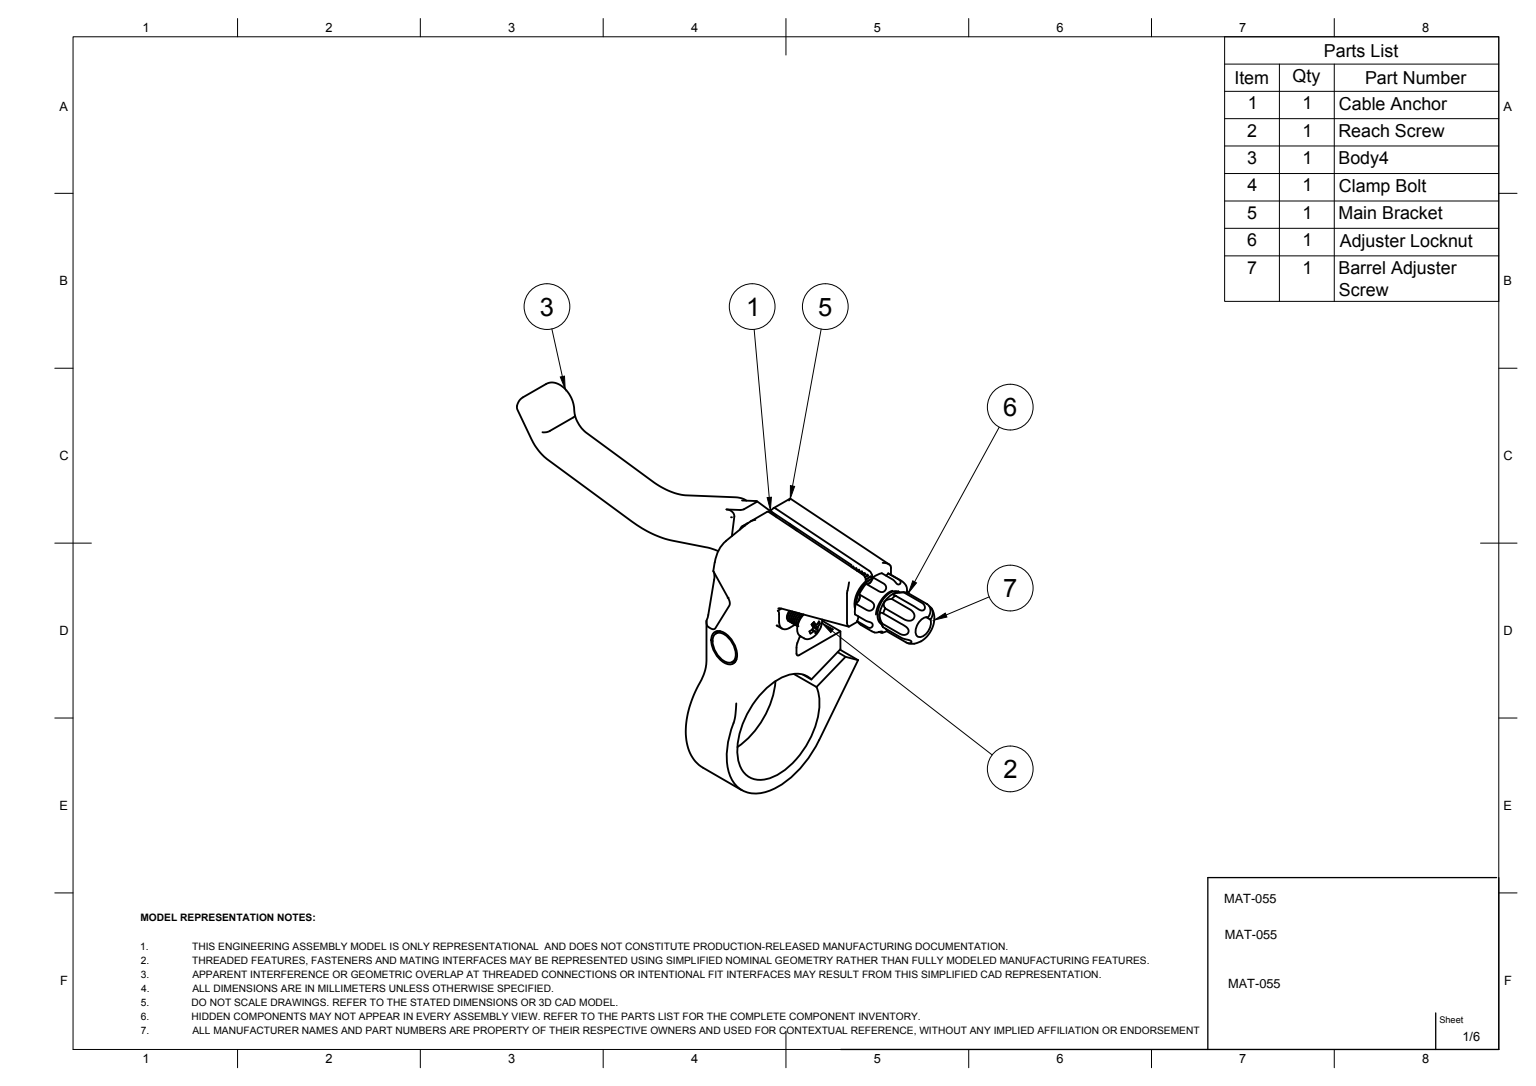
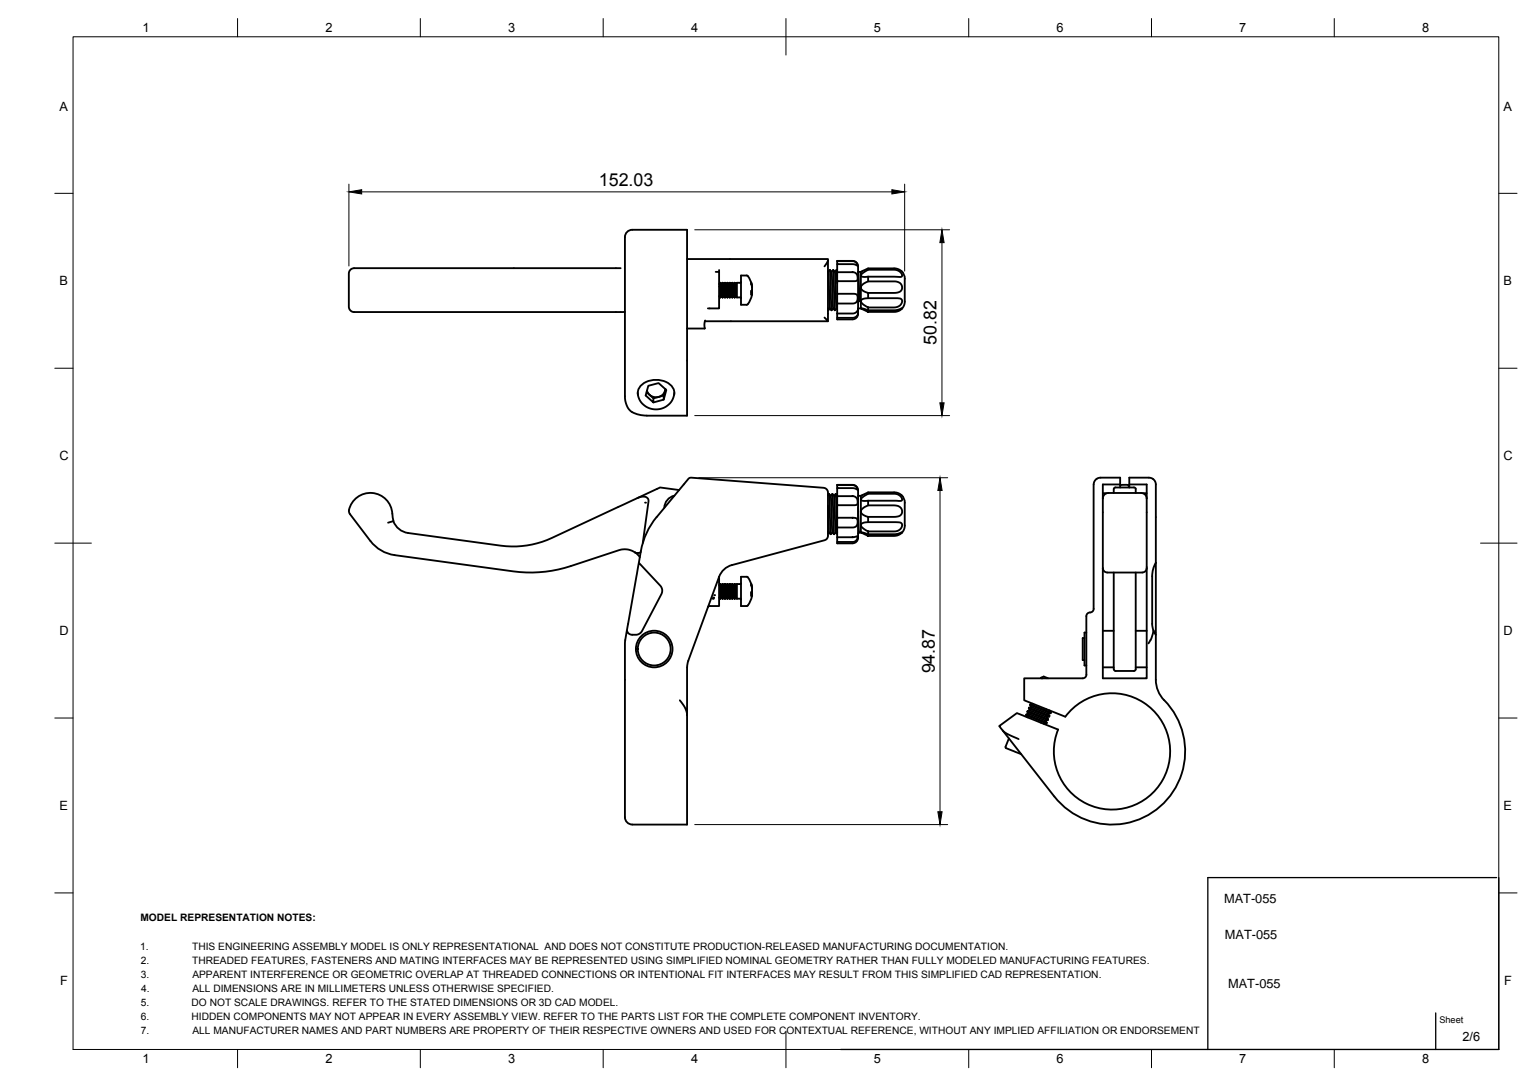
ISO-10303-21;
HEADER;
FILE_DESCRIPTION (('STEP AP214'),
    '1' );
FILE_NAME ('MAT-055',
    '2026-10-30T09:41:00',
    ( '' ),
    ( '' ),
    'SwSTEP 2.0',
    'SolidWorks 2020',
    '' );
FILE_SCHEMA (( 'AUTOMOTIVE_DESIGN' ));
ENDSEC;

DATA;
#1 = CARTESIAN_POINT ( 'NONE',  ( 110.9687390045248350, -9.868328341294098749, -11.32035403202665869 ) ) ;
#2 = LINE ( 'NONE', #2744, #42488 ) ;
#3 = ORIENTED_EDGE ( 'NONE', *, *, #32082, .F. ) ;
#4 = CARTESIAN_POINT ( 'NONE',  ( 113.1933481442453058, -4.089484607189486809, -7.948022111789456723 ) ) ;
#5 = CARTESIAN_POINT ( 'NONE',  ( 112.6260814775786514, -9.261995988541697145, -16.69588392320189030 ) ) ;
#6 = CARTESIAN_POINT ( 'NONE',  ( 122.0994348109119443, 0.9020085738987339008, -11.91225656197089222 ) ) ;
#7 = CARTESIAN_POINT ( 'NONE',  ( 116.4267681442453153, -6.222761293078241884, -8.102969835052219238 ) ) ;
#8 = DIRECTION ( 'NONE',  ( 1.000000000000000000, 0.000000000000000000, -0.000000000000000000 ) ) ;
#9 = CARTESIAN_POINT ( 'NONE',  ( 120.6245414775786458, -9.988377603198976828, -10.36322818467138340 ) ) ;
#10 = FACE_OUTER_BOUND ( 'NONE', #7467, .T. ) ;
#11 = CARTESIAN_POINT ( 'NONE',  ( 121.3619881442452879, -5.574606645277164318, -18.38911715685844683 ) ) ;
#12 = ORIENTED_EDGE ( 'NONE', *, *, #37026, .T. ) ;
#13 = CARTESIAN_POINT ( 'NONE',  ( 69.69189222814998175, -41.76310523276723785, -24.39321520033831447 ) ) ;
#14 = CIRCLE ( 'NONE', #29859, 2.000000000000000444 ) ;
#15 = CARTESIAN_POINT ( 'NONE',  ( 117.5613014775786525, 0.9020085738987339008, -11.91225656197089222 ) ) ;
#16 = CARTESIAN_POINT ( 'NONE',  ( 89.67401078471493747, -27.84333996136784961, -14.15691383771150136 ) ) ;
#17 = VERTEX_POINT ( 'NONE', #2774 ) ;
#18 = CARTESIAN_POINT ( 'NONE',  ( 123.0077516859119839, -9.665098340737509730, -17.37397104707595474 ) ) ;
#19 = CARTESIAN_POINT ( 'NONE',  ( 137.1799701741921922, -1.245005990108144500, -9.487437202584745322 ) ) ;
#20 = CARTESIAN_POINT ( 'NONE',  ( 121.4754414775786131, -8.166667518702819706, -8.995218007635861213 ) ) ;
#21 = CARTESIAN_POINT ( 'NONE',  ( 106.2459265045248173, -7.250697342233347165, -19.15521520033831138 ) ) ;
#22 = CARTESIAN_POINT ( 'NONE',  ( 119.6034614775786196, -3.505236298600246325, -18.68346056562440793 ) ) ;
#23 = ORIENTED_EDGE ( 'NONE', *, *, #16097, .T. ) ;
#24 = ORIENTED_EDGE ( 'NONE', *, *, #31128, .T. ) ;
#25 = CARTESIAN_POINT ( 'NONE',  ( 115.3489614775786407, -9.261995988541697145, -16.69588392320189030 ) ) ;
#26 = CYLINDRICAL_SURFACE ( 'NONE', #29939, 3.000000000000002665 ) ;
#27 = AXIS2_PLACEMENT_3D ( 'NONE', #14609, #30094, #23021 ) ;
#28 = DIRECTION ( 'NONE',  ( 0.000000000000000000, 0.000000000000000000, -1.000000000000000000 ) ) ;
#29 = EDGE_CURVE ( 'NONE', #24368, #33578, #9787, .T. ) ;
#30 = LINE ( 'NONE', #27854, #4652 ) ;
#31 = CARTESIAN_POINT ( 'NONE',  ( 121.5321681442453183, -9.988377603198976828, -10.36322818467138340 ) ) ;
#32 = CARTESIAN_POINT ( 'NONE',  ( 74.32979735608419958, -48.45188957854135481, -10.89321520033831447 ) ) ;
#33 = LINE ( 'NONE', #17589, #1125 ) ;
#34 = CARTESIAN_POINT ( 'NONE',  ( 122.3830681442452857, -8.166667518702819706, -8.995218007635861213 ) ) ;
#36 = CARTESIAN_POINT ( 'NONE',  ( 118.7525614775786380, -1.833838273342659253, -17.42832698103878286 ) ) ;
#35 = CARTESIAN_POINT ( 'NONE',  ( 120.3409081442453044, -0.4660016031367893996, -10.09054647747474043 ) ) ;
#37 = CARTESIAN_POINT ( 'NONE',  ( 121.2485348109119769, -8.899110576539710493, -16.42337572283490132 ) ) ;
#38 = DIRECTION ( 'NONE',  ( 0.9609149988134837450, -0.1028163501681639419, 0.2570431154366518145 ) ) ;
#39 = CARTESIAN_POINT ( 'NONE',  ( 114.9518748109119883, -1.834011780172310813, -8.268836392978581529 ) ) ;
#40 = EDGE_LOOP ( 'NONE', ( #5265, #23177, #27838, #18578 ) ) ;
#41 = CARTESIAN_POINT ( 'NONE',  ( 116.0834518517486771, -0.01906416985213849058, -12.14321520033831625 ) ) ;
#42 = CARTESIAN_POINT ( 'NONE',  ( 106.5237390045248418, 0.8980012041604421569, -15.77991374673208469 ) ) ;
#43 = CARTESIAN_POINT ( 'NONE',  ( 107.8433483795247838, -8.402594152722688392, -16.93181055722141792 ) ) ;
#44 = CARTESIAN_POINT ( 'NONE',  ( 105.4819421295248247, 0.8980012041604618078, -13.39321520033831447 ) ) ;
#45 = CARTESIAN_POINT ( 'NONE',  ( 125.3895814775786448, -7.893985811506177619, -18.51759400769804742 ) ) ;
#46 = CARTESIAN_POINT ( 'NONE',  ( 125.5597614775786326, -7.894159318335828068, -9.358103419637847864 ) ) ;
#47 = ORIENTED_EDGE ( 'NONE', *, *, #34668, .T. ) ;
#48 = CARTESIAN_POINT ( 'NONE',  ( 125.2761281442453054, -10.63000616557722466, -14.87417383870573495 ) ) ;
#49 = CARTESIAN_POINT ( 'NONE',  ( 111.3854577545248645, -7.250697342233347165, -7.631215200338321125 ) ) ;
#50 = DIRECTION ( 'NONE',  ( 0.000000000000000000, 0.000000000000000000, -1.000000000000000000 ) ) ;
#51 = ADVANCED_FACE ( 'NONE', ( #30593 ), #44511, .T. ) ;
#52 = CARTESIAN_POINT ( 'NONE',  ( 122.7234281442452755, -5.638512984488999180, -18.83840828888717311 ) ) ;
#53 = CARTESIAN_POINT ( 'NONE',  ( 125.8433948109119456, -1.834011780172310813, -8.268836392978581529 ) ) ;
#54 = CARTESIAN_POINT ( 'NONE',  ( 111.7184548109119788, -9.261995988541697145, -16.69588392320189030 ) ) ;
#55 = CARTESIAN_POINT ( 'NONE',  ( 116.0388171295248014, -10.62599879583958540, -13.39321520033831447 ) ) ;
#56 = CARTESIAN_POINT ( 'NONE',  ( 106.8710046295248759, -4.863998795839590272, -7.631215200338315796 ) ) ;
#57 = ORIENTED_EDGE ( 'NONE', *, *, #39925, .T. ) ;
#58 = DIRECTION ( 'NONE',  ( -0.000000000000000000, -0.9284778069183721172, -0.3713878862591650232 ) ) ;
#59 = AXIS2_PLACEMENT_3D ( 'NONE', #1011, #14251, #21539 ) ;
#60 = CARTESIAN_POINT ( 'NONE',  ( 116.8238548109119819, -5.574606645277164318, -18.38911715685844683 ) ) ;
#61 = CARTESIAN_POINT ( 'NONE',  ( 112.6260814775786514, -9.261995988541697145, -16.69588392320189030 ) ) ;
#62 = CARTESIAN_POINT ( 'NONE',  ( 115.7610046295247912, -4.863998795839590272, -7.631215200338315796 ) ) ;
#63 = CARTESIAN_POINT ( 'NONE',  ( 108.3295202545248657, 0.1403307496149616695, -11.32035403202665336 ) ) ;
#64 = AXIS2_PLACEMENT_3D ( 'NONE', #36243, #40129, #40585 ) ;
#65 = CARTESIAN_POINT ( 'NONE',  ( 120.9081748109119872, -4.153390946401325223, -8.397313243818185668 ) ) ;
#66 = CARTESIAN_POINT ( 'NONE',  ( 115.1787814775786387, -0.1624402480850797581, -16.17319339645315424 ) ) ;
#67 = CARTESIAN_POINT ( 'NONE',  ( 112.1155414775786454, -10.15424416112533912, -14.75197769757731336 ) ) ;
#68 = ORIENTED_EDGE ( 'NONE', *, *, #40399, .T. ) ;
#69 = CARTESIAN_POINT ( 'NONE',  ( 121.4103298109119748, -7.200787124940443817, -17.81845355600750835 ) ) ;
#70 = CARTESIAN_POINT ( 'NONE',  ( 124.5059548109119731, -5.999156839134619723, -18.26265215102738892 ) ) ;
#71 = CARTESIAN_POINT ( 'NONE',  ( 112.3991748109119868, -1.833838273342658809, -17.42832698103878286 ) ) ;
#72 = ORIENTED_EDGE ( 'NONE', *, *, #6315, .T. ) ;
#73 = CARTESIAN_POINT ( 'NONE',  ( 126.4750299824193007, -9.298013242772034559, -15.96981777986906970 ) ) ;
#74 = CARTESIAN_POINT ( 'NONE',  ( 112.6356140045247827, 0.1403307496149616695, -15.46607636864997204 ) ) ;
#75 = ORIENTED_EDGE ( 'NONE', *, *, #33478, .T. ) ;
#76 = AXIS2_PLACEMENT_3D ( 'NONE', #7945, #18211, #24609 ) ;
#77 = CARTESIAN_POINT ( 'NONE',  ( 116.8238548109119819, -5.574606645277164318, -18.38911715685844683 ) ) ;
#78 = CARTESIAN_POINT ( 'NONE',  ( 113.1933481442453058, -5.574606645277164318, -18.38911715685844683 ) ) ;
#79 = CARTESIAN_POINT ( 'NONE',  ( 112.8721930757767495, -0.9924539043446216624, -17.29976612834909133 ) ) ;
#80 = CARTESIAN_POINT ( 'NONE',  ( 123.7717360609119623, -3.387241619883791355, -18.17469012370385073 ) ) ;
#81 = ORIENTED_EDGE ( 'NONE', *, *, #25738, .F. ) ;
#82 = DIRECTION ( 'NONE',  ( 0.9609149988134837450, -0.1028163501681639419, 0.2570431154366518145 ) ) ;
#83 = CARTESIAN_POINT ( 'NONE',  ( 86.34560043013698305, -9.320000780048239619, -16.89321520033831447 ) ) ;
#84 = B_SPLINE_CURVE_WITH_KNOTS ( 'NONE', 3,
 ( #40412, #43376, #5506, #23076, #29462, #30146, #44061, #26048, #15786, #12373 ),
 .UNSPECIFIED., .F., .F.,
 ( 4, 2, 2, 2, 4 ),
 ( 0.000000000000000000, 0.0003215953659093761900, 0.0006431907318187523800, 0.0009647860977281285701, 0.001286381463637504760 ),
 .UNSPECIFIED. ) ;
#85 = CARTESIAN_POINT ( 'NONE',  ( 106.4542858795248179, -8.402594152722688392, -9.854619843455216355 ) ) ;
#86 = B_SPLINE_CURVE_WITH_KNOTS ( 'NONE', 3,
 ( #37430, #6200, #27183, #20122 ),
 .UNSPECIFIED., .F., .F.,
 ( 4, 4 ),
 ( 7.175310251266321521E-15, 2.533189092146110195E-06 ),
 .UNSPECIFIED. ) ;
#87 = FACE_OUTER_BOUND ( 'NONE', #1657, .T. ) ;
#88 = AXIS2_PLACEMENT_3D ( 'NONE', #42203, #35787, #10965 ) ;
#89 = CARTESIAN_POINT ( 'NONE',  ( 124.5954081442453116, -6.222761293078241884, -8.102969835052219238 ) ) ;
#90 = CARTESIAN_POINT ( 'NONE',  ( 116.8805814775786445, -3.505236298600246325, -18.68346056562440793 ) ) ;
#91 = CARTESIAN_POINT ( 'NONE',  ( 78.69189222814998175, -49.76310523276723785, -23.89321520033831803 ) ) ;
#92 = ORIENTED_EDGE ( 'NONE', *, *, #23975, .F. ) ;
#93 = CARTESIAN_POINT ( 'NONE',  ( 71.02242295334774269, -99.02728775972636299, -55.91838671430374319 ) ) ;
#94 = CARTESIAN_POINT ( 'NONE',  ( 117.0507614775786465, 0.1319031606808879209, -14.10382304977623669 ) ) ;
#95 = CARTESIAN_POINT ( 'NONE',  ( 119.7434548109119703, -3.132014511563818271, -18.68827187929387179 ) ) ;
#96 = CARTESIAN_POINT ( 'NONE',  ( 85.28386362106600416, -27.88924328735366132, -8.828750294274950505 ) ) ;
#97 = CARTESIAN_POINT ( 'NONE',  ( 125.5030348109119558, -3.383040157471821630, -19.15922257007629170 ) ) ;
#98 = EDGE_CURVE ( 'NONE', #12720, #5950, #1643, .T. ) ;
#99 = CARTESIAN_POINT ( 'NONE',  ( 113.5337081442453240, -9.261995988541697145, -16.69588392320189030 ) ) ;
#100 = ORIENTED_EDGE ( 'NONE', *, *, #14497, .T. ) ;
#101 = CARTESIAN_POINT ( 'NONE',  ( 112.7962614775786676, -3.383040157471821630, -19.15922257007629170 ) ) ;
#102 = CARTESIAN_POINT ( 'NONE',  ( 114.4980614775786592, -7.893985811506184724, -18.51759400769803676 ) ) ;
#103 = CARTESIAN_POINT ( 'NONE',  ( 111.6632702545248605, -10.62599879583958717, -15.77991374673208469 ) ) ;
#104 = CARTESIAN_POINT ( 'NONE',  ( 112.3424481442453384, -6.344957434206662583, -7.627207830600332805 ) ) ;
#105 = CARTESIAN_POINT ( 'NONE',  ( 114.4980614775786592, -7.893985811506177619, -18.51759400769804742 ) ) ;
#106 = CARTESIAN_POINT ( 'NONE',  ( 124.3685014775786328, 0.4262465694468514643, -12.03445270309931736 ) ) ;
#107 = CARTESIAN_POINT ( 'NONE',  ( 69.36136150295220659, -60.18712133882883819, -34.17284023871924603 ) ) ;
#108 = CARTESIAN_POINT ( 'NONE',  ( 108.5378796295247810, -4.863998795839590272, -8.388885654883775800 ) ) ;
#109 = DIRECTION ( 'NONE',  ( -1.000000000000000000, 0.000000000000000000, 0.000000000000000000 ) ) ;
#110 = CARTESIAN_POINT ( 'NONE',  ( 109.2294422165998071, -3.102175910333654585, -18.18453611788106983 ) ) ;
#111 = AXIS2_PLACEMENT_3D ( 'NONE', #10058, #13020, #24396 ) ;
#112 = CARTESIAN_POINT ( 'NONE',  ( 117.9583881442453048, 0.1319031606808879209, -14.10382304977623669 ) ) ;
#113 = CARTESIAN_POINT ( 'NONE',  ( 107.0099108795247815, -8.938348069036489818, -9.318865927141430916 ) ) ;
#114 = CARTESIAN_POINT ( 'NONE',  ( 115.2748327545248657, -6.936859964151250502, -8.388885654883777576 ) ) ;
#115 = CARTESIAN_POINT ( 'NONE',  ( 111.3854577545248645, -7.250697342233347165, -7.631215200338321125 ) ) ;
#116 = CARTESIAN_POINT ( 'NONE',  ( 128.2184548109119930, -5.622599431619523358, -7.441364641445410655 ) ) ;
#117 = CARTESIAN_POINT ( 'NONE',  ( 124.1983214775786166, -8.166667518702819706, -8.995218007635861213 ) ) ;
#118 = FACE_OUTER_BOUND ( 'NONE', #4304, .T. ) ;
#119 = CARTESIAN_POINT ( 'NONE',  ( 121.5888948109119809, -10.30919188438810075, -12.61870101168855918 ) ) ;
#120 = CARTESIAN_POINT ( 'NONE',  ( 117.9583881442453048, -10.30919188438810075, -12.61870101168855918 ) ) ;
#121 = ORIENTED_EDGE ( 'NONE', *, *, #26803, .F. ) ;
#122 = CARTESIAN_POINT ( 'NONE',  ( 115.6325948109119821, -9.565557343593413364, -10.61323700422348004 ) ) ;
#123 = CIRCLE ( 'NONE', #28512, 2.445500000000004448 ) ;
#124 = CARTESIAN_POINT ( 'NONE',  ( 122.0427081442452817, 0.5811942927096110934, -14.16772938898807510 ) ) ;
#126 = EDGE_CURVE ( 'NONE', #5046, #36034, #30866, .T. ) ;
#125 = CARTESIAN_POINT ( 'NONE',  ( 118.4689281442453392, 0.9020085738987339008, -11.91225656197089222 ) ) ;
#127 = CARTESIAN_POINT ( 'NONE',  ( 115.7460481442453357, -10.15424416112533912, -14.75197769757731336 ) ) ;
#128 = ORIENTED_EDGE ( 'NONE', *, *, #14994, .T. ) ;
#129 = CARTESIAN_POINT ( 'NONE',  ( 120.0572748109119772, -6.222761293078241884, -8.102969835052219238 ) ) ;
#130 = CARTESIAN_POINT ( 'NONE',  ( 115.0086014775786509, -4.089484607189486809, -7.948022111789456723 ) ) ;
#131 = CARTESIAN_POINT ( 'NONE',  ( 137.2359773051214802, 0.4104479539111648978, -13.25635893580179925 ) ) ;
#132 = CARTESIAN_POINT ( 'NONE',  ( 114.7192077545248594, -7.250697342233347165, -7.631215200338321125 ) ) ;
#133 = B_SPLINE_CURVE_WITH_KNOTS ( 'NONE', 3,
 ( #26160, #29806, #32757, #36631, #33206, #33421, #5174, #29130, #43042, #26387, #19321, #1981, #18865, #15907, #43720, #40297, #19544, #22961, #9061, #39624, #36853, #40065, #5622, #19092, #8163, #15001, #35960, #8830, #28914, #1530, #42824, #25494, #39398, #32977, #11810 ),
 .UNSPECIFIED., .F., .F.,
 ( 4, 2, 2, 1, 1, 2, 2, 1, 2, 2, 1, 1, 1, 1, 2, 2, 1, 1, 1, 1, 2, 2, 4 ),
 ( 0.000000000000000000, 0.06250000000002535472, 0.1250000000000507094, 0.1875000000000760503, 0.2187500000000859035, 0.2343750000000941469, 0.2500000000001023626, 0.3125000000001353362, 0.3281250000001413869, 0.3437500000001474376, 0.3750000000001494360, 0.4375000000001431633, 0.4687500000001400546, 0.4843750000001384448, 0.4921875000001327272, 0.5000000000001270095, 0.6250000000001643130, 0.6875000000001828537, 0.7187500000001921796, 0.7343750000001968425, 0.7421875000001944001, 0.7500000000001918465, 1.000000000000000000 ),
 .UNSPECIFIED. ) ;
#134 = DIRECTION ( 'NONE',  ( -0.000000000000000000, -0.9284778069183718952, -0.3713878862591649677 ) ) ;
#135 = CARTESIAN_POINT ( 'NONE',  ( 70.19189222814998175, -53.33815113939435548, -34.53808368179734600 ) ) ;
#136 = DIRECTION ( 'NONE',  ( 0.000000000000000000, -0.4669533266896233603, -0.8842819633428546933 ) ) ;
#137 = CARTESIAN_POINT ( 'NONE',  ( 114.9518748109119883, -1.834011780172310813, -8.268836392978581529 ) ) ;
#138 = LINE ( 'NONE', #803, #41193 ) ;
#139 = DIRECTION ( 'NONE',  ( 0.000000000000000000, 0.9242245927363041957, 0.3818493186865896116 ) ) ;
#140 = CARTESIAN_POINT ( 'NONE',  ( 63.90572062191856872, -12.84802420451643812, -16.01116961145836370 ) ) ;
#141 = CARTESIAN_POINT ( 'NONE',  ( 111.1767004682428848, 0.5115630086001619059, -14.64321520033833757 ) ) ;
#142 = CARTESIAN_POINT ( 'NONE',  ( 115.6915515045247531, -6.936859964151250502, -18.39754474579286025 ) ) ;
#143 = CARTESIAN_POINT ( 'NONE',  ( 116.9373081442452929, -8.166667518702817929, -8.995218007635861213 ) ) ;
#144 = DIRECTION ( 'NONE',  ( 0.000000000000000000, 0.000000000000000000, -1.000000000000000000 ) ) ;
#145 = CARTESIAN_POINT ( 'NONE',  ( 111.8528364273310274, -2.236191541394347837, -18.14152338500401385 ) ) ;
#146 = CARTESIAN_POINT ( 'NONE',  ( 118.4689281442453250, 0.9020085738987385637, -11.91225656197091887 ) ) ;
#147 = CARTESIAN_POINT ( 'NONE',  ( 125.0492214775786266, -3.505236298600246325, -18.68346056562440793 ) ) ;
#148 = ORIENTED_EDGE ( 'NONE', *, *, #1596, .T. ) ;
#149 = CARTESIAN_POINT ( 'NONE',  ( 136.0320772899156339, -9.514942969284794216, -9.745064694461806454 ) ) ;
#150 = CARTESIAN_POINT ( 'NONE',  ( 124.4252281442452812, -9.261995988541697145, -16.69588392320189030 ) ) ;
#151 = CARTESIAN_POINT ( 'NONE',  ( 125.9568481442452850, -6.344957434206665248, -7.627207830600338134 ) ) ;
#152 = CARTESIAN_POINT ( 'NONE',  ( 115.2355081442453155, 0.1319031606808879209, -14.10382304977623669 ) ) ;
#153 = CARTESIAN_POINT ( 'NONE',  ( 112.3424481442453384, -3.505236298600246325, -18.68346056562440793 ) ) ;
#154 = CARTESIAN_POINT ( 'NONE',  ( 74.47157298427187300, -3.053873105668316601, -12.39321520033831447 ) ) ;
#155 = CARTESIAN_POINT ( 'NONE',  ( 112.5661608795247872, -8.938348069036489818, -9.318865927141430916 ) ) ;
#156 = CARTESIAN_POINT ( 'NONE',  ( 119.1496481442453046, -6.222761293078241884, -8.102969835052219238 ) ) ;
#157 = CARTESIAN_POINT ( 'NONE',  ( 120.1707281442453166, -9.565557343593413364, -10.61323700422348004 ) ) ;
#158 = CARTESIAN_POINT ( 'NONE',  ( 109.2294420414169451, -0.008529726858385754465, -11.21375788622608560 ) ) ;
#159 = CARTESIAN_POINT ( 'NONE',  ( 122.9382985609119743, -10.36940331770106916, -15.09355782777062061 ) ) ;
#160 = CARTESIAN_POINT ( 'NONE',  ( 107.0793640045248196, 0.1403307496149616695, -15.46607636864997204 ) ) ;
#161 = DIRECTION ( 'NONE',  ( 0.000000000000000000, -0.3818493186865927203, 0.9242245927363029745 ) ) ;
#162 = CARTESIAN_POINT ( 'NONE',  ( 114.1577014775786552, -6.344957434206662583, -7.627207830600332805 ) ) ;
#163 = CARTESIAN_POINT ( 'NONE',  ( 113.3068014775786594, -8.166667518702817929, -8.995218007635859436 ) ) ;
#164 = CARTESIAN_POINT ( 'NONE',  ( 108.8851452545248151, 0.8980012041604421569, -11.00651665394454071 ) ) ;
#165 = DIRECTION ( 'NONE',  ( -0.9970811988817434024, 0.07634843047859724008, 0.000000000000000000 ) ) ;
#166 = VERTEX_POINT ( 'NONE', #36740 ) ;
#167 = CIRCLE ( 'NONE', #27232, 2.999999999999999556 ) ;
#168 = CARTESIAN_POINT ( 'NONE',  ( 123.3474214775786209, -9.988377603198976828, -10.36322818467138340 ) ) ;
#169 = AXIS2_PLACEMENT_3D ( 'NONE', #31050, #27866, #41779 ) ;
#170 = CARTESIAN_POINT ( 'NONE',  ( 112.3991748109119868, -8.166667518702817929, -8.995218007635859436 ) ) ;
#171 = CARTESIAN_POINT ( 'NONE',  ( 119.2063748109119814, -7.894159318335828068, -9.358103419637847864 ) ) ;
#172 = CARTESIAN_POINT ( 'NONE',  ( 124.9357681442453014, -1.834011780172310813, -8.268836392978581529 ) ) ;
#173 = CARTESIAN_POINT ( 'NONE',  ( 116.7104014775786425, -0.4660016031367893996, -10.09054647747474043 ) ) ;
#174 = CARTESIAN_POINT ( 'NONE',  ( 108.1906140045248037, 0.1403307496149616695, -15.46607636864997204 ) ) ;
#175 = AXIS2_PLACEMENT_3D ( 'NONE', #36006, #42871, #25989 ) ;
#176 = CARTESIAN_POINT ( 'NONE',  ( 111.6050014775786536, 0.1319031606808879209, -14.10382304977623669 ) ) ;
#177 = EDGE_LOOP ( 'NONE', ( #36537, #100, #20372, #6347 ) ) ;
#178 = CARTESIAN_POINT ( 'NONE',  ( 121.7023481442452777, -9.261995988541697145, -16.69588392320189030 ) ) ;
#179 = EDGE_CURVE ( 'NONE', #39765, #40221, #19962, .T. ) ;
#180 = CARTESIAN_POINT ( 'NONE',  ( 121.2019704359119743, 1.345710702986147034, -13.97328579221134426 ) ) ;
#181 = CARTESIAN_POINT ( 'NONE',  ( 114.2711548109119803, -9.988377603198976828, -10.36322818467138340 ) ) ;
#182 = EDGE_LOOP ( 'NONE', ( #10317, #8710, #12538, #23742 ) ) ;
#183 = CARTESIAN_POINT ( 'NONE',  ( 107.3571765045248299, -2.791137627527939813, -8.388885654883777576 ) ) ;
#184 = CARTESIAN_POINT ( 'NONE',  ( 124.0848681442452772, -4.089484607189486809, -7.948022111789456723 ) ) ;
#185 = CYLINDRICAL_SURFACE ( 'NONE', #31797, 1.499999999999999556 ) ;
#186 = CARTESIAN_POINT ( 'NONE',  ( 112.5693548109119888, 0.4262465694468514643, -12.03445270309931736 ) ) ;
#187 = CARTESIAN_POINT ( 'NONE',  ( 124.5059548109119731, -9.675232987814487373, -12.03232374619203249 ) ) ;
#188 =( BOUNDED_CURVE ( )  B_SPLINE_CURVE ( 3, ( #13503, #13725, #28295, #3452 ),
 .UNSPECIFIED., .F., .F. ) 
 B_SPLINE_CURVE_WITH_KNOTS ( ( 4, 4 ),
 ( 4.712388980384689674, 4.721492906269370238 ),
 .UNSPECIFIED. ) 
 CURVE ( )  GEOMETRIC_REPRESENTATION_ITEM ( )  RATIONAL_B_SPLINE_CURVE ( ( 1.000000000000000000, 0.9999930932230500780, 0.9999930932230500780, 1.000000000000000000 ) ) 
 REPRESENTATION_ITEM ( '' )  );
#189 = CARTESIAN_POINT ( 'NONE',  ( 119.4332814775786318, -8.899110576539710493, -16.42337572283490132 ) ) ;
#190 = CARTESIAN_POINT ( 'NONE',  ( 121.0408330757767459, -0.9924539043446216624, -17.29976612834909133 ) ) ;
#191 = CONICAL_SURFACE ( 'NONE', #23525, 2.999999999999999556, 0.9599310885968830309 ) ;
#192 = CARTESIAN_POINT ( 'NONE',  ( 120.7947214775786193, -0.8288870151387760510, -10.36305467784173118 ) ) ;
#193 = VECTOR ( 'NONE', #10934, 1000.000000000000114 ) ;
#194 = DIRECTION ( 'NONE',  ( -0.000000000000000000, -0.9284778069183721172, -0.3713878862591650232 ) ) ;
#195 = CARTESIAN_POINT ( 'NONE',  ( 119.4332814775786318, -8.899110576539710493, -16.42337572283490132 ) ) ;
#196 = CARTESIAN_POINT ( 'NONE',  ( 123.5633766859119760, -0.06289925094097943703, -9.412459353600674206 ) ) ;
#197 = CARTESIAN_POINT ( 'NONE',  ( 115.0653281442453277, -6.344957434206662583, -7.627207830600332805 ) ) ;
#198 = CARTESIAN_POINT ( 'NONE',  ( 123.3474214775786351, -9.988377603198957289, -10.36322818467135498 ) ) ;
#199 = CARTESIAN_POINT ( 'NONE',  ( 117.8449348109119938, -1.833838273342659253, -17.42832698103878286 ) ) ;
#200 = ORIENTED_EDGE ( 'NONE', *, *, #27729, .T. ) ;
#201 = CARTESIAN_POINT ( 'NONE',  ( 116.8805814775786445, -6.344957434206662583, -7.627207830600332805 ) ) ;
#202 = CARTESIAN_POINT ( 'NONE',  ( 106.8015515045248378, -2.477300249445798297, -7.631215200338321125 ) ) ;
#203 = EDGE_CURVE ( 'NONE', #36947, #44995, #9172, .T. ) ;
#204 = CARTESIAN_POINT ( 'NONE',  ( 70.47992290675011873, 2.032776587329049978, -16.39321520033831447 ) ) ;
#205 = AXIS2_PLACEMENT_3D ( 'NONE', #1914, #29739, #9001 ) ;
#206 = CARTESIAN_POINT ( 'NONE',  ( 90.99708770779186295, -25.99489077589524300, -13.39321520033831447 ) ) ;
#207 = CARTESIAN_POINT ( 'NONE',  ( 127.7184548109119788, -4.683672500039348208, -14.88233656108870662 ) ) ;
#208 = CARTESIAN_POINT ( 'NONE',  ( 121.2485348109119769, -0.4660016031367893996, -10.09054647747474043 ) ) ;
#209 = ORIENTED_EDGE ( 'NONE', *, *, #44836, .F. ) ;
#210 = CARTESIAN_POINT ( 'NONE',  ( 120.2510376736034345, -8.245233026025740486, -17.07659070123625611 ) ) ;
#211 = CARTESIAN_POINT ( 'NONE',  ( 118.0151148109119816, 0.4262465694468514643, -12.03445270309931736 ) ) ;
#212 = EDGE_CURVE ( 'NONE', #32579, #21740, #16699, .T. ) ;
#213 = CARTESIAN_POINT ( 'NONE',  ( 74.69189222814998175, -41.76310523276723785, -7.393215200338315363 ) ) ;
#214 = CARTESIAN_POINT ( 'NONE',  ( 64.04449450084898388, -15.08552066177155382, -16.37144510805424957 ) ) ;
#215 = DIRECTION ( 'NONE',  ( -0.1352586133457950590, -0.9908103287288504424, 0.000000000000000000 ) ) ;
#216 = EDGE_CURVE ( 'NONE', #33082, #17518, #26949, .T. ) ;
#217 = CARTESIAN_POINT ( 'NONE',  ( 110.5520202545248054, 0.1403307496149616695, -11.32035403202665336 ) ) ;
#218 = CARTESIAN_POINT ( 'NONE',  ( 89.13600071704317429, -10.42165226880396567, -14.07015947738872796 ) ) ;
#219 = VERTEX_POINT ( 'NONE', #5508 ) ;
#220 = CARTESIAN_POINT ( 'NONE',  ( 113.4769814775786330, -10.63000616557722466, -14.87417383870573495 ) ) ;
#221 = CARTESIAN_POINT ( 'NONE',  ( 124.5386814775786206, -4.153390946401325223, -8.397313243818185668 ) ) ;
#222 = CARTESIAN_POINT ( 'NONE',  ( 124.3685014775786328, -10.63000616557722466, -14.87417383870573495 ) ) ;
#223 = CARTESIAN_POINT ( 'NONE',  ( 115.6893214775786447, -9.859900752359374465, -12.68260735090039404 ) ) ;
#224 = LINE ( 'NONE', #17347, #39403 ) ;
#225 = CARTESIAN_POINT ( 'NONE',  ( 118.6391081442452986, -4.089484607189486809, -7.948022111789456723 ) ) ;
#226 = DIRECTION ( 'NONE',  ( 0.000000000000000000, 0.000000000000000000, -1.000000000000000000 ) ) ;
#227 = CYLINDRICAL_SURFACE ( 'NONE', #9190, 4.000000000000000000 ) ;
#228 = CARTESIAN_POINT ( 'NONE',  ( 122.8936081442453059, -9.565557343593413364, -10.61323700422348004 ) ) ;
#229 = ORIENTED_EDGE ( 'NONE', *, *, #20701, .T. ) ;
#230 = AXIS2_PLACEMENT_3D ( 'NONE', #1932, #32931, #26795 ) ;
#231 = CARTESIAN_POINT ( 'NONE',  ( 70.19189222814998175, -75.31442247550839397, -37.94335727672635983 ) ) ;
#232 = CONICAL_SURFACE ( 'NONE', #26442, 1.610000000000000986, 0.9599310885968765916 ) ;
#233 = CARTESIAN_POINT ( 'NONE',  ( 116.8805814775786445, -6.344957434206662583, -7.627207830600332805 ) ) ;
#234 = CARTESIAN_POINT ( 'NONE',  ( 136.3514896075913327, -8.489760904479810577, -17.93711134556155784 ) ) ;
#235 = ORIENTED_EDGE ( 'NONE', *, *, #33948, .T. ) ;
#236 = ADVANCED_FACE ( 'NONE', ( #2543, #19428 ), #16245, .T. ) ;
#237 = LINE ( 'NONE', #38306, #33556 ) ;
#238 = EDGE_CURVE ( 'NONE', #18481, #11704, #33042, .T. ) ;
#239 = ADVANCED_FACE ( 'NONE', ( #9623 ), #30148, .T. ) ;
#240 = CARTESIAN_POINT ( 'NONE',  ( 123.4608748109119745, -10.63000616557722466, -14.87417383870573495 ) ) ;
#241 = CARTESIAN_POINT ( 'NONE',  ( 77.77634386988368931, 3.254514819260763581, -19.39321520033831447 ) ) ;
#242 = CARTESIAN_POINT ( 'NONE',  ( 110.1353015045248469, -2.477300249445798297, -7.631215200338321125 ) ) ;
#243 = CARTESIAN_POINT ( 'NONE',  ( 121.4187148109119789, -3.505236298600246325, -18.68346056562440793 ) ) ;
#244 = EDGE_LOOP ( 'NONE', ( #3351, #8690, #1510, #25931, #38519, #27404, #20407, #392, #9598, #8626 ) ) ;
#245 = AXIS2_PLACEMENT_3D ( 'NONE', #38694, #8154, #22058 ) ;
#246 = ORIENTED_EDGE ( 'NONE', *, *, #30782, .T. ) ;
#247 = CARTESIAN_POINT ( 'NONE',  ( 113.6471614775786492, -5.638512984488999180, -18.83840828888717311 ) ) ;
#248 = CARTESIAN_POINT ( 'NONE',  ( 123.6310548109119765, -4.153390946401325223, -8.397313243818185668 ) ) ;
#249 = CARTESIAN_POINT ( 'NONE',  ( 112.7938987682628067, -1.040089454026971172, -17.23633227186634187 ) ) ;
#250 = CARTESIAN_POINT ( 'NONE',  ( 121.7023481442452777, -9.261995988541697145, -16.69588392320189030 ) ) ;
#251 = DIRECTION ( 'NONE',  ( 0.2768435750659263284, 0.3568721902840676363, -0.8921882507333129819 ) ) ;
#252 = CYLINDRICAL_SURFACE ( 'NONE', #41921, 3.000000000000001776 ) ;
#253 = CARTESIAN_POINT ( 'NONE',  ( 122.2696148109119889, -4.089484607189486809, -7.948022111789456723 ) ) ;
#255 = CARTESIAN_POINT ( 'NONE',  ( 123.2339681442453241, -3.505236298600246325, -18.68346056562440793 ) ) ;
#254 = CARTESIAN_POINT ( 'NONE',  ( 120.7947214775786193, -9.261995988541697145, -16.69588392320189030 ) ) ;
#256 = CARTESIAN_POINT ( 'NONE',  ( 118.8092881442453290, -0.1624402480850797581, -16.17319339645315424 ) ) ;
#257 = CARTESIAN_POINT ( 'NONE',  ( 64.46696884417693241, -15.35047623415474405, -15.89321305673442986 ) ) ;
#258 = CARTESIAN_POINT ( 'NONE',  ( 116.5402214775786405, 0.2603800115204892296, -16.42320221600525088 ) ) ;
#259 = VERTEX_POINT ( 'NONE', #5961 ) ;
#260 = VECTOR ( 'NONE', #38746, 1000.000000000000000 ) ;
#261 = DIRECTION ( 'NONE',  ( 1.000000000000000000, 0.000000000000000000, 0.000000000000000000 ) ) ;
#262 = CARTESIAN_POINT ( 'NONE',  ( 113.1217858795247935, -8.402594152722688392, -9.854619843455216355 ) ) ;
#263 = AXIS2_PLACEMENT_3D ( 'NONE', #1168, #7793, #17829 ) ;
#264 = CARTESIAN_POINT ( 'NONE',  ( 108.3989733795247759, -1.325403438956436419, -9.854619843455211026 ) ) ;
#265 = CARTESIAN_POINT ( 'NONE',  ( 113.7468640045248236, 0.1403307496149616695, -15.46607636864997204 ) ) ;
#266 = CARTESIAN_POINT ( 'NONE',  ( 125.3223148109119904, 0.3778260857404745487, -12.04688916545782185 ) ) ;
#267 = CARTESIAN_POINT ( 'NONE',  ( 125.1059481442452750, -1.833838273342660141, -17.42832698103878286 ) ) ;
#268 = EDGE_LOOP ( 'NONE', ( #6034, #39667, #9832, #29930 ) ) ;
#269 = CARTESIAN_POINT ( 'NONE',  ( 112.2857214775786474, -5.574606645277164318, -18.38911715685844683 ) ) ;
#270 = CARTESIAN_POINT ( 'NONE',  ( 110.9687390045248350, 0.8980012041604421569, -15.77991374673208469 ) ) ;
#271 = CARTESIAN_POINT ( 'NONE',  ( 91.77400275106518279, -25.99489077589524300, -13.39321520033831625 ) ) ;
#272 = CARTESIAN_POINT ( 'NONE',  ( 123.8012348109119642, 0.2603800115204892296, -16.42320221600525088 ) ) ;
#273 = CARTESIAN_POINT ( 'NONE',  ( 124.0281414775786146, -1.834011780172310813, -8.268836392978581529 ) ) ;
#274 = CARTESIAN_POINT ( 'NONE',  ( 119.9518141859119851, -8.321307733199551748, -9.223433127585318303 ) ) ;
#275 = CARTESIAN_POINT ( 'NONE',  ( 112.9097148109120070, 0.2603800115204892296, -16.42320221600525088 ) ) ;
#276 = EDGE_CURVE ( 'NONE', #36610, #20781, #19248, .T. ) ;
#277 = CARTESIAN_POINT ( 'NONE',  ( 115.2748327545248657, -2.477300249445798297, -19.15521520033831138 ) ) ;
#278 = CARTESIAN_POINT ( 'NONE',  ( 114.7886608795247696, -1.325403438956436419, -16.93181055722141792 ) ) ;
#279 = VERTEX_POINT ( 'NONE', #20785 ) ;
#280 = AXIS2_PLACEMENT_3D ( 'NONE', #38645, #14273, #42543 ) ;
#281 = CARTESIAN_POINT ( 'NONE',  ( 126.2202699136542350, -7.820588090633775025, -9.359791697047713299 ) ) ;
#282 = CARTESIAN_POINT ( 'NONE',  ( 114.4413348109119823, -0.8288870151387760510, -10.36305467784173118 ) ) ;
#283 = CARTESIAN_POINT ( 'NONE',  ( 126.1270281442452870, 0.1319031606808879209, -14.10382304977623669 ) ) ;
#284 = CARTESIAN_POINT ( 'NONE',  ( 113.3995983795247895, -0.7896495226426338832, -9.318865927141430916 ) ) ;
#285 = CARTESIAN_POINT ( 'NONE',  ( 107.4960827545248350, -6.936859964151250502, -8.388885654883777576 ) ) ;
#286 = CARTESIAN_POINT ( 'NONE',  ( 120.2841814775786276, -10.15424416112533912, -14.75197769757731336 ) ) ;
#287 = CARTESIAN_POINT ( 'NONE',  ( 119.0929214775786278, -4.153390946401325223, -8.397313243818185668 ) ) ;
#288 = CARTESIAN_POINT ( 'NONE',  ( 125.9001214775786224, -4.089484607189486809, -7.948022111789456723 ) ) ;
#289 = ORIENTED_EDGE ( 'NONE', *, *, #44643, .F. ) ;
#290 = CARTESIAN_POINT ( 'NONE',  ( 124.6521348109119884, -7.894159318335828068, -9.358103419637847864 ) ) ;
#291 = CARTESIAN_POINT ( 'NONE',  ( 27.57768543387103222, -14.97172645945875935, -19.39321520033831447 ) ) ;
#292 = CARTESIAN_POINT ( 'NONE',  ( 114.2144281442453178, -1.833838273342658809, -17.42832698103878286 ) ) ;
#293 = ORIENTED_EDGE ( 'NONE', *, *, #35379, .F. ) ;
#294 = CARTESIAN_POINT ( 'NONE',  ( 124.8328548109119822, -8.862178061931773598, -16.39564131203328401 ) ) ;
#295 = EDGE_CURVE ( 'NONE', #33939, #11904, #44743, .T. ) ;
#296 = CARTESIAN_POINT ( 'NONE',  ( 106.5931921295248372, 0.8980012041604618078, -13.39321520033831447 ) ) ;
#297 = CARTESIAN_POINT ( 'NONE',  ( 110.9687390045248350, -9.868328341294098749, -11.32035403202665869 ) ) ;
#298 = EDGE_LOOP ( 'NONE', ( #6324, #200, #13819, #23872, #43619, #8175, #10670, #40408, #38496, #9642, #19801, #11801, #12135, #8822, #43173 ) ) ;
#299 = CARTESIAN_POINT ( 'NONE',  ( 118.5823814775786360, -7.643976991954077427, -18.09477374809248928 ) ) ;
#300 = CARTESIAN_POINT ( 'NONE',  ( 113.8740681442453138, -9.859900752359374465, -12.68260735090039404 ) ) ;
#301 = EDGE_CURVE ( 'NONE', #24082, #31284, #22134, .T. ) ;
#302 = LINE ( 'NONE', #3715, #30421 ) ;
#303 = CARTESIAN_POINT ( 'NONE',  ( 123.7717360609119623, -6.564341423271550902, -7.887810678476487425 ) ) ;
#304 = ORIENTED_EDGE ( 'NONE', *, *, #43174, .F. ) ;
#305 = CARTESIAN_POINT ( 'NONE',  ( 74.32979735608419958, -48.45188957854135481, -10.39321520033831625 ) ) ;
#306 = DIRECTION ( 'NONE',  ( 0.000000000000000000, 0.7876185884367599144, -0.6161630946014909904 ) ) ;
#307 = CARTESIAN_POINT ( 'NONE',  ( 106.5931921295248372, -9.868328341294093420, -13.39321520033831447 ) ) ;
#308 = CARTESIAN_POINT ( 'NONE',  ( 114.1009748109119784, -4.089484607189486809, -7.948022111789456723 ) ) ;
#309 = CARTESIAN_POINT ( 'NONE',  ( 122.2696148109119889, -5.574606645277164318, -18.38911715685844683 ) ) ;
#310 = CARTESIAN_POINT ( 'NONE',  ( 116.3700414775786527, -4.153390946401321671, -8.397313243818183892 ) ) ;
#311 = FACE_OUTER_BOUND ( 'NONE', #28489, .T. ) ;
#312 = ORIENTED_EDGE ( 'NONE', *, *, #19134, .T. ) ;
#313 = CARTESIAN_POINT ( 'NONE',  ( 115.1787814775786387, -0.1624402480850797581, -16.17319339645315424 ) ) ;
#314 = AXIS2_PLACEMENT_3D ( 'NONE', #35221, #3555, #37996 ) ;
#315 = CARTESIAN_POINT ( 'NONE',  ( 121.9470836909669913, -25.99489077589524300, -13.39321520033831447 ) ) ;
#316 = LINE ( 'NONE', #14010, #39137 ) ;
#317 = CARTESIAN_POINT ( 'NONE',  ( 90.04708369096697140, -25.99489077589524300, -13.39321520033831447 ) ) ;
#318 = CARTESIAN_POINT ( 'NONE',  ( 116.5402214775786405, 0.2603800115204892296, -16.42320221600525088 ) ) ;
#319 = ORIENTED_EDGE ( 'NONE', *, *, #19756, .T. ) ;
#320 = CARTESIAN_POINT ( 'NONE',  ( 118.4689281442453392, 0.9020085738987339008, -11.91225656197089222 ) ) ;
#321 = LINE ( 'NONE', #35409, #15967 ) ;
#322 = CARTESIAN_POINT ( 'NONE',  ( 112.8439733795247832, -8.938348069036489818, -17.46756447353520159 ) ) ;
#323 = CARTESIAN_POINT ( 'NONE',  ( 113.3068014775786594, -8.166667518702817929, -8.995218007635859436 ) ) ;
#324 = CARTESIAN_POINT ( 'NONE',  ( 112.2289948109119848, -1.834011780172310813, -8.268836392978581529 ) ) ;
#326 = AXIS2_PLACEMENT_3D ( 'NONE', #2034, #13672, #6599 ) ;
#325 = CARTESIAN_POINT ( 'NONE',  ( 123.5743281442453139, -2.084020599724406786, -8.691656652584148546 ) ) ;
#327 = CARTESIAN_POINT ( 'NONE',  ( 111.7327233795247849, -1.325403438956533675, -9.854619843455175499 ) ) ;
#328 = CARTESIAN_POINT ( 'NONE',  ( 110.2047546295247855, -4.863998795839590272, -18.39754474579285315 ) ) ;
#329 = ORIENTED_EDGE ( 'NONE', *, *, #34728, .F. ) ;
#330 = CARTESIAN_POINT ( 'NONE',  ( 120.5887993777725029, -1.267766418764730840, -16.93314635290706605 ) ) ;
#331 = CARTESIAN_POINT ( 'NONE',  ( 109.2294421564239713, -3.315832619059893460, -18.27430022661860676 ) ) ;
#332 = CARTESIAN_POINT ( 'NONE',  ( 115.2355081442453155, 0.1319031606808879209, -14.10382304977623669 ) ) ;
#333 = CARTESIAN_POINT ( 'NONE',  ( 106.0375671295248310, -10.62599879583958540, -13.39321520033831447 ) ) ;
#334 = CARTESIAN_POINT ( 'NONE',  ( 114.4413952545248350, -9.868328341294098749, -15.46607636864997204 ) ) ;
#335 = CARTESIAN_POINT ( 'NONE',  ( 108.1906140045248463, -10.62599879583958717, -11.00651665394454604 ) ) ;
#336 = CARTESIAN_POINT ( 'NONE',  ( 66.06194382436763135, -14.97931106434683635, -7.393215200338315363 ) ) ;
#337 = CARTESIAN_POINT ( 'NONE',  ( 124.0281414775786146, -1.834011780172310813, -8.268836392978581529 ) ) ;
#338 = CARTESIAN_POINT ( 'NONE',  ( 71.37572422742091760, -11.86958442233774313, -21.89321520033831447 ) ) ;
#339 = CARTESIAN_POINT ( 'NONE',  ( 123.2339681442453241, -6.344957434206665248, -7.627207830600338134 ) ) ;
#340 = CARTESIAN_POINT ( 'NONE',  ( 116.0296814775786345, -8.166667518702817929, -8.995218007635861213 ) ) ;
#342 = ORIENTED_EDGE ( 'NONE', *, *, #31421, .T. ) ;
#341 = EDGE_CURVE ( 'NONE', #2225, #6245, #14383, .T. ) ;
#343 = CARTESIAN_POINT ( 'NONE',  ( 116.4267681442453153, -6.222761293078241884, -8.102969835052219238 ) ) ;
#344 = CARTESIAN_POINT ( 'NONE',  ( 113.1933481442453058, -4.089484607189486809, -7.948022111789456723 ) ) ;
#345 = CARTESIAN_POINT ( 'NONE',  ( 117.5045748109119756, 0.5811942927096110934, -14.16772938898807510 ) ) ;
#346 = CARTESIAN_POINT ( 'NONE',  ( 117.4478481442453131, -9.565557343593413364, -10.61323700422348004 ) ) ;
#347 = ORIENTED_EDGE ( 'NONE', *, *, #19251, .F. ) ;
#348 = CARTESIAN_POINT ( 'NONE',  ( 119.7736414775786358, 0.1319031606808879209, -14.10382304977623669 ) ) ;
#349 = AXIS2_PLACEMENT_3D ( 'NONE', #13047, #20117, #28 ) ;
#350 = CARTESIAN_POINT ( 'NONE',  ( 116.9940348109119839, -9.988377603198976828, -10.36322818467138340 ) ) ;
#351 = EDGE_CURVE ( 'NONE', #29699, #30236, #16925, .T. ) ;
#352 = CARTESIAN_POINT ( 'NONE',  ( 67.84197459855160162, -60.15404070048191443, -37.99358876332483703 ) ) ;
#353 = CARTESIAN_POINT ( 'NONE',  ( 107.9128015045248219, -2.477300249445798297, -7.631215200338321125 ) ) ;
#354 = B_SPLINE_CURVE_WITH_KNOTS ( 'NONE', 3,
 ( #21953, #36072, #29691, #15790, #25607, #25823, #22401, #36296, #1419, #40183 ),
 .UNSPECIFIED., .F., .F.,
 ( 4, 2, 2, 2, 4 ),
 ( 0.000000000000000000, 0.2500000000000000000, 0.5000000000000000000, 0.7500000000000000000, 1.000000000000000000 ),
 .UNSPECIFIED. ) ;
#355 = VECTOR ( 'NONE', #33888, 1000.000000000000000 ) ;
#356 = FACE_OUTER_BOUND ( 'NONE', #44787, .T. ) ;
#357 = DIRECTION ( 'NONE',  ( 1.000000000000000000, 0.000000000000000000, -0.000000000000000000 ) ) ;
#358 = CARTESIAN_POINT ( 'NONE',  ( 94.20708369096698220, -26.09538666226425363, -14.49867541642786861 ) ) ;
#359 = CARTESIAN_POINT ( 'NONE',  ( 113.0798948109119948, -0.4660016031367893996, -10.09054647747474043 ) ) ;
#360 = CARTESIAN_POINT ( 'NONE',  ( 90.93679655599923706, -18.80572346544368756, -20.89321520033831447 ) ) ;
#361 = CARTESIAN_POINT ( 'NONE',  ( 113.9307948109119764, -10.15424416112533912, -14.75197769757731336 ) ) ;
#362 = CARTESIAN_POINT ( 'NONE',  ( 61.78196040322745120, -12.46576002031727448, -17.04883285403948534 ) ) ;
#363 = CARTESIAN_POINT ( 'NONE',  ( 112.3324666496844912, 0.5600166689815611054, -12.14321520033829849 ) ) ;
#364 = CARTESIAN_POINT ( 'NONE',  ( 114.4413952545248350, -9.868328341294098749, -15.46607636864997204 ) ) ;
#365 = CARTESIAN_POINT ( 'NONE',  ( 113.8740681442453138, -9.859900752359374465, -12.68260735090039404 ) ) ;
#366 = CARTESIAN_POINT ( 'NONE',  ( 95.28169473643895060, -25.99489077589524300, -13.39321520033831447 ) ) ;
#367 = DIRECTION ( 'NONE',  ( -0.000000000000000000, -0.9284778069183718952, -0.3713878862591649677 ) ) ;
#368 = ADVANCED_FACE ( 'NONE', ( #7092 ), #38148, .T. ) ;
#370 = CARTESIAN_POINT ( 'NONE',  ( 114.3278814775786429, -10.30919188438810075, -12.61870101168855918 ) ) ;
#369 = FACE_OUTER_BOUND ( 'NONE', #21979, .T. ) ;
#371 = CARTESIAN_POINT ( 'NONE',  ( 124.6521348109119884, -7.894159318335828068, -9.358103419637847864 ) ) ;
#372 = CARTESIAN_POINT ( 'NONE',  ( 118.0151148109119816, 0.4262465694468514643, -12.03445270309931736 ) ) ;
#373 = ORIENTED_EDGE ( 'NONE', *, *, #35321, .F. ) ;
#374 = CARTESIAN_POINT ( 'NONE',  ( 125.5030348109119558, -3.383040157471821630, -19.15922257007629170 ) ) ;
#375 = CARTESIAN_POINT ( 'NONE',  ( 121.4187148109119789, -6.344957434206665248, -7.627207830600338134 ) ) ;
#376 = CARTESIAN_POINT ( 'NONE',  ( 116.3860827545247787, -6.936859964151250502, -8.388885654883777576 ) ) ;
#377 = CARTESIAN_POINT ( 'NONE',  ( 115.6893214775786447, -9.859900752359374465, -12.68260735090039404 ) ) ;
#378 = CARTESIAN_POINT ( 'NONE',  ( 111.7751814775786556, -2.084020599724406786, -8.691656652584148546 ) ) ;
#379 = CARTESIAN_POINT ( 'NONE',  ( 96.46827370896536991, -26.13949388144357755, -14.39191870720298994 ) ) ;
#380 = CARTESIAN_POINT ( 'NONE',  ( 114.3024890045248156, 0.8980012041604421569, -15.77991374673208469 ) ) ;
#381 = PRESENTATION_LAYER_ASSIGNMENT (  '', '', ( #30201 ) ) ;
#382 = CARTESIAN_POINT ( 'NONE',  ( 121.1350814775786233, -9.859900752359378018, -12.68260735090039759 ) ) ;
#383 = CARTESIAN_POINT ( 'NONE',  ( 119.9438214775786378, -2.084020599724406786, -8.691656652584148546 ) ) ;
#384 = CARTESIAN_POINT ( 'NONE',  ( 69.48536631248848039, -66.77523564985355620, -42.98127819198803934 ) ) ;
#385 = CARTESIAN_POINT ( 'NONE',  ( 120.0212673109119805, 0.2312338769422704887, -16.08380026872395874 ) ) ;
#386 = CARTESIAN_POINT ( 'NONE',  ( 108.3295202545248657, 0.1403307496149616695, -11.32035403202665336 ) ) ;
#387 = CARTESIAN_POINT ( 'NONE',  ( 117.1746850318387203, 1.411517391187495640, -21.51583517613059016 ) ) ;
#388 = CARTESIAN_POINT ( 'NONE',  ( 117.3343948109119737, -3.383040157471821630, -19.15922257007629170 ) ) ;
#389 = CARTESIAN_POINT ( 'NONE',  ( 115.0653281442453277, -6.344957434206662583, -7.627207830600332805 ) ) ;
#390 = CARTESIAN_POINT ( 'NONE',  ( 112.4272546295247821, -4.863998795839590272, -7.631215200338315796 ) ) ;
#391 = CARTESIAN_POINT ( 'NONE',  ( 112.2289948109119848, -1.834011780172310813, -8.268836392978581529 ) ) ;
#392 = ORIENTED_EDGE ( 'NONE', *, *, #6669, .F. ) ;
#393 = CARTESIAN_POINT ( 'NONE',  ( 117.2294421295247844, 1.035107641088057973, -21.89321520033831447 ) ) ;
#394 = CARTESIAN_POINT ( 'NONE',  ( 120.7947214775786193, -9.261995988541697145, -16.69588392320189030 ) ) ;
#395 = CARTESIAN_POINT ( 'NONE',  ( 114.8951481442453115, -0.4660016031367893996, -10.09054647747474043 ) ) ;
#396 = CARTESIAN_POINT ( 'NONE',  ( 120.6245414775786458, -0.1624402480850797581, -16.17319339645315424 ) ) ;
#397 = SURFACE_STYLE_FILL_AREA ( #24138 ) ;
#398 = CARTESIAN_POINT ( 'NONE',  ( 111.7751814775786556, -2.084020599724406786, -8.691656652584148546 ) ) ;
#399 = CARTESIAN_POINT ( 'NONE',  ( 121.0783548109119749, 0.2603800115204892296, -16.42320221600525088 ) ) ;
#400 = CARTESIAN_POINT ( 'NONE',  ( 106.7320983795247855, -8.402594152722688392, -16.93181055722141792 ) ) ;
#401 = EDGE_CURVE ( 'NONE', #31742, #38280, #42421, .T. ) ;
#402 = CARTESIAN_POINT ( 'NONE',  ( 115.6893214775786447, -9.859900752359374465, -12.68260735090039404 ) ) ;
#403 = CARTESIAN_POINT ( 'NONE',  ( 125.0375914802849024, -3.929494816607940422, -18.62311481910837685 ) ) ;
#404 = EDGE_LOOP ( 'NONE', ( #33107, #21221, #35400, #21094, #24132, #19976, #30122, #32334, #19696, #15366, #342, #5443, #42035, #39327, #5928, #9393, #16209, #25408, #27389, #31461 ) ) ;
#405 = CARTESIAN_POINT ( 'NONE',  ( 120.1707281442453166, 0.2603800115204892296, -16.42320221600525088 ) ) ;
#406 = CARTESIAN_POINT ( 'NONE',  ( 71.02242295334774269, -99.02728775972636299, -55.91838671430374319 ) ) ;
#407 = CARTESIAN_POINT ( 'NONE',  ( 118.1852948109119836, -5.638512984488999180, -18.83840828888717311 ) ) ;
#408 = VERTEX_POINT ( 'NONE', #41764 ) ;
#409 = CARTESIAN_POINT ( 'NONE',  ( 107.1488171295247867, 0.1403307496149613920, -13.39321520033831447 ) ) ;
#410 = DIRECTION ( 'NONE',  ( -1.000000000000000000, 0.000000000000000000, 0.000000000000000000 ) ) ;
#411 = CARTESIAN_POINT ( 'NONE',  ( 122.2696148109119889, -4.089484607189438847, -7.948022111789470934 ) ) ;
#412 = CARTESIAN_POINT ( 'NONE',  ( 114.4980614775786734, -2.084020599724406786, -8.691656652584148546 ) ) ;
#413 = CARTESIAN_POINT ( 'NONE',  ( 126.2184548109119788, -1.295815253274133161, -16.89579513612386563 ) ) ;
#414 = CARTESIAN_POINT ( 'NONE',  ( 118.2420214775786320, -6.222761293078241884, -8.102969835052219238 ) ) ;
#415 = CARTESIAN_POINT ( 'NONE',  ( 120.2122292294923938, -2.263366209404226392, -18.10533625161308180 ) ) ;
#416 = CIRCLE ( 'NONE', #25919, 2.999999999999999556 ) ;
#417 = CARTESIAN_POINT ( 'NONE',  ( 122.0427081442452817, -9.859900752359378018, -12.68260735090039759 ) ) ;
#418 = CARTESIAN_POINT ( 'NONE',  ( 124.7442371152574054, -12.24640110593768227, -10.93193462351065470 ) ) ;
#419 = CARTESIAN_POINT ( 'NONE',  ( 119.8870948109119752, -0.8288870151387760510, -10.36305467784173118 ) ) ;
#420 = CARTESIAN_POINT ( 'NONE',  ( 122.3132204359119868, 1.345710702986147034, -13.97328579221134426 ) ) ;
#421 = CARTESIAN_POINT ( 'NONE',  ( 114.4980614775786592, -7.893985811506177619, -18.51759400769804742 ) ) ;
#422 = DIRECTION ( 'NONE',  ( 1.000000000000000000, 0.000000000000000000, -0.000000000000000000 ) ) ;
#423 = CARTESIAN_POINT ( 'NONE',  ( 120.8514481442452961, -2.084020599724406786, -8.691656652584148546 ) ) ;
#424 = VERTEX_POINT ( 'NONE', #34228 ) ;
#425 = CARTESIAN_POINT ( 'NONE',  ( 117.5613014775786525, 0.9020085738987339008, -11.91225656197089222 ) ) ;
#426 = CARTESIAN_POINT ( 'NONE',  ( 113.6079577545248043, -2.791137627527939813, -18.39754474579286025 ) ) ;
#427 = FACE_OUTER_BOUND ( 'NONE', #35725, .T. ) ;
#428 = DIRECTION ( 'NONE',  ( 8.673617379884029556E-16, 1.000000000000000000, 0.000000000000000000 ) ) ;
#429 = DIRECTION ( 'NONE',  ( 1.387778780781445676E-17, -0.9284778069183720062, -0.3713878862591650232 ) ) ;
#430 = CIRCLE ( 'NONE', #37583, 1.200000000000000178 ) ;
#431 = CARTESIAN_POINT ( 'NONE',  ( 123.4608748109119745, -10.63000616557722466, -14.87417383870573495 ) ) ;
#432 = ORIENTED_EDGE ( 'NONE', *, *, #12226, .F. ) ;
#433 = CARTESIAN_POINT ( 'NONE',  ( 127.0298367773230979, -8.891943447879246065, -9.788057200751348219 ) ) ;
#434 = CARTESIAN_POINT ( 'NONE',  ( 120.9081748109119872, -4.153390946401325223, -8.397313243818185668 ) ) ;
#435 = FACE_OUTER_BOUND ( 'NONE', #25731, .T. ) ;
#436 = CARTESIAN_POINT ( 'NONE',  ( 62.89921056888596240, -13.37922507188889654, -18.73918694084264303 ) ) ;
#437 = CARTESIAN_POINT ( 'NONE',  ( 85.15861813568058380, -26.75858941326842810, -11.54476601486570964 ) ) ;
#438 = CARTESIAN_POINT ( 'NONE',  ( 110.2742077545248094, -2.791137627527939813, -18.39754474579286025 ) ) ;
#439 = DIRECTION ( 'NONE',  ( 1.000000000000000000, 0.000000000000000000, -0.000000000000000000 ) ) ;
#440 = AXIS2_PLACEMENT_3D ( 'NONE', #42881, #38535, #14611 ) ;
#441 = ORIENTED_EDGE ( 'NONE', *, *, #35642, .T. ) ;
#442 = CARTESIAN_POINT ( 'NONE',  ( 116.1431348109119881, -10.30919188438810075, -12.61870101168855918 ) ) ;
#443 = CARTESIAN_POINT ( 'NONE',  ( 124.9924948109119924, -5.574606645277164318, -18.38911715685844683 ) ) ;
#444 = CARTESIAN_POINT ( 'NONE',  ( 122.7801548109119665, -3.383040157471821630, -19.15922257007629170 ) ) ;
#445 = CARTESIAN_POINT ( 'NONE',  ( 117.6180281442453150, -8.899110576539710493, -16.42337572283490132 ) ) ;
#446 = CYLINDRICAL_SURFACE ( 'NONE', #37941, 1.499999999999996225 ) ;
#447 = CARTESIAN_POINT ( 'NONE',  ( 121.7023481442452777, -9.261995988541697145, -16.69588392320189030 ) ) ;
#448 = CARTESIAN_POINT ( 'NONE',  ( 123.8579614775786126, -9.859900752359374465, -12.68260735090038693 ) ) ;
#449 = CARTESIAN_POINT ( 'NONE',  ( 66.82415148905926117, -40.21211973637273474, -4.893215200338314474 ) ) ;
#450 = CARTESIAN_POINT ( 'NONE',  ( 109.9649712410415816, 0.7607806665038616689, -12.14321520033831625 ) ) ;
#451 = CARTESIAN_POINT ( 'NONE',  ( 123.0070614775786169, -10.15424416112533912, -14.75197769757731336 ) ) ;
#452 = VERTEX_POINT ( 'NONE', #31478 ) ;
#453 = AXIS2_PLACEMENT_3D ( 'NONE', #36071, #15337, #1637 ) ;
#454 = DIRECTION ( 'NONE',  ( -0.2768435750659241079, -0.3568721902840695792, 0.8921882507333129819 ) ) ;
#455 = CARTESIAN_POINT ( 'NONE',  ( 120.1707281442453166, 0.2603800115204892296, -16.42320221600525088 ) ) ;
#456 = CARTESIAN_POINT ( 'NONE',  ( 125.2761281442453054, 0.4262465694468514643, -12.03445270309931736 ) ) ;
#457 = ORIENTED_EDGE ( 'NONE', *, *, #36836, .F. ) ;
#458 =( BOUNDED_SURFACE ( )  B_SPLINE_SURFACE ( 1, 2, ( 
 ( #7146, #28584, #982, #21057, #38826, #7830, #25389, #7368, #746, #32433, #29027, #42716, #18090, #8052, #14669, #535, #42494, #38591, #10586, #34935, #3943, #35846, #14444, #35396, #28137, #31539, #24485, #28352, #14222, #11253, #4172, #39058, #21736, #35625, #35167, #17641, #21956, #4399, #11483, #18315, #18541, #42265, #308, #1207, #15121, #42045, #10806, #24701, #21281, #16248, #33317, #5066, #26508, #19213, #12381, #12151, #36075, #25611, #16017, #9176, #29467, #39958, #43383, #43605, #8501, #23083, #39732, #11700, #15792, #39513, #4846, #26054, #5297, #8720, #29694, #22405, #8277, #36964, #36524, #2091, #22626, #36744, #36298, #22179, #5512, #33093, #2320, #18765, #32654, #42938, #1421, #29925, #18982, #40416, #1862, #26279, #40187, #15341, #29250, #43839, #5735, #8953, #22853, #19431, #12606, #32871, #19654, #1640, #43159, #33541, #11926, #25825, #15564, #37885, #37431, #30151, #16473, #38105, #44298, #23548, #13507, #3229, #16929, #26732, #27415, #26952, #13729, #5965, #27638, #6661, #2546, #40874, #2779, #23773, #30824, #44067, #40641, #24214, #3456, #44972, #10312, #9627, #41335, #17155, #13053, #41552, #10094, #44748, #6201, #12833, #6880, #37665, #34670, #9396, #20123, #16704, #30376, #34233, #34008, #23997, #6440, #20349, #20790, #33776, #30598, #27186, #44515, #3007, #23307, #37191, #20571, #34448, #19889, #13280, #31042, #41106, #9864, #7537, #39226, #35793, #39000, #24875, #14841, #21454, #7311, #35337, #253, #17373, #34, #10753, #42656, #24651, #42211, #34881, #38320, #31261, #38536, #21007, #18030, #31704, #14612, #32154, #14162, #4109, #7991, #13946, #7770, #38767, #28751, #31927, #21230, #692, #28080, #27859, #41769, #35109, #11427, #3890, #10972, #3669, #7097, #10529, #17810, #17590, #28529, #474, #42435, #28299, #11199, #41988, #24428, #25333, #25104, #21677, #35565, #4337, #14387, #31483, #18258, #922, #21899, #11642, #25552, #4565, #23024, #40131, #11872, #33266, #26002, #19155, #18929, #42882, #32379, #22794, #15964, #36245, #1587 ),
 ( #39458, #12322, #26221, #25776, #18489, #36021, #12548, #18710, #43102, #33036, #36688, #36472, #1146, #1811, #1371, #2040, #8222, #29867, #8896, #22128, #15282, #22351, #43329, #5239, #15063, #28977, #43783, #4789, #19378, #26455, #29190, #15738, #5458, #32600, #40357, #29640, #43554, #39683, #8448, #9121, #12098, #5012, #32817, #15508, #29415, #39906, #8667, #22569, #37608, #30540, #44461, #13676, #40587, #19835, #33953, #9575, #9809, #20517, #33486, #23718, #27358, #2264, #5913, #17101, #13227, #16192, #27584, #16646, #30096, #41278, #44012, #30768, #37825, #27128, #33722, #44919, #26899, #41499, #12774, #41052, #9346, #30317, #2492, #37139, #16421, #44694, #34174, #23255, #10037, #13454, #34397, #44243, #23945, #20067, #26676, #13001, #37377, #40819, #19602, #6382, #10255, #36912, #5683, #20290, #23491, #2949, #6147, #2720, #16877, #6603, #3178, #30993, #24601, #35279, #31211, #10919, #14111, #642, #24819, #35511, #45134, #20958, #35050, #14557, #21175, #28475, #17754, #32099, #20737, #24162, #3834, #13893, #867, #21399, #4053, #31877, #7479, #14335, #18202, #11144, #42380, #10698, #28700, #25047, #195, #38942, #17977, #7710, #21623, #31651, #4283, #14786, #419, #28027, #42604, #38054, #10479, #17531, #28249, #42158, #38711, #34830, #6832, #34617, #3404, #17321, #41715, #27800, #24380, #38266, #41935, #7047, #3615, #31428, #38484, #7259, #22739, #4960, #8840, #5183, #22299, #36641, #19100, #35967, #32987, #1761, #42830, #15687, #29138, #32765, #29589, #11817, #15916, #18439, #32328, #11370, #29814, #43507, #18658, #40076, #1538, #25949, #25725, #4516, #39172, #12275, #5414, #43050, #8395, #15460, #39632, #29366, #19330, #8169, #25276, #43277, #7936, #1094, #26171, #33216, #32548, #21847, #11591, #1990, #25501, #4737, #39856, #35742, #12046, #15009, #8621, #22079, #28923, #39405, #1318, #15229, #36196, #18874, #22518, #36416, #44410, #12498, #9070, #38380, #17649, #14008, #24495, #40536, #27078, #31320, #12719, #10593, #9753, #13176, #26622, #43730, #7153 ) ),
 .UNSPECIFIED., .F., .F., .F. ) 
 B_SPLINE_SURFACE_WITH_KNOTS ( ( 2, 2 ),
 ( 3, 2, 2, 2, 2, 2, 2, 2, 2, 2, 2, 2, 2, 2, 2, 2, 2, 2, 2, 2, 2, 2, 2, 2, 2, 2, 2, 2, 2, 2, 2, 2, 2, 2, 2, 2, 2, 2, 2, 2, 2, 2, 2, 2, 2, 2, 2, 2, 2, 2, 2, 2, 2, 2, 2, 2, 2, 2, 2, 2, 2, 2, 2, 2, 2, 2, 2, 2, 2, 2, 2, 2, 2, 2, 2, 2, 2, 2, 2, 2, 2, 2, 2, 2, 2, 2, 2, 2, 2, 2, 2, 2, 2, 2, 2, 2, 2, 2, 2, 2, 2, 2, 2, 2, 2, 2, 2, 2, 2, 2, 2, 2, 2, 2, 2, 2, 2, 2, 2, 2, 2, 2, 2, 2, 2, 2, 2, 2, 3 ),
 ( 0.000000000000000000, 1.000000000000000000 ),
 ( 0.000000000000000000, 0.007812500000000000000, 0.01562500000000000000, 0.02343750000000000000, 0.03125000000000000000, 0.03906250000000000000, 0.04687500000000000000, 0.05468750000000000000, 0.06250000000000000000, 0.07031250000000000000, 0.07812500000000000000, 0.08593750000000000000, 0.09375000000000000000, 0.1015625000000000000, 0.1093750000000000000, 0.1171875000000000000, 0.1250000000000000000, 0.1328125000000000000, 0.1406250000000000000, 0.1484375000000000000, 0.1562500000000000000, 0.1640625000000000000, 0.1718750000000000000, 0.1796875000000000000, 0.1875000000000000000, 0.1953125000000000000, 0.2031250000000000000, 0.2109375000000000000, 0.2187500000000000000, 0.2265625000000000000, 0.2343750000000000000, 0.2421875000000000000, 0.2500000000000000000, 0.2578125000000000000, 0.2656250000000000000, 0.2734375000000000000, 0.2812500000000000000, 0.2890625000000000000, 0.2968750000000000000, 0.3046875000000000000, 0.3125000000000000000, 0.3203125000000000000, 0.3281250000000000000, 0.3359375000000000000, 0.3437500000000000000, 0.3515625000000000000, 0.3593750000000000000, 0.3671875000000000000, 0.3750000000000000000, 0.3828125000000000000, 0.3906250000000000000, 0.3984375000000000000, 0.4062500000000000000, 0.4140625000000000000, 0.4218750000000000000, 0.4296875000000000000, 0.4375000000000000000, 0.4453125000000000000, 0.4531250000000000000, 0.4609375000000000000, 0.4687500000000000000, 0.4765625000000000000, 0.4843750000000000000, 0.4921875000000000000, 0.5000000000000000000, 0.5078125000000000000, 0.5156250000000000000, 0.5234375000000000000, 0.5312500000000000000, 0.5390625000000000000, 0.5468750000000000000, 0.5546875000000000000, 0.5625000000000000000, 0.5703125000000000000, 0.5781250000000000000, 0.5859375000000000000, 0.5937500000000000000, 0.6015625000000000000, 0.6093750000000000000, 0.6171875000000000000, 0.6250000000000000000, 0.6328125000000000000, 0.6406250000000000000, 0.6484375000000000000, 0.6562500000000000000, 0.6640625000000000000, 0.6718750000000000000, 0.6796875000000000000, 0.6875000000000000000, 0.6953125000000000000, 0.7031250000000000000, 0.7109375000000000000, 0.7187500000000000000, 0.7265625000000000000, 0.7343750000000000000, 0.7421875000000000000, 0.7500000000000000000, 0.7578125000000000000, 0.7656250000000000000, 0.7734375000000000000, 0.7812500000000000000, 0.7890625000000000000, 0.7968750000000000000, 0.8046875000000000000, 0.8125000000000000000, 0.8203125000000000000, 0.8281250000000000000, 0.8359375000000000000, 0.8437500000000000000, 0.8515625000000000000, 0.8593750000000000000, 0.8671875000000000000, 0.8750000000000000000, 0.8828125000000000000, 0.8906250000000000000, 0.8984375000000000000, 0.9062500000000000000, 0.9140625000000000000, 0.9218750000000000000, 0.9296875000000000000, 0.9375000000000000000, 0.9453125000000000000, 0.9531250000000000000, 0.9609375000000000000, 0.9687500000000000000, 0.9765625000000000000, 0.9843750000000000000, 0.9921875000000000000, 1.000000000000000000 ),
 .UNSPECIFIED. ) 
 GEOMETRIC_REPRESENTATION_ITEM ( )  RATIONAL_B_SPLINE_SURFACE ( (
 ( 1.000000000000000000, 0.9238795325112869605, 1.000000000000000000, 0.9238795325112869605, 1.000000000000000000, 0.9238795325112869605, 1.000000000000000000, 0.9238795325112869605, 1.000000000000000000, 0.9238795325112869605, 1.000000000000000000, 0.9238795325112869605, 1.000000000000000000, 0.9238795325112869605, 1.000000000000000000, 0.9238795325112869605, 1.000000000000000000, 0.9238795325112869605, 1.000000000000000000, 0.9238795325112869605, 1.000000000000000000, 0.9238795325112869605, 1.000000000000000000, 0.9238795325112869605, 1.000000000000000000, 0.9238795325112869605, 1.000000000000000000, 0.9238795325112869605, 1.000000000000000000, 0.9238795325112869605, 1.000000000000000000, 0.9238795325112869605, 1.000000000000000000, 0.9238795325112869605, 1.000000000000000000, 0.9238795325112869605, 1.000000000000000000, 0.9238795325112869605, 1.000000000000000000, 0.9238795325112869605, 1.000000000000000000, 0.9238795325112869605, 1.000000000000000000, 0.9238795325112869605, 1.000000000000000000, 0.9238795325112869605, 1.000000000000000000, 0.9238795325112869605, 1.000000000000000000, 0.9238795325112869605, 1.000000000000000000, 0.9238795325112869605, 1.000000000000000000, 0.9238795325112869605, 1.000000000000000000, 0.9238795325112869605, 1.000000000000000000, 0.9238795325112869605, 1.000000000000000000, 0.9238795325112869605, 1.000000000000000000, 0.9238795325112869605, 1.000000000000000000, 0.9238795325112869605, 1.000000000000000000, 0.9238795325112869605, 1.000000000000000000, 0.9238795325112869605, 1.000000000000000000, 0.9238795325112869605, 1.000000000000000000, 0.9238795325112869605, 1.000000000000000000, 0.9238795325112869605, 1.000000000000000000, 0.9238795325112869605, 1.000000000000000000, 0.9238795325112869605, 1.000000000000000000, 0.9238795325112869605, 1.000000000000000000, 0.9238795325112869605, 1.000000000000000000, 0.9238795325112869605, 1.000000000000000000, 0.9238795325112869605, 1.000000000000000000, 0.9238795325112869605, 1.000000000000000000, 0.9238795325112869605, 1.000000000000000000, 0.9238795325112869605, 1.000000000000000000, 0.9238795325112869605, 1.000000000000000000, 0.9238795325112869605, 1.000000000000000000, 0.9238795325112869605, 1.000000000000000000, 0.9238795325112869605, 1.000000000000000000, 0.9238795325112869605, 1.000000000000000000, 0.9238795325112869605, 1.000000000000000000, 0.9238795325112869605, 1.000000000000000000, 0.9238795325112869605, 1.000000000000000000, 0.9238795325112869605, 1.000000000000000000, 0.9238795325112869605, 1.000000000000000000, 0.9238795325112869605, 1.000000000000000000, 0.9238795325112869605, 1.000000000000000000, 0.9238795325112869605, 1.000000000000000000, 0.9238795325112869605, 1.000000000000000000, 0.9238795325112869605, 1.000000000000000000, 0.9238795325112869605, 1.000000000000000000, 0.9238795325112869605, 1.000000000000000000, 0.9238795325112869605, 1.000000000000000000, 0.9238795325112869605, 1.000000000000000000, 0.9238795325112869605, 1.000000000000000000, 0.9238795325112869605, 1.000000000000000000, 0.9238795325112869605, 1.000000000000000000, 0.9238795325112869605, 1.000000000000000000, 0.9238795325112869605, 1.000000000000000000, 0.9238795325112869605, 1.000000000000000000, 0.9238795325112869605, 1.000000000000000000, 0.9238795325112869605, 1.000000000000000000, 0.9238795325112869605, 1.000000000000000000, 0.9238795325112869605, 1.000000000000000000, 0.9238795325112869605, 1.000000000000000000, 0.9238795325112869605, 1.000000000000000000, 0.9238795325112869605, 1.000000000000000000, 0.9238795325112869605, 1.000000000000000000, 0.9238795325112869605, 1.000000000000000000, 0.9238795325112869605, 1.000000000000000000, 0.9238795325112869605, 1.000000000000000000, 0.9238795325112869605, 1.000000000000000000, 0.9238795325112869605, 1.000000000000000000, 0.9238795325112869605, 1.000000000000000000, 0.9238795325112869605, 1.000000000000000000, 0.9238795325112869605, 1.000000000000000000, 0.9238795325112869605, 1.000000000000000000, 0.9238795325112869605, 1.000000000000000000, 0.9238795325112869605, 1.000000000000000000, 0.9238795325112869605, 1.000000000000000000, 0.9238795325112869605, 1.000000000000000000, 0.9238795325112869605, 1.000000000000000000, 0.9238795325112869605, 1.000000000000000000, 0.9238795325112869605, 1.000000000000000000, 0.9238795325112869605, 1.000000000000000000, 0.9238795325112869605, 1.000000000000000000, 0.9238795325112869605, 1.000000000000000000, 0.9238795325112869605, 1.000000000000000000, 0.9238795325112869605, 1.000000000000000000, 0.9238795325112869605, 1.000000000000000000, 0.9238795325112869605, 1.000000000000000000, 0.9238795325112869605, 1.000000000000000000, 0.9238795325112869605, 1.000000000000000000, 0.9238795325112869605, 1.000000000000000000, 0.9238795325112869605, 1.000000000000000000, 0.9238795325112869605, 1.000000000000000000, 0.9238795325112869605, 1.000000000000000000, 0.9238795325112869605, 1.000000000000000000, 0.9238795325112869605, 1.000000000000000000, 0.9238795325112869605, 1.000000000000000000, 0.9238795325112869605, 1.000000000000000000, 0.9238795325112869605, 1.000000000000000000, 0.9238795325112869605, 1.000000000000000000, 0.9238795325112869605, 1.000000000000000000, 0.9238795325112869605, 1.000000000000000000, 0.9238795325112869605, 1.000000000000000000, 0.9238795325112869605, 1.000000000000000000, 0.9238795325112869605, 1.000000000000000000, 0.9238795325112869605, 1.000000000000000000, 0.9238795325112869605, 1.000000000000000000, 0.9238795325112869605, 1.000000000000000000, 0.9238795325112869605, 1.000000000000000000, 0.9238795325112869605, 1.000000000000000000, 0.9238795325112869605, 1.000000000000000000, 0.9238795325112869605, 1.000000000000000000, 0.9238795325112869605, 1.000000000000000000, 0.9238795325112869605, 1.000000000000000000),
 ( 1.000000000000000000, 0.9238795325112869605, 1.000000000000000000, 0.9238795325112869605, 1.000000000000000000, 0.9238795325112869605, 1.000000000000000000, 0.9238795325112869605, 1.000000000000000000, 0.9238795325112869605, 1.000000000000000000, 0.9238795325112869605, 1.000000000000000000, 0.9238795325112869605, 1.000000000000000000, 0.9238795325112869605, 1.000000000000000000, 0.9238795325112869605, 1.000000000000000000, 0.9238795325112869605, 1.000000000000000000, 0.9238795325112869605, 1.000000000000000000, 0.9238795325112869605, 1.000000000000000000, 0.9238795325112869605, 1.000000000000000000, 0.9238795325112869605, 1.000000000000000000, 0.9238795325112869605, 1.000000000000000000, 0.9238795325112869605, 1.000000000000000000, 0.9238795325112869605, 1.000000000000000000, 0.9238795325112869605, 1.000000000000000000, 0.9238795325112869605, 1.000000000000000000, 0.9238795325112869605, 1.000000000000000000, 0.9238795325112869605, 1.000000000000000000, 0.9238795325112869605, 1.000000000000000000, 0.9238795325112869605, 1.000000000000000000, 0.9238795325112869605, 1.000000000000000000, 0.9238795325112869605, 1.000000000000000000, 0.9238795325112869605, 1.000000000000000000, 0.9238795325112869605, 1.000000000000000000, 0.9238795325112869605, 1.000000000000000000, 0.9238795325112869605, 1.000000000000000000, 0.9238795325112869605, 1.000000000000000000, 0.9238795325112869605, 1.000000000000000000, 0.9238795325112869605, 1.000000000000000000, 0.9238795325112869605, 1.000000000000000000, 0.9238795325112869605, 1.000000000000000000, 0.9238795325112869605, 1.000000000000000000, 0.9238795325112869605, 1.000000000000000000, 0.9238795325112869605, 1.000000000000000000, 0.9238795325112869605, 1.000000000000000000, 0.9238795325112869605, 1.000000000000000000, 0.9238795325112869605, 1.000000000000000000, 0.9238795325112869605, 1.000000000000000000, 0.9238795325112869605, 1.000000000000000000, 0.9238795325112869605, 1.000000000000000000, 0.9238795325112869605, 1.000000000000000000, 0.9238795325112869605, 1.000000000000000000, 0.9238795325112869605, 1.000000000000000000, 0.9238795325112869605, 1.000000000000000000, 0.9238795325112869605, 1.000000000000000000, 0.9238795325112869605, 1.000000000000000000, 0.9238795325112869605, 1.000000000000000000, 0.9238795325112869605, 1.000000000000000000, 0.9238795325112869605, 1.000000000000000000, 0.9238795325112869605, 1.000000000000000000, 0.9238795325112869605, 1.000000000000000000, 0.9238795325112869605, 1.000000000000000000, 0.9238795325112869605, 1.000000000000000000, 0.9238795325112869605, 1.000000000000000000, 0.9238795325112869605, 1.000000000000000000, 0.9238795325112869605, 1.000000000000000000, 0.9238795325112869605, 1.000000000000000000, 0.9238795325112869605, 1.000000000000000000, 0.9238795325112869605, 1.000000000000000000, 0.9238795325112869605, 1.000000000000000000, 0.9238795325112869605, 1.000000000000000000, 0.9238795325112869605, 1.000000000000000000, 0.9238795325112869605, 1.000000000000000000, 0.9238795325112869605, 1.000000000000000000, 0.9238795325112869605, 1.000000000000000000, 0.9238795325112869605, 1.000000000000000000, 0.9238795325112869605, 1.000000000000000000, 0.9238795325112869605, 1.000000000000000000, 0.9238795325112869605, 1.000000000000000000, 0.9238795325112869605, 1.000000000000000000, 0.9238795325112869605, 1.000000000000000000, 0.9238795325112869605, 1.000000000000000000, 0.9238795325112869605, 1.000000000000000000, 0.9238795325112869605, 1.000000000000000000, 0.9238795325112869605, 1.000000000000000000, 0.9238795325112869605, 1.000000000000000000, 0.9238795325112869605, 1.000000000000000000, 0.9238795325112869605, 1.000000000000000000, 0.9238795325112869605, 1.000000000000000000, 0.9238795325112869605, 1.000000000000000000, 0.9238795325112869605, 1.000000000000000000, 0.9238795325112869605, 1.000000000000000000, 0.9238795325112869605, 1.000000000000000000, 0.9238795325112869605, 1.000000000000000000, 0.9238795325112869605, 1.000000000000000000, 0.9238795325112869605, 1.000000000000000000, 0.9238795325112869605, 1.000000000000000000, 0.9238795325112869605, 1.000000000000000000, 0.9238795325112869605, 1.000000000000000000, 0.9238795325112869605, 1.000000000000000000, 0.9238795325112869605, 1.000000000000000000, 0.9238795325112869605, 1.000000000000000000, 0.9238795325112869605, 1.000000000000000000, 0.9238795325112869605, 1.000000000000000000, 0.9238795325112869605, 1.000000000000000000, 0.9238795325112869605, 1.000000000000000000, 0.9238795325112869605, 1.000000000000000000, 0.9238795325112869605, 1.000000000000000000, 0.9238795325112869605, 1.000000000000000000, 0.9238795325112869605, 1.000000000000000000, 0.9238795325112869605, 1.000000000000000000, 0.9238795325112869605, 1.000000000000000000, 0.9238795325112869605, 1.000000000000000000, 0.9238795325112869605, 1.000000000000000000, 0.9238795325112869605, 1.000000000000000000, 0.9238795325112869605, 1.000000000000000000, 0.9238795325112869605, 1.000000000000000000, 0.9238795325112869605, 1.000000000000000000, 0.9238795325112869605, 1.000000000000000000, 0.9238795325112869605, 1.000000000000000000, 0.9238795325112869605, 1.000000000000000000, 0.9238795325112869605, 1.000000000000000000, 0.9238795325112869605, 1.000000000000000000, 0.9238795325112869605, 1.000000000000000000, 0.9238795325112869605, 1.000000000000000000, 0.9238795325112869605, 1.000000000000000000, 0.9238795325112869605, 1.000000000000000000, 0.9238795325112869605, 1.000000000000000000, 0.9238795325112869605, 1.000000000000000000, 0.9238795325112869605, 1.000000000000000000, 0.9238795325112869605, 1.000000000000000000, 0.9238795325112869605, 1.000000000000000000, 0.9238795325112869605, 1.000000000000000000, 0.9238795325112869605, 1.000000000000000000, 0.9238795325112869605, 1.000000000000000000) ) ) 
 REPRESENTATION_ITEM ( '' )  SURFACE ( )  );
#459 = CARTESIAN_POINT ( 'NONE',  ( 136.3568202015646875, 0.5053874888704125157, -11.17693241582777119 ) ) ;
#460 = CARTESIAN_POINT ( 'NONE',  ( 121.9859814775786333, 0.2603800115204892296, -16.42320221600525088 ) ) ;
#461 = CARTESIAN_POINT ( 'NONE',  ( 108.8851452545248151, 0.8980012041604421569, -11.00651665394454071 ) ) ;
#462 = CARTESIAN_POINT ( 'NONE',  ( 120.2841814775786276, -10.15424416112533912, -14.75197769757731336 ) ) ;
#463 = ORIENTED_EDGE ( 'NONE', *, *, #12759, .F. ) ;
#464 = CARTESIAN_POINT ( 'NONE',  ( 114.7816948109119863, 0.5811942927096154232, -14.16772938898807155 ) ) ;
#465 = AXIS2_PLACEMENT_3D ( 'NONE', #17179, #9891, #34693 ) ;
#466 = CARTESIAN_POINT ( 'NONE',  ( 69.69189222814998175, -41.76310523276723785, -4.893215200338314474 ) ) ;
#467 = CARTESIAN_POINT ( 'NONE',  ( 120.1814158072985350, 0.3208234527006321724, -15.99825685930877839 ) ) ;
#468 = DIRECTION ( 'NONE',  ( 0.000000000000000000, -0.3818493186865927203, 0.9242245927363029745 ) ) ;
#469 = EDGE_CURVE ( 'NONE', #23752, #259, #6849, .T. ) ;
#470 = CARTESIAN_POINT ( 'NONE',  ( 125.2194014775786286, -10.30919188438810075, -12.61870101168855918 ) ) ;
#471 = CONICAL_SURFACE ( 'NONE', #35383, 5.999999999999997335, 0.4636476090008060935 ) ;
#472 = DIRECTION ( 'NONE',  ( 0.000000000000000000, 0.000000000000000000, -1.000000000000000000 ) ) ;
#473 = CARTESIAN_POINT ( 'NONE',  ( 112.1243801106810167, -8.918668529216430940, -16.32041580884654053 ) ) ;
#474 = CARTESIAN_POINT ( 'NONE',  ( 124.4819548109119722, -7.893985811506177619, -18.51759400769804742 ) ) ;
#476 = CARTESIAN_POINT ( 'NONE',  ( 123.3474214775786209, -0.1624402480850797581, -16.17319339645315424 ) ) ;
#475 = CARTESIAN_POINT ( 'NONE',  ( 122.8368814775786291, -1.561330072975668948, -17.79121239304076951 ) ) ;
#477 = CARTESIAN_POINT ( 'NONE',  ( 118.2987481442453088, -7.894159318335828068, -9.358103419637847864 ) ) ;
#478 = LINE ( 'NONE', #3232, #42202 ) ;
#479 = CARTESIAN_POINT ( 'NONE',  ( 116.5969481442453031, 0.5811942927096154232, -14.16772938898807155 ) ) ;
#480 = EDGE_LOOP ( 'NONE', ( #674, #23, #42394, #32349, #19349 ) ) ;
#481 = VECTOR ( 'NONE', #10247, 1000.000000000000000 ) ;
#482 = DIRECTION ( 'NONE',  ( -0.2768435750659241079, -0.3568721902840695792, 0.8921882507333129819 ) ) ;
#483 = CARTESIAN_POINT ( 'NONE',  ( 125.4357681442453156, -2.109465145233854422, -8.734689011828928429 ) ) ;
#484 = CARTESIAN_POINT ( 'NONE',  ( 113.2606921295247702, -9.868328341294093420, -13.39321520033831447 ) ) ;
#485 = CARTESIAN_POINT ( 'NONE',  ( 110.1353015045248469, -6.936859964151250502, -18.39754474579286025 ) ) ;
#486 = CARTESIAN_POINT ( 'NONE',  ( 115.6915515045247531, -6.936859964151250502, -18.39754474579286025 ) ) ;
#487 = DIRECTION ( 'NONE',  ( 0.9609149988134843001, -0.1028163501681632064, 0.2570431154366505933 ) ) ;
#488 = CARTESIAN_POINT ( 'NONE',  ( 112.5693548109119888, -10.63000616557722466, -14.87417383870573495 ) ) ;
#489 = ORIENTED_EDGE ( 'NONE', *, *, #38798, .T. ) ;
#490 = EDGE_CURVE ( 'NONE', #13961, #15605, #188, .T. ) ;
#491 = CARTESIAN_POINT ( 'NONE',  ( 114.8951481442453115, -8.899110576539710493, -16.42337572283490132 ) ) ;
#492 = CARTESIAN_POINT ( 'NONE',  ( 112.7745202545247878, -10.62599879583958717, -15.77991374673208469 ) ) ;
#493 = CARTESIAN_POINT ( 'NONE',  ( 118.7735460444391862, -1.267766418764730840, -16.93314635290706605 ) ) ;
#494 = CARTESIAN_POINT ( 'NONE',  ( 122.0427081442452817, 0.5811942927096110934, -14.16772938898807510 ) ) ;
#495 = EDGE_CURVE ( 'NONE', #29216, #38926, #30, .T. ) ;
#496 = CARTESIAN_POINT ( 'NONE',  ( 126.0135748109119902, -8.166667518702819706, -8.995218007635861213 ) ) ;
#497 = CARTESIAN_POINT ( 'NONE',  ( 64.24243542014160369, -41.01918285936451269, -16.39321520033831447 ) ) ;
#498 = CARTESIAN_POINT ( 'NONE',  ( 116.6536748109119941, 0.9020085738987339008, -11.91225656197089222 ) ) ;
#499 = CARTESIAN_POINT ( 'NONE',  ( 115.6915515045247531, -2.477300249445798297, -7.631215200338321125 ) ) ;
#500 = CARTESIAN_POINT ( 'NONE',  ( 112.9134265045247645, -2.791137627527939813, -8.388885654883777576 ) ) ;
#501 = ORIENTED_EDGE ( 'NONE', *, *, #21109, .T. ) ;
#502 = CARTESIAN_POINT ( 'NONE',  ( 127.0150841466612093, -7.206988222280049428, -8.529861501223846787 ) ) ;
#503 = CARTESIAN_POINT ( 'NONE',  ( 116.4834948109119779, -7.894159318335828068, -9.358103419637847864 ) ) ;
#504 = CARTESIAN_POINT ( 'NONE',  ( 113.0798948109119948, -0.4660016031367893996, -10.09054647747474043 ) ) ;
#505 = AXIS2_PLACEMENT_3D ( 'NONE', #40612, #43354, #19626 ) ;
#506 = CARTESIAN_POINT ( 'NONE',  ( 114.9970202545248412, -10.62599879583958717, -15.77991374673208469 ) ) ;
#507 = CARTESIAN_POINT ( 'NONE',  ( 105.2041296295248287, -4.863998795839590272, -8.388885654883775800 ) ) ;
#508 = CYLINDRICAL_SURFACE ( 'NONE', #17648, 1.999999999999998890 ) ;
#509 = CARTESIAN_POINT ( 'NONE',  ( 118.2420214775786320, -6.222761293078241884, -8.102969835052219238 ) ) ;
#510 = CARTESIAN_POINT ( 'NONE',  ( 112.9097148109120070, -9.565557343593413364, -10.61323700422348004 ) ) ;
#511 = VERTEX_POINT ( 'NONE', #38315 ) ;
#512 = AXIS2_PLACEMENT_3D ( 'NONE', #29324, #1497, #9256 ) ;
#513 = CARTESIAN_POINT ( 'NONE',  ( 125.7866681442452688, -8.899110576539710493, -16.42337572283490132 ) ) ;
#514 = CARTESIAN_POINT ( 'NONE',  ( 125.3895814775786448, -2.084020599724406786, -8.691656652584148546 ) ) ;
#515 = CARTESIAN_POINT ( 'NONE',  ( 112.4559014775786778, -0.1624402480850797581, -16.17319339645315424 ) ) ;
#516 = ORIENTED_EDGE ( 'NONE', *, *, #914, .T. ) ;
#517 = DIRECTION ( 'NONE',  ( -0.7071067811865480168, 0.5654279342906962658, 0.4246071727182139655 ) ) ;
#518 = CARTESIAN_POINT ( 'NONE',  ( 112.6828081442453282, -7.893985811506177619, -18.51759400769804742 ) ) ;
#519 = VECTOR ( 'NONE', #2199, 999.9999999999998863 ) ;
#520 = CARTESIAN_POINT ( 'NONE',  ( 111.5938171295247940, 0.1403307496149613920, -13.39321520033831447 ) ) ;
#521 = CARTESIAN_POINT ( 'NONE',  ( 124.8790414775786246, -8.899110576539710493, -16.42337572283490132 ) ) ;
#522 = EDGE_CURVE ( 'NONE', #12356, #39715, #34544, .T. ) ;
#523 = VERTEX_POINT ( 'NONE', #21002 ) ;
#524 = CARTESIAN_POINT ( 'NONE',  ( 117.9583881442453048, 0.1319031606808879209, -14.10382304977623669 ) ) ;
#525 = CARTESIAN_POINT ( 'NONE',  ( 112.2857214775786474, -5.574606645277164318, -18.38911715685844683 ) ) ;
#526 = DIRECTION ( 'NONE',  ( 1.000000000000000000, 0.000000000000000000, 0.000000000000000000 ) ) ;
#527 = EDGE_CURVE ( 'NONE', #24697, #26785, #16321, .T. ) ;
#528 = CARTESIAN_POINT ( 'NONE',  ( 123.8411891859119862, -8.844754642576884152, -8.592115655440050404 ) ) ;
#529 = VERTEX_POINT ( 'NONE', #27409 ) ;
#530 = CARTESIAN_POINT ( 'NONE',  ( 121.4178819144190129, -1.220279397241718966, -16.99638242193886484 ) ) ;
#531 = DIRECTION ( 'NONE',  ( 0.000000000000000000, 0.000000000000000000, -1.000000000000000000 ) ) ;
#532 = ADVANCED_FACE ( 'NONE', ( #3665 ), #7307, .T. ) ;
#533 = CARTESIAN_POINT ( 'NONE',  ( 112.4967077545247633, -7.250697342233347165, -7.631215200338321125 ) ) ;
#534 = CIRCLE ( 'NONE', #35440, 3.000000000000002665 ) ;
#535 = CARTESIAN_POINT ( 'NONE',  ( 112.5693548109119888, -10.63000616557722466, -14.87417383870573495 ) ) ;
#536 = CARTESIAN_POINT ( 'NONE',  ( 126.2972081442452890, -2.084020599724406786, -8.691656652584148546 ) ) ;
#537 = CARTESIAN_POINT ( 'NONE',  ( 118.8092881442453290, -0.1624402480850797581, -16.17319339645315424 ) ) ;
#538 = DIRECTION ( 'NONE',  ( 1.000000000000000000, 0.000000000000000000, -0.000000000000000000 ) ) ;
#539 = EDGE_LOOP ( 'NONE', ( #15498, #3012, #28270, #31753 ) ) ;
#540 = CARTESIAN_POINT ( 'NONE',  ( 115.5758681442453053, -7.894159318335828068, -9.358103419637847864 ) ) ;
#541 = CARTESIAN_POINT ( 'NONE',  ( 115.4137390045248566, 0.8980012041604421569, -15.77991374673208469 ) ) ;
#542 = CARTESIAN_POINT ( 'NONE',  ( 85.65290454163996969, -26.88367880166602220, -8.452090709015315895 ) ) ;
#543 = DIRECTION ( 'NONE',  ( 1.000000000000000000, 0.000000000000000000, -0.000000000000000000 ) ) ;
#544 = CARTESIAN_POINT ( 'NONE',  ( 115.1787814775786387, -9.988377603198976828, -10.36322818467138340 ) ) ;
#545 = ORIENTED_EDGE ( 'NONE', *, *, #32038, .F. ) ;
#546 = CARTESIAN_POINT ( 'NONE',  ( 118.7525614775786380, -8.166667518702819706, -8.995218007635861213 ) ) ;
#547 = CARTESIAN_POINT ( 'NONE',  ( 113.8740681442453138, 0.5811942927096102052, -14.16772938898808221 ) ) ;
#548 = CARTESIAN_POINT ( 'NONE',  ( 113.1912390045248031, 0.8980012041604421569, -15.77991374673208469 ) ) ;
#549 = CARTESIAN_POINT ( 'NONE',  ( 111.7184548109119788, -9.261995988541697145, -16.69588392320189030 ) ) ;
#550 = EDGE_CURVE ( 'NONE', #15771, #19842, #17806, .T. ) ;
#551 = CARTESIAN_POINT ( 'NONE',  ( 114.5547881442453217, -5.638512984488999180, -18.83840828888717311 ) ) ;
#552 = CIRCLE ( 'NONE', #2726, 2.000000000000001776 ) ;
#553 = DIRECTION ( 'NONE',  ( -0.6049664196031393493, 0.7962509850245451659, 0.000000000000000000 ) ) ;
#554 = CARTESIAN_POINT ( 'NONE',  ( 62.74499803203641335, -14.59121584191781018, -17.38686684484656908 ) ) ;
#555 = CARTESIAN_POINT ( 'NONE',  ( 110.3436608795247764, -1.325403438956436419, -16.93181055722141792 ) ) ;
#556 = EDGE_LOOP ( 'NONE', ( #34925, #21880, #41263, #43526, #26990, #41505, #39389, #13719, #5501, #37121, #24239, #17991 ) ) ;
#557 = CARTESIAN_POINT ( 'NONE',  ( 119.7434548109119703, -4.863998795839242995, -13.39321520033831447 ) ) ;
#558 = CARTESIAN_POINT ( 'NONE',  ( 109.2294414898113217, -8.099164058012600975, -17.65094077544404882 ) ) ;
#559 = CARTESIAN_POINT ( 'NONE',  ( 116.8805814775786445, -3.505236298600246325, -18.68346056562440793 ) ) ;
#560 = CARTESIAN_POINT ( 'NONE',  ( 64.90995917204980969, -13.28308322077656278, -11.63059948780157349 ) ) ;
#561 = CARTESIAN_POINT ( 'NONE',  ( 122.7386537256648751, -1.063912429576147511, -17.20460841810472985 ) ) ;
#562 = CARTESIAN_POINT ( 'NONE',  ( 111.2465515045248168, -2.477300249445798297, -7.631215200338321125 ) ) ;
#563 = CARTESIAN_POINT ( 'NONE',  ( 126.5010429760476995, -4.770821923364382044, -8.252762481559532404 ) ) ;
#564 = CARTESIAN_POINT ( 'NONE',  ( 111.3213681442453264, -7.643976991954077427, -18.09477374809248928 ) ) ;
#565 = CARTESIAN_POINT ( 'NONE',  ( 135.7140458755418138, 1.062807768444411494, -12.64888035845507375 ) ) ;
#566 = CARTESIAN_POINT ( 'NONE',  ( 122.8368814775786291, -1.561330072975668948, -17.79121239304076951 ) ) ;
#567 = CARTESIAN_POINT ( 'NONE',  ( 117.4478481442453131, 0.2603800115204892296, -16.42320221600525088 ) ) ;
#568 = ORIENTED_EDGE ( 'NONE', *, *, #1973, .T. ) ;
#569 = CARTESIAN_POINT ( 'NONE',  ( 113.4769814775786330, 0.4262465694468514643, -12.03445270309931736 ) ) ;
#570 = CARTESIAN_POINT ( 'NONE',  ( 125.7299414775786346, 0.9020085738987339008, -11.91225656197089222 ) ) ;
#571 = CARTESIAN_POINT ( 'NONE',  ( 119.0361948109119652, -7.893985811506177619, -18.51759400769804742 ) ) ;
#572 = AXIS2_PLACEMENT_3D ( 'NONE', #28197, #18381, #24548 ) ;
#573 = CARTESIAN_POINT ( 'NONE',  ( 115.6325948109119821, -9.565557343593413364, -10.61323700422348004 ) ) ;
#574 = VERTEX_POINT ( 'NONE', #3001 ) ;
#575 = CARTESIAN_POINT ( 'NONE',  ( 120.4543614775786295, -5.574606645277164318, -18.38911715685844683 ) ) ;
#576 = CARTESIAN_POINT ( 'NONE',  ( 118.4122014775786340, 0.5811942927096110934, -14.16772938898807510 ) ) ;
#577 = CARTESIAN_POINT ( 'NONE',  ( 137.2322813334390048, 0.1647898037908461233, -15.00067708421986978 ) ) ;
#578 = B_SPLINE_CURVE_WITH_KNOTS ( 'NONE', 3,
 ( #44025, #9134, #33735, #2506, #13013, #26912, #37389, #6161, #17545, #41510, #31003, #21410, #14569, #34840, #207 ),
 .UNSPECIFIED., .F., .F.,
 ( 4, 2, 2, 1, 1, 1, 2, 2, 4 ),
 ( 0.000000000000000000, 0.2500000000000473510, 0.3750000000000788258, 0.4375000000001000311, 0.4687500000001022515, 0.4843750000001034173, 0.4921875000000962008, 0.5000000000000890399, 1.000000000000000000 ),
 .UNSPECIFIED. ) ;
#579 = CARTESIAN_POINT ( 'NONE',  ( 108.2600671295247992, -10.62599879583958540, -13.39321520033831447 ) ) ;
#580 = CARTESIAN_POINT ( 'NONE',  ( 114.2354127111058659, -1.267766418764742165, -16.93314635290707315 ) ) ;
#581 = CARTESIAN_POINT ( 'NONE',  ( 126.5034829605236268, 0.2779052449522967372, -13.48229229357312597 ) ) ;
#582 = CARTESIAN_POINT ( 'NONE',  ( 116.4555358795247884, -8.402594152722688392, -9.854619843455216355 ) ) ;
#583 = CARTESIAN_POINT ( 'NONE',  ( 113.7038881442453402, -3.383040157471821630, -19.15922257007629170 ) ) ;
#584 = DIRECTION ( 'NONE',  ( 0.000000000000000000, 0.000000000000000000, -1.000000000000000000 ) ) ;
#585 = CARTESIAN_POINT ( 'NONE',  ( 114.1009748109119784, -5.574606645277164318, -18.38911715685844683 ) ) ;
#586 = LINE ( 'NONE', #7416, #43252 ) ;
#587 = EDGE_CURVE ( 'NONE', #3470, #34725, #44742, .T. ) ;
#588 = CARTESIAN_POINT ( 'NONE',  ( 112.4290776191212871, 0.4261359969231631739, -12.14321520033833046 ) ) ;
#589 = CARTESIAN_POINT ( 'NONE',  ( 114.8581140045248361, 0.1403307496149616695, -15.46607636864997204 ) ) ;
#590 = CARTESIAN_POINT ( 'NONE',  ( 112.9664414775786412, -9.859900752359374465, -12.68260735090039404 ) ) ;
#591 = DIRECTION ( 'NONE',  ( -0.000000000000000000, -0.9284778069183721172, -0.3713878862591650232 ) ) ;
#592 = DIRECTION ( 'NONE',  ( -1.224775218828351862E-16, 0.3818493186865896671, -0.9242245927363043068 ) ) ;
#594 = CARTESIAN_POINT ( 'NONE',  ( 117.6747548109119919, -1.834011780172310813, -8.268836392978581529 ) ) ;
#593 = CARTESIAN_POINT ( 'NONE',  ( 118.6391081442452986, -4.089484607189483256, -7.948022111789462052 ) ) ;
#595 = CARTESIAN_POINT ( 'NONE',  ( 123.7445081442452874, -7.894159318335828068, -9.358103419637847864 ) ) ;
#596 = CARTESIAN_POINT ( 'NONE',  ( 118.2420214775786320, -6.222761293078241884, -8.102969835052219238 ) ) ;
#597 = CARTESIAN_POINT ( 'NONE',  ( 112.9664414775786412, -9.859900752359374465, -12.68260735090039404 ) ) ;
#598 = ORIENTED_EDGE ( 'NONE', *, *, #44306, .T. ) ;
#599 = CARTESIAN_POINT ( 'NONE',  ( 135.8497638153338585, -7.066639826094078813, -7.851922482749025711 ) ) ;
#600 = CARTESIAN_POINT ( 'NONE',  ( 121.6456214775786293, -10.63000616557722466, -14.87417383870573495 ) ) ;
#601 = CARTESIAN_POINT ( 'NONE',  ( 113.1912390045248031, -9.868328341294098749, -11.32035403202665869 ) ) ;
#602 = CARTESIAN_POINT ( 'NONE',  ( 118.0718414775786442, -0.8288870151387760510, -10.36305467784173118 ) ) ;
#603 = CARTESIAN_POINT ( 'NONE',  ( 114.1577014775786552, -3.505236298600246325, -18.68346056562440793 ) ) ;
#604 = DIRECTION ( 'NONE',  ( -1.000000000000000000, 0.000000000000000000, 0.000000000000000000 ) ) ;
#605 = CARTESIAN_POINT ( 'NONE',  ( 114.8581140045248361, -10.62599879583958717, -11.00651665394454604 ) ) ;
#606 = CARTESIAN_POINT ( 'NONE',  ( 121.0783548109119749, -9.565557343593413364, -10.61323700422348004 ) ) ;
#607 = CARTESIAN_POINT ( 'NONE',  ( 123.1205148109119563, -7.643976991954077427, -18.09477374809248928 ) ) ;
#608 = CARTESIAN_POINT ( 'NONE',  ( 114.6115148109119843, -6.222761293078232114, -8.102969835052212133 ) ) ;
#609 = CARTESIAN_POINT ( 'NONE',  ( 109.2293317483792805, -6.895714903177337263, -8.103635009265300226 ) ) ;
#610 = CARTESIAN_POINT ( 'NONE',  ( 121.9659548109119811, -7.554583864224885481, -18.48844787311982785 ) ) ;
#611 = CARTESIAN_POINT ( 'NONE',  ( 114.7192077545248594, -7.250697342233347165, -7.631215200338321125 ) ) ;
#612 = CARTESIAN_POINT ( 'NONE',  ( 116.4741944465760213, 2.215541826465470709, -20.45829475731958169 ) ) ;
#613 = CARTESIAN_POINT ( 'NONE',  ( 118.0718414775786300, -9.261995988541697145, -16.69588392320189030 ) ) ;
#614 = CARTESIAN_POINT ( 'NONE',  ( 116.5402214775786405, 0.2603800115204892296, -16.42320221600525088 ) ) ;
#615 = CARTESIAN_POINT ( 'NONE',  ( 111.5243640045248412, -10.62599879583958717, -11.00651665394454604 ) ) ;
#616 = EDGE_CURVE ( 'NONE', #38570, #22820, #35985, .T. ) ;
#617 = CARTESIAN_POINT ( 'NONE',  ( 114.7816948109119863, 0.5811942927096154232, -14.16772938898807155 ) ) ;
#618 = ORIENTED_EDGE ( 'NONE', *, *, #13638, .T. ) ;
#619 = DIRECTION ( 'NONE',  ( 1.000000000000000000, 0.000000000000000000, -0.000000000000000000 ) ) ;
#620 = CARTESIAN_POINT ( 'NONE',  ( 124.0848681442452772, -4.089484607189486809, -7.948022111789456723 ) ) ;
#621 = CARTESIAN_POINT ( 'NONE',  ( 117.0507614775786465, -10.30919188438810075, -12.61870101168855918 ) ) ;
#622 = CARTESIAN_POINT ( 'NONE',  ( 122.8936081442453059, -9.565557343593413364, -10.61323700422348004 ) ) ;
#623 = CARTESIAN_POINT ( 'NONE',  ( 112.0020881442453344, -9.565557343593413364, -10.61323700422348004 ) ) ;
#624 = CARTESIAN_POINT ( 'NONE',  ( 121.5888948109119809, -10.30919188438810075, -12.61870101168855918 ) ) ;
#625 = CARTESIAN_POINT ( 'NONE',  ( 113.1217858795247935, -0.7896495226426338832, -17.46756447353520159 ) ) ;
#626 = CARTESIAN_POINT ( 'NONE',  ( 116.3700414775786527, -4.153390946401321671, -8.397313243818183892 ) ) ;
#627 = CARTESIAN_POINT ( 'NONE',  ( 123.6792205938796485, -6.000230167480150811, -18.26468474152937205 ) ) ;
#628 = ORIENTED_EDGE ( 'NONE', *, *, #2447, .F. ) ;
#629 = CARTESIAN_POINT ( 'NONE',  ( 120.5678148109119832, -8.166667518702819706, -8.995218007635861213 ) ) ;
#630 = CARTESIAN_POINT ( 'NONE',  ( 123.4939235609119663, 0.6414057260225851653, -11.69287257290600657 ) ) ;
#631 = CARTESIAN_POINT ( 'NONE',  ( 121.0216281442452981, -1.561330072975668948, -17.79121239304076951 ) ) ;
#632 = ORIENTED_EDGE ( 'NONE', *, *, #36066, .T. ) ;
#633 = CARTESIAN_POINT ( 'NONE',  ( 116.1777233795247781, -8.938348069036489818, -17.46756447353520159 ) ) ;
#634 = CARTESIAN_POINT ( 'NONE',  ( 125.7299414775786346, 0.9020085738987339008, -11.91225656197089222 ) ) ;
#635 = CARTESIAN_POINT ( 'NONE',  ( 122.2128881442452979, -1.834011780172266848, -8.268836392978604621 ) ) ;
#636 = CARTESIAN_POINT ( 'NONE',  ( 114.6115148109119986, -6.222761293078241884, -8.102969835052219238 ) ) ;
#637 = CARTESIAN_POINT ( 'NONE',  ( 77.25325688895158294, -4.012910213732562070, -16.89321520033831447 ) ) ;
#638 = CARTESIAN_POINT ( 'NONE',  ( 120.1707281442453166, -9.565557343593413364, -10.61323700422348004 ) ) ;
#639 = CARTESIAN_POINT ( 'NONE',  ( 143.3676850761856940, -63.77884951796256274, -31.62409037935697143 ) ) ;
#640 = CARTESIAN_POINT ( 'NONE',  ( 119.7736414775786358, 0.1319031606808879209, -14.10382304977623669 ) ) ;
#641 = CARTESIAN_POINT ( 'NONE',  ( 125.2183010572641422, -10.90914942692569589, -9.272323934217878261 ) ) ;
#642 = CARTESIAN_POINT ( 'NONE',  ( 117.9016614775786280, -0.1624402480850797581, -16.17319339645315424 ) ) ;
#643 = CARTESIAN_POINT ( 'NONE',  ( 112.6260814775786514, -9.261995988541697145, -16.69588392320189030 ) ) ;
#644 = CARTESIAN_POINT ( 'NONE',  ( 118.4689281442453392, 0.9020085738987339008, -11.91225656197089222 ) ) ;
#645 = CARTESIAN_POINT ( 'NONE',  ( 111.8319081442453182, -5.638512984488999180, -18.83840828888717311 ) ) ;
#646 = CARTESIAN_POINT ( 'NONE',  ( 111.6379010812576809, -0.01829820670803256055, -12.14321520033831625 ) ) ;
#647 = CARTESIAN_POINT ( 'NONE',  ( 120.4543614775786295, -5.574606645277164318, -18.38911715685844683 ) ) ;
#648 = ORIENTED_EDGE ( 'NONE', *, *, #42605, .T. ) ;
#649 = CARTESIAN_POINT ( 'NONE',  ( 117.6180281442453150, -0.4660016031367893996, -10.09054647747474043 ) ) ;
#650 = CARTESIAN_POINT ( 'NONE',  ( 111.8716296295247901, -4.863998795839590272, -8.388885654883775800 ) ) ;
#651 = CARTESIAN_POINT ( 'NONE',  ( 115.8595014775786609, -7.643976991954099631, -18.09477374809247152 ) ) ;
#652 = DIRECTION ( 'NONE',  ( 0.000000000000000000, 0.9284778069183720062, 0.3713878862591650232 ) ) ;
#653 = ADVANCED_FACE ( 'NONE', ( #22123 ), #35789, .F. ) ;
#654 = CARTESIAN_POINT ( 'NONE',  ( 82.42994493343583429, -31.76310523276723430, -22.89321520033831803 ) ) ;
#655 = CARTESIAN_POINT ( 'NONE',  ( 121.0783548109119749, 0.2603800115204892296, -16.42320221600525088 ) ) ;
#656 = ORIENTED_EDGE ( 'NONE', *, *, #15376, .T. ) ;
#657 = CARTESIAN_POINT ( 'NONE',  ( 118.7315769107182177, -2.467220198592778413, -17.83387418641524391 ) ) ;
#658 = VECTOR ( 'NONE', #32222, 1000.000000000000000 ) ;
#659 = CARTESIAN_POINT ( 'NONE',  ( 122.8368814775786291, -7.894159318335828068, -9.358103419637847864 ) ) ;
#660 = CARTESIAN_POINT ( 'NONE',  ( 120.6463454359119822, -11.07370829466463569, -12.81314460846529002 ) ) ;
#661 = CARTESIAN_POINT ( 'NONE',  ( 64.65529483955577916, -15.48286765530762388, -15.65793769818279735 ) ) ;
#662 = CARTESIAN_POINT ( 'NONE',  ( 112.7050671295247923, 0.1403307496149613920, -13.39321520033831447 ) ) ;
#663 = ORIENTED_EDGE ( 'NONE', *, *, #32365, .T. ) ;
#664 = CARTESIAN_POINT ( 'NONE',  ( 114.6682414775786469, -1.561330072975668060, -17.79121239304076596 ) ) ;
#665 = CARTESIAN_POINT ( 'NONE',  ( 125.1626748109119802, -0.1624402480850797581, -16.17319339645315424 ) ) ;
#666 = DIRECTION ( 'NONE',  ( 0.000000000000000000, 0.000000000000000000, 1.000000000000000000 ) ) ;
#667 = CARTESIAN_POINT ( 'NONE',  ( 119.5467348109119712, -5.574606645277164318, -18.38911715685844683 ) ) ;
#668 = CARTESIAN_POINT ( 'NONE',  ( 112.2857214775786474, -5.574606645277164318, -18.38911715685844683 ) ) ;
#669 = CARTESIAN_POINT ( 'NONE',  ( 121.1918081442452859, 0.9020085738987339008, -11.91225656197089222 ) ) ;
#670 = CARTESIAN_POINT ( 'NONE',  ( 112.0693548109120030, -10.10582367741923093, -14.73954123521778925 ) ) ;
#671 = CARTESIAN_POINT ( 'NONE',  ( 27.57768543387103222, -14.97172645945875935, -19.39321520033831447 ) ) ;
#672 = DIRECTION ( 'NONE',  ( -0.5735764363510450492, -0.3127926500124816878, 0.7570804645221038687 ) ) ;
#673 = CARTESIAN_POINT ( 'NONE',  ( 125.5597614775786326, -7.894159318335828068, -9.358103419637847864 ) ) ;
#674 = ORIENTED_EDGE ( 'NONE', *, *, #40341, .T. ) ;
#675 = CARTESIAN_POINT ( 'NONE',  ( 114.9970202545248412, 0.1403307496149616695, -11.32035403202665336 ) ) ;
#676 = CARTESIAN_POINT ( 'NONE',  ( 121.9292548109119849, -1.561330072975668948, -17.79121239304076951 ) ) ;
#677 = CARTESIAN_POINT ( 'NONE',  ( 61.14757329627086335, -2.318400467695852285, -17.89321520033712432 ) ) ;
#678 = ORIENTED_EDGE ( 'NONE', *, *, #1567, .T. ) ;
#679 = CARTESIAN_POINT ( 'NONE',  ( 136.9394333025986157, 0.1406925880472598978, -11.10009844214757813 ) ) ;
#680 = CARTESIAN_POINT ( 'NONE',  ( 121.3619881442452879, -4.089484607189486809, -7.948022111789456723 ) ) ;
#681 = DIRECTION ( 'NONE',  ( 1.000000000000000000, 0.000000000000000000, 0.000000000000000000 ) ) ;
#682 = CARTESIAN_POINT ( 'NONE',  ( 123.1772414775786189, -5.574606645277164318, -18.38911715685844683 ) ) ;
#683 = ORIENTED_EDGE ( 'NONE', *, *, #19629, .T. ) ;
#684 = CARTESIAN_POINT ( 'NONE',  ( 114.2144281442453178, -8.166667518702817929, -8.995218007635859436 ) ) ;
#685 = DIRECTION ( 'NONE',  ( -1.000000000000000000, 0.000000000000000000, -0.000000000000000000 ) ) ;
#686 = AXIS2_PLACEMENT_3D ( 'NONE', #16548, #16776, #44363 ) ;
#687 = CARTESIAN_POINT ( 'NONE',  ( 120.2841814775786276, 0.9020085738987414503, -11.91225656197092242 ) ) ;
#688 = DIRECTION ( 'NONE',  ( -1.000000000000000000, 0.000000000000000000, -0.000000000000000000 ) ) ;
#689 = CARTESIAN_POINT ( 'NONE',  ( 126.0135748109119902, -8.166667518702819706, -8.995218007635861213 ) ) ;
#690 = CARTESIAN_POINT ( 'NONE',  ( 122.5664060953690466, -6.001247023715324147, -18.26661038929047010 ) ) ;
#691 = DIRECTION ( 'NONE',  ( 1.000000000000000000, 0.000000000000000000, -0.000000000000000000 ) ) ;
#692 = CARTESIAN_POINT ( 'NONE',  ( 123.6877814775786533, -3.383040157471821630, -19.15922257007629170 ) ) ;
#694 = CARTESIAN_POINT ( 'NONE',  ( 122.0427081442452817, -9.859900752359378018, -12.68260735090039759 ) ) ;
#693 = CARTESIAN_POINT ( 'NONE',  ( 123.1205148109119563, -1.834011780172310813, -8.268836392978581529 ) ) ;
#695 = CARTESIAN_POINT ( 'NONE',  ( 119.4900081442453086, -7.643976991954077427, -18.09477374809248928 ) ) ;
#696 = DIRECTION ( 'NONE',  ( 0.000000000000000000, -0.4669533266896290225, -0.8842819633428516957 ) ) ;
#697 = CARTESIAN_POINT ( 'NONE',  ( 120.3409081442453044, -0.4660016031367893996, -10.09054647747474043 ) ) ;
#698 = ORIENTED_EDGE ( 'NONE', *, *, #12294, .T. ) ;
#699 = ORIENTED_EDGE ( 'NONE', *, *, #22024, .F. ) ;
#700 = CARTESIAN_POINT ( 'NONE',  ( 112.0109337908067886, 0.5115630086001619059, -12.14321520033831625 ) ) ;
#701 = CARTESIAN_POINT ( 'NONE',  ( 115.9693640045247776, -10.62599879583958717, -11.00651665394454604 ) ) ;
#702 = CARTESIAN_POINT ( 'NONE',  ( 114.3719421295247827, -9.868328341294093420, -13.39321520033831447 ) ) ;
#703 = CARTESIAN_POINT ( 'NONE',  ( 110.4131140045248287, 0.1403307496149616695, -15.46607636864997204 ) ) ;
#704 = CARTESIAN_POINT ( 'NONE',  ( 113.6079577545248043, -2.791137627527939813, -18.39754474579286025 ) ) ;
#705 = CARTESIAN_POINT ( 'NONE',  ( 124.9357681442453014, -1.834011780172310813, -8.268836392978581529 ) ) ;
#706 = CARTESIAN_POINT ( 'NONE',  ( 125.7866681442452688, -8.899110576539710493, -16.42337572283490132 ) ) ;
#707 = EDGE_LOOP ( 'NONE', ( #22175, #39798, #28141, #15557 ) ) ;
#708 = CARTESIAN_POINT ( 'NONE',  ( 111.7184548109119788, -0.8288870151387760510, -10.36305467784173118 ) ) ;
#709 = CARTESIAN_POINT ( 'NONE',  ( 109.2324108795247923, -8.938348069036489818, -9.318865927141430916 ) ) ;
#710 = FACE_OUTER_BOUND ( 'NONE', #10794, .T. ) ;
#711 = CARTESIAN_POINT ( 'NONE',  ( 125.3895814775786448, -7.893985811506177619, -18.51759400769804742 ) ) ;
#712 = CARTESIAN_POINT ( 'NONE',  ( 63.70438564670760684, -13.53232477329181727, -18.38352350030624294 ) ) ;
#713 = CARTESIAN_POINT ( 'NONE',  ( 116.8238548109119819, -4.089484607189486809, -7.948022111789456723 ) ) ;
#714 = CARTESIAN_POINT ( 'NONE',  ( 115.3442858795247759, -0.7896495226426338832, -17.46756447353520159 ) ) ;
#715 = CARTESIAN_POINT ( 'NONE',  ( 110.0658483795247804, -8.402594152722688392, -16.93181055722141792 ) ) ;
#716 = ORIENTED_EDGE ( 'NONE', *, *, #37812, .T. ) ;
#717 = CARTESIAN_POINT ( 'NONE',  ( 89.12784890491134604, -25.99489077589524300, -13.39321520033831625 ) ) ;
#718 = CARTESIAN_POINT ( 'NONE',  ( 115.6325948109119821, -9.565557343593413364, -10.61323700422348004 ) ) ;
#719 = CARTESIAN_POINT ( 'NONE',  ( 112.7962614775786676, -3.383040157471821630, -19.15922257007629170 ) ) ;
#720 = AXIS2_PLACEMENT_3D ( 'NONE', #5243, #1374, #19159 ) ;
#721 = CARTESIAN_POINT ( 'NONE',  ( 83.84865386347668448, -25.99489077589588604, -15.39321520033831625 ) ) ;
#722 = CARTESIAN_POINT ( 'NONE',  ( 118.0718414775786442, -0.8288870151387542906, -10.36305467784175782 ) ) ;
#723 = CARTESIAN_POINT ( 'NONE',  ( 121.2485348109119769, -8.899110576539710493, -16.42337572283490132 ) ) ;
#724 = CARTESIAN_POINT ( 'NONE',  ( 115.9162281442453093, -5.574606645277164318, -18.38911715685844683 ) ) ;
#725 = ORIENTED_EDGE ( 'NONE', *, *, #4716, .T. ) ;
#726 = CARTESIAN_POINT ( 'NONE',  ( 122.3826735609119680, -9.645473719204776586, -14.86997237629376656 ) ) ;
#727 = AXIS2_PLACEMENT_3D ( 'NONE', #17094, #41489, #30986 ) ;
#728 = CARTESIAN_POINT ( 'NONE',  ( 121.6115542554890823, -2.372251574601201174, -17.96033910819751611 ) ) ;
#729 = CARTESIAN_POINT ( 'NONE',  ( 112.2857214775786474, -5.574606645277164318, -18.38911715685844683 ) ) ;
#730 = ORIENTED_EDGE ( 'NONE', *, *, #26390, .T. ) ;
#731 = AXIS2_PLACEMENT_3D ( 'NONE', #25829, #15568, #36529 ) ;
#732 = DIRECTION ( 'NONE',  ( 1.000000000000000000, 0.000000000000000000, -0.000000000000000000 ) ) ;
#733 = CARTESIAN_POINT ( 'NONE',  ( 110.2047546295247855, -4.863998795839590272, -18.39754474579285315 ) ) ;
#734 = CARTESIAN_POINT ( 'NONE',  ( 113.0231681442453180, -10.15424416112533912, -14.75197769757731336 ) ) ;
#735 = VERTEX_POINT ( 'NONE', #8443 ) ;
#736 = EDGE_LOOP ( 'NONE', ( #25087, #5555, #41613, #11878, #12693, #17378, #19659, #35868, #19138, #20829, #22693, #7077, #26268, #39578, #22712, #14892, #27175, #41481, #36545, #23506, #11620, #21726, #7317, #13984, #8190, #40680, #34034, #25489, #21906, #8484, #12745, #23708, #757, #38515, #7628, #13878, #11265, #4610, #632, #28496, #3732, #17194, #21188, #31683, #31251 ) ) ;
#737 = CARTESIAN_POINT ( 'NONE',  ( 118.4689281442453392, -10.15424416112533912, -14.75197769757731336 ) ) ;
#738 = CARTESIAN_POINT ( 'NONE',  ( 118.4689281442453250, -10.15424416112533912, -14.75197769757731336 ) ) ;
#739 = CARTESIAN_POINT ( 'NONE',  ( 124.5602934112120721, -9.863183861322463386, -13.54995704067371598 ) ) ;
#740 = ADVANCED_FACE ( 'NONE', ( #42651 ), #25772, .F. ) ;
#741 = CARTESIAN_POINT ( 'NONE',  ( 121.4797829359119987, -4.283928203966213211, -7.183505701512925334 ) ) ;
#742 = ORIENTED_EDGE ( 'NONE', *, *, #32280, .T. ) ;
#743 = CYLINDRICAL_SURFACE ( 'NONE', #3356, 5.999999999999997335 ) ;
#744 = CARTESIAN_POINT ( 'NONE',  ( 125.1433143116118032, -2.283722140743223328, -6.422401579036027819 ) ) ;
#745 = CARTESIAN_POINT ( 'NONE',  ( 112.4272546295247821, -4.863998795839590272, -7.631215200338315796 ) ) ;
#746 = CARTESIAN_POINT ( 'NONE',  ( 112.1722681442453222, -0.4660016031367893996, -10.09054647747474043 ) ) ;
#747 = CARTESIAN_POINT ( 'NONE',  ( 113.1933481442453058, -4.089484607189486809, -7.948022111789456723 ) ) ;
#748 = CARTESIAN_POINT ( 'NONE',  ( 117.4478481442453131, -9.565557343593413364, -10.61323700422348004 ) ) ;
#749 = CARTESIAN_POINT ( 'NONE',  ( 138.2184548109119930, -4.863998795840020151, -13.39321520033889890 ) ) ;
#750 = EDGE_LOOP ( 'NONE', ( #41830, #3198, #2175, #16810 ) ) ;
#751 = CARTESIAN_POINT ( 'NONE',  ( 117.9016614775786280, -0.1624402480850797581, -16.17319339645315424 ) ) ;
#752 = CARTESIAN_POINT ( 'NONE',  ( 119.7434548109119419, -2.229855236528029305, -9.108032788432828042 ) ) ;
#753 = CIRCLE ( 'NONE', #18249, 1.610000000000000986 ) ;
#754 = CARTESIAN_POINT ( 'NONE',  ( 125.1533364939176636, -1.283731733903592076, -16.91188614879543906 ) ) ;
#755 = CARTESIAN_POINT ( 'NONE',  ( 116.5249890045247980, 0.8980012041604421569, -15.77991374673208469 ) ) ;
#756 = CARTESIAN_POINT ( 'NONE',  ( 115.5758681442453053, -1.561330072975668060, -17.79121239304076951 ) ) ;
#757 = ORIENTED_EDGE ( 'NONE', *, *, #19062, .F. ) ;
#758 = TOROIDAL_SURFACE ( 'NONE', #8032, 1.500000000000000000, 0.5000000000000000000 ) ;
#759 = CARTESIAN_POINT ( 'NONE',  ( 118.8660148109119774, -10.30919188438810075, -12.61870101168855918 ) ) ;
#760 = DIRECTION ( 'NONE',  ( 1.000000000000000000, 0.000000000000000000, 0.000000000000000000 ) ) ;
#761 = CARTESIAN_POINT ( 'NONE',  ( 111.7327233795247849, -8.938348069036489818, -17.46756447353520159 ) ) ;
#762 = CARTESIAN_POINT ( 'NONE',  ( 116.0864081442453113, -9.988377603198976828, -10.36322818467138340 ) ) ;
#763 = CARTESIAN_POINT ( 'NONE',  ( 113.4202548109119846, -10.30919188438810075, -12.61870101168855918 ) ) ;
#764 = CARTESIAN_POINT ( 'NONE',  ( 35.90261398037149121, 14.17005867477686820, -19.39321520033831447 ) ) ;
#765 = CARTESIAN_POINT ( 'NONE',  ( 71.37572422742091760, -11.86958442233774313, -21.39321520033831447 ) ) ;
#766 = CARTESIAN_POINT ( 'NONE',  ( 106.3848327545248651, -6.936859964151250502, -8.388885654883777576 ) ) ;
#767 = EDGE_CURVE ( 'NONE', #10224, #32004, #15058, .T. ) ;
#768 = EDGE_LOOP ( 'NONE', ( #33338, #27679, #441, #42888 ) ) ;
#769 = LINE ( 'NONE', #29271, #10675 ) ;
#770 = CARTESIAN_POINT ( 'NONE',  ( 109.2294595382483777, -2.917851662749194386, -18.10281666216439689 ) ) ;
#771 = CARTESIAN_POINT ( 'NONE',  ( 115.1787814775786387, -0.1624402480850797581, -16.17319339645315424 ) ) ;
#772 = CARTESIAN_POINT ( 'NONE',  ( 64.39654352178588681, -13.03842319615433709, -11.15581236813648935 ) ) ;
#773 = CARTESIAN_POINT ( 'NONE',  ( 118.1852948109119836, -5.638512984489023161, -18.83840828888716601 ) ) ;
#774 = CARTESIAN_POINT ( 'NONE',  ( 114.1635827545248389, -6.936859964151250502, -8.388885654883777576 ) ) ;
#775 = CARTESIAN_POINT ( 'NONE',  ( 126.5254139958991431, -4.795709975826312643, -8.240175154163296156 ) ) ;
#776 = CARTESIAN_POINT ( 'NONE',  ( 114.4413348109119823, -0.8288870151387760510, -10.36305467784173118 ) ) ;
#777 = CARTESIAN_POINT ( 'NONE',  ( 135.8582226017265384, 1.040662781756023447, -12.66189764563367604 ) ) ;
#778 = EDGE_CURVE ( 'NONE', #21905, #21031, #9632, .T. ) ;
#779 = CARTESIAN_POINT ( 'NONE',  ( 122.3830681442452857, -8.166667518702819706, -8.995218007635861213 ) ) ;
#780 = CARTESIAN_POINT ( 'NONE',  ( 119.3765548109119834, 0.9020085738987339008, -11.91225656197089222 ) ) ;
#781 = EDGE_LOOP ( 'NONE', ( #39157, #35315, #35728, #29011 ) ) ;
#782 = EDGE_CURVE ( 'NONE', #20212, #40139, #9055, .T. ) ;
#783 = CARTESIAN_POINT ( 'NONE',  ( 116.6536748109119941, -10.15424416112533912, -14.75197769757731336 ) ) ;
#784 = CARTESIAN_POINT ( 'NONE',  ( 112.6828081442453282, -7.893985811506177619, -18.51759400769804742 ) ) ;
#785 = CIRCLE ( 'NONE', #6628, 1.009117809157100254 ) ;
#786 = CARTESIAN_POINT ( 'NONE',  ( 117.0507614775786465, -10.30919188438810075, -12.61870101168855918 ) ) ;
#787 = CARTESIAN_POINT ( 'NONE',  ( 119.4900081442453086, -7.643976991954077427, -18.09477374809248928 ) ) ;
#788 = EDGE_LOOP ( 'NONE', ( #32650, #7157 ) ) ;
#789 = CARTESIAN_POINT ( 'NONE',  ( 121.3052614775786111, -7.643976991954077427, -18.09477374809248928 ) ) ;
#790 = EDGE_CURVE ( 'NONE', #42505, #31077, #32347, .T. ) ;
#791 = CONICAL_SURFACE ( 'NONE', #29218, 1.610000000000000986, 0.9599310885968765916 ) ;
#792 = CARTESIAN_POINT ( 'NONE',  ( 119.8303681442453126, -10.63000616557722466, -14.87417383870573495 ) ) ;
#793 = DIRECTION ( 'NONE',  ( -0.7871354856660162103, -0.4483307682966942709, -0.4235767337848251879 ) ) ;
#794 = CARTESIAN_POINT ( 'NONE',  ( 111.3854577545248645, -7.250697342233347165, -7.631215200338321125 ) ) ;
#795 = CIRCLE ( 'NONE', #27739, 2.000000000000000444 ) ;
#796 = EDGE_CURVE ( 'NONE', #20803, #26292, #18485, .T. ) ;
#797 = EDGE_CURVE ( 'NONE', #37424, #32220, #29734, .T. ) ;
#798 = EDGE_CURVE ( 'NONE', #38024, #6756, #5259, .T. ) ;
#799 = CARTESIAN_POINT ( 'NONE',  ( 64.46696884418977902, -15.35047623416358142, -10.89321734395795893 ) ) ;
#800 = DIRECTION ( 'NONE',  ( 0.9609149988134837450, -0.1028163501681639419, 0.2570431154366518145 ) ) ;
#801 = CARTESIAN_POINT ( 'NONE',  ( 113.3301452545248083, -9.868328341294098749, -15.46607636864997204 ) ) ;
#802 = CARTESIAN_POINT ( 'NONE',  ( 113.9875214775786532, -0.4660016031367893996, -10.09054647747474043 ) ) ;
#803 = CARTESIAN_POINT ( 'NONE',  ( 121.9470836909669913, -27.84333996136784961, -14.15691383771150136 ) ) ;
#804 = CARTESIAN_POINT ( 'NONE',  ( 116.8238548109119819, -5.574606645277164318, -18.38911715685844683 ) ) ;
#805 = CARTESIAN_POINT ( 'NONE',  ( 111.4567791257774729, 0.2334052082820642360, -12.14321520033830026 ) ) ;
#806 = DIRECTION ( 'NONE',  ( 1.000000000000000000, 0.000000000000000000, 0.000000000000000000 ) ) ;
#807 = CARTESIAN_POINT ( 'NONE',  ( 112.7050671295247923, 0.1403307496149613920, -13.39321520033831447 ) ) ;
#808 = CARTESIAN_POINT ( 'NONE',  ( 112.2289948109119848, -7.643976991954077427, -18.09477374809248928 ) ) ;
#809 = DIRECTION ( 'NONE',  ( -0.1352586133457901185, -0.9908103287288512195, 0.000000000000000000 ) ) ;
#810 = AXIS2_PLACEMENT_3D ( 'NONE', #14418, #28328, #11900 ) ;
#811 = DIRECTION ( 'NONE',  ( 0.000000000000000000, 0.000000000000000000, 1.000000000000000000 ) ) ;
#813 = CARTESIAN_POINT ( 'NONE',  ( 117.6180281442453150, -0.4660016031367893996, -10.09054647747474043 ) ) ;
#812 = CARTESIAN_POINT ( 'NONE',  ( 60.96717296766336602, -14.49347760901631688, -8.701126109306295930 ) ) ;
#814 = CARTESIAN_POINT ( 'NONE',  ( 117.9583881442453048, 0.1319031606808879209, -14.10382304977623669 ) ) ;
#815 = CARTESIAN_POINT ( 'NONE',  ( 125.5030348109119558, -3.383040157471821630, -19.15922257007629170 ) ) ;
#816 = VERTEX_POINT ( 'NONE', #43550 ) ;
#817 = CARTESIAN_POINT ( 'NONE',  ( 136.9115742440160659, -9.061375133822513916, -9.797515867730091088 ) ) ;
#818 = CARTESIAN_POINT ( 'NONE',  ( 123.8012348109119642, 0.2603800115204892296, -16.42320221600525088 ) ) ;
#819 = CARTESIAN_POINT ( 'NONE',  ( 114.0246765045248196, -2.791137627527939813, -8.388885654883777576 ) ) ;
#820 = CARTESIAN_POINT ( 'NONE',  ( 119.7736414775786358, 0.1319031606808879209, -14.10382304977623669 ) ) ;
#821 = CARTESIAN_POINT ( 'NONE',  ( 115.7460481442453357, -10.15424416112533912, -14.75197769757731336 ) ) ;
#822 = CARTESIAN_POINT ( 'NONE',  ( 85.43848064358274996, -28.59459646149706913, -9.352541679919285755 ) ) ;
#823 = CARTESIAN_POINT ( 'NONE',  ( 113.3301452545248083, 0.8980012041604421569, -11.00651665394454071 ) ) ;
#824 = CARTESIAN_POINT ( 'NONE',  ( 119.3765548109119834, -10.15424416112533912, -14.75197769757731336 ) ) ;
#825 = CONICAL_SURFACE ( 'NONE', #24153, 2.999999999999999556, 0.9599310885968830309 ) ;
#826 = CARTESIAN_POINT ( 'NONE',  ( 124.8790414775786246, -8.899110576539710493, -16.42337572283490132 ) ) ;
#827 = CARTESIAN_POINT ( 'NONE',  ( 114.8384214775786489, -10.15424416112534267, -14.75197769757730804 ) ) ;
#828 = CARTESIAN_POINT ( 'NONE',  ( 109.2293785907020407, -6.437107504569898886, -7.971344053030498422 ) ) ;
#829 = CARTESIAN_POINT ( 'NONE',  ( 123.5633766859119760, -0.06289925094097943703, -9.412459353600674206 ) ) ;
#830 = CARTESIAN_POINT ( 'NONE',  ( 106.8710046295248759, -4.863998795839590272, -18.39754474579285315 ) ) ;
#831 = PRODUCT_DEFINITION_SHAPE ( 'NONE', 'NONE',  #16477 ) ;
#832 = CARTESIAN_POINT ( 'NONE',  ( 62.57015527438819191, -24.33598972801448923, -6.893215200338315363 ) ) ;
#833 = CARTESIAN_POINT ( 'NONE',  ( 118.8660148109119774, -10.30919188438810075, -12.61870101168855918 ) ) ;
#834 = CARTESIAN_POINT ( 'NONE',  ( 118.2420214775786320, -3.383040157471821630, -19.15922257007629170 ) ) ;
#835 = CARTESIAN_POINT ( 'NONE',  ( 110.1353015045248469, -2.477300249445798297, -7.631215200338321125 ) ) ;
#836 = CARTESIAN_POINT ( 'NONE',  ( 112.5693548109119888, -10.63000616557722466, -14.87417383870573495 ) ) ;
#837 = ORIENTED_EDGE ( 'NONE', *, *, #6922, .T. ) ;
#838 = CARTESIAN_POINT ( 'NONE',  ( 70.19189222814998175, -62.26243369865490251, -38.10776559704283528 ) ) ;
#839 = CARTESIAN_POINT ( 'NONE',  ( 115.5758681442453053, -1.561330072975668060, -17.79121239304076951 ) ) ;
#840 = CARTESIAN_POINT ( 'NONE',  ( 120.3409081442453044, -8.899110576539710493, -16.42337572283490132 ) ) ;
#841 = APPLICATION_PROTOCOL_DEFINITION ( 'draft international standard', 'automotive_design', 1998, #25639 ) ;
#842 = CARTESIAN_POINT ( 'NONE',  ( 124.7088614775786226, 0.2603800115204892296, -16.42320221600525088 ) ) ;
#843 = CARTESIAN_POINT ( 'NONE',  ( 121.1918081442452859, 0.9020085738987339008, -11.91225656197089222 ) ) ;
#844 = EDGE_CURVE ( 'NONE', #21157, #21529, #40068, .T. ) ;
#845 = CARTESIAN_POINT ( 'NONE',  ( 114.1635827545248389, -2.477300249445798297, -19.15521520033831138 ) ) ;
#846 = CARTESIAN_POINT ( 'NONE',  ( 117.6180281442453150, -8.899110576539710493, -16.42337572283490132 ) ) ;
#847 = CARTESIAN_POINT ( 'NONE',  ( 122.1743141859119817, -0.8832429491016019485, -18.19431474523657855 ) ) ;
#848 = LINE ( 'NONE', #18639, #17728 ) ;
#849 = ORIENTED_EDGE ( 'NONE', *, *, #34615, .T. ) ;
#850 = SHAPE_REPRESENTATION ( 'Reach Screw', ( #12375 ), #43820 ) ;
#851 = EDGE_CURVE ( 'NONE', #28482, #19616, #5453, .T. ) ;
#852 = CARTESIAN_POINT ( 'NONE',  ( 123.6328298109119714, -2.173413727453600508, -8.297982527556802879 ) ) ;
#853 = CARTESIAN_POINT ( 'NONE',  ( 120.3976348109119812, -1.834011780172310813, -8.268836392978581529 ) ) ;
#854 = VERTEX_POINT ( 'NONE', #33717 ) ;
#855 = DIRECTION ( 'NONE',  ( 0.000000000000000000, 0.000000000000000000, -1.000000000000000000 ) ) ;
#856 = CARTESIAN_POINT ( 'NONE',  ( 128.0511146350389993, -7.187744967641459759, -18.83419938739690025 ) ) ;
#857 = EDGE_CURVE ( 'NONE', #16139, #18111, #18527, .T. ) ;
#858 = DIRECTION ( 'NONE',  ( 0.000000000000000000, -0.9242245927363029745, -0.3818493186865927203 ) ) ;
#859 = CARTESIAN_POINT ( 'NONE',  ( 117.1642148109119859, -0.8288870151387760510, -10.36305467784173118 ) ) ;
#860 = DIRECTION ( 'NONE',  ( -0.000000000000000000, -0.9284778069183718952, -0.3713878862591649677 ) ) ;
#861 = EDGE_CURVE ( 'NONE', #37401, #29422, #44018, .T. ) ;
#862 = CARTESIAN_POINT ( 'NONE',  ( 64.12124478315966769, -35.39759648474613840, -5.871463680831255694 ) ) ;
#863 = CARTESIAN_POINT ( 'NONE',  ( 119.6601881442453106, -1.833838273342659253, -17.42832698103878286 ) ) ;
#864 = CARTESIAN_POINT ( 'NONE',  ( 121.5888948109119809, -10.30919188438809364, -12.61870101168852187 ) ) ;
#865 = CARTESIAN_POINT ( 'NONE',  ( 123.0070614775786169, -10.15424416112533912, -14.75197769757731336 ) ) ;
#866 = CARTESIAN_POINT ( 'NONE',  ( 124.1726284085844298, -11.17717881402670699, -8.479713305622000874 ) ) ;
#867 = CARTESIAN_POINT ( 'NONE',  ( 118.7525614775786380, -1.833838273342659253, -17.42832698103878286 ) ) ;
#868 = CARTESIAN_POINT ( 'NONE',  ( 114.8384214775786489, 0.9020085738987339008, -11.91225656197089222 ) ) ;
#869 = CARTESIAN_POINT ( 'NONE',  ( 120.6812681442452941, -10.30919188438810075, -12.61870101168855918 ) ) ;
#870 = CARTESIAN_POINT ( 'NONE',  ( 112.1722681442453222, -0.4660016031367893996, -10.09054647747474043 ) ) ;
#871 = FACE_OUTER_BOUND ( 'NONE', #3620, .T. ) ;
#872 = CARTESIAN_POINT ( 'NONE',  ( 120.2274548109119934, -9.859900752359374465, -12.68260735090039404 ) ) ;
#873 = VERTEX_POINT ( 'NONE', #7043 ) ;
#874 = CARTESIAN_POINT ( 'NONE',  ( 122.0427081442452817, 0.5811942927096110934, -14.16772938898807510 ) ) ;
#875 = CARTESIAN_POINT ( 'NONE',  ( 111.4549108795247747, -1.325403438956436419, -16.93181055722141792 ) ) ;
#876 = LINE ( 'NONE', #14795, #14624 ) ;
#877 = CARTESIAN_POINT ( 'NONE',  ( 70.19189222814998175, -59.83749578782295941, -37.13779888561150244 ) ) ;
#878 = CIRCLE ( 'NONE', #26376, 20.00000000000000355 ) ;
#879 = CARTESIAN_POINT ( 'NONE',  ( 85.07488655036617331, -28.45866502056250980, -7.893215200338303816 ) ) ;
#880 = CARTESIAN_POINT ( 'NONE',  ( 59.41476255453773803, -13.68180535374018092, -7.393215200338314474 ) ) ;
#881 = ORIENTED_EDGE ( 'NONE', *, *, #16520, .F. ) ;
#882 = LINE ( 'NONE', #14801, #2318 ) ;
#883 = CARTESIAN_POINT ( 'NONE',  ( 123.2906948109119867, -1.833838273342659697, -17.42832698103878286 ) ) ;
#884 = CARTESIAN_POINT ( 'NONE',  ( 119.8129079359119942, -5.444069387712269226, -19.60292469916370450 ) ) ;
#885 = PLANE ( 'NONE',  #8115 ) ;
#886 = CARTESIAN_POINT ( 'NONE',  ( 109.2294421295247844, -49.76310523276723785, -7.393215200338315363 ) ) ;
#887 = CARTESIAN_POINT ( 'NONE',  ( 112.6356140045247827, 0.1403307496149616695, -15.46607636864997204 ) ) ;
#888 = ORIENTED_EDGE ( 'NONE', *, *, #41925, .F. ) ;
#889 = CARTESIAN_POINT ( 'NONE',  ( 113.6471614775786492, -5.638512984488999180, -18.83840828888717311 ) ) ;
#890 = AXIS2_PLACEMENT_3D ( 'NONE', #38470, #13662, #21159 ) ;
#891 = CARTESIAN_POINT ( 'NONE',  ( 114.6682414775786469, -1.561330072975668060, -17.79121239304076596 ) ) ;
#892 = DIRECTION ( 'NONE',  ( 0.9659258262890689783, 0.2588190451025185190, 0.000000000000000000 ) ) ;
#893 = CARTESIAN_POINT ( 'NONE',  ( 122.3263414775786373, -3.505236298600246325, -18.68346056562440793 ) ) ;
#894 = CARTESIAN_POINT ( 'NONE',  ( 126.2471382750707818, -3.957262863412609022, -8.461457090771025591 ) ) ;
#895 = FILL_AREA_STYLE ('',( #36665 ) ) ;
#896 = CARTESIAN_POINT ( 'NONE',  ( 122.8368814775786291, -1.561330072975668948, -17.79121239304076951 ) ) ;
#897 = LINE ( 'NONE', #21877, #4551 ) ;
#898 = DIRECTION ( 'NONE',  ( 0.000000000000000000, 0.000000000000000000, 1.000000000000000000 ) ) ;
#899 = CARTESIAN_POINT ( 'NONE',  ( 72.75524511225664526, -29.99489077589588959, -18.39321520033831803 ) ) ;
#900 = CARTESIAN_POINT ( 'NONE',  ( 112.2289948109119848, -1.834011780172310813, -8.268836392978581529 ) ) ;
#901 = EDGE_LOOP ( 'NONE', ( #39869, #4969 ) ) ;
#902 = EDGE_CURVE ( 'NONE', #31222, #12871, #2499, .T. ) ;
#903 = CARTESIAN_POINT ( 'NONE',  ( 116.3166296295247832, -4.863998795839590272, -8.388885654883775800 ) ) ;
#904 = CARTESIAN_POINT ( 'NONE',  ( 118.8092881442453290, -9.988377603198976828, -10.36322818467138340 ) ) ;
#905 = CARTESIAN_POINT ( 'NONE',  ( 61.98291279206183191, -3.705398587646214992, -19.39321520033831447 ) ) ;
#906 = EDGE_LOOP ( 'NONE', ( #19691, #14880 ) ) ;
#907 = LINE ( 'NONE', #38753, #23410 ) ;
#908 = CARTESIAN_POINT ( 'NONE',  ( 111.3780948109119890, -5.574606645277164318, -18.38911715685844683 ) ) ;
#909 = AXIS2_PLACEMENT_3D ( 'NONE', #40106, #12526, #26200 ) ;
#910 = DIRECTION ( 'NONE',  ( -0.000000000000000000, -0.9284778069183721172, -0.3713878862591650232 ) ) ;
#911 = CARTESIAN_POINT ( 'NONE',  ( 121.9859814775786333, -9.565557343593413364, -10.61323700422348004 ) ) ;
#912 = ORIENTED_EDGE ( 'NONE', *, *, #22583, .T. ) ;
#913 = CARTESIAN_POINT ( 'NONE',  ( 116.6536748109119941, 0.9020085738987339008, -11.91225656197089222 ) ) ;
#914 = EDGE_CURVE ( 'NONE', #29459, #28588, #42750, .T. ) ;
#915 = DIRECTION ( 'NONE',  ( 0.9908103287288504424, -0.1352586133457951423, 0.000000000000000000 ) ) ;
#916 = CARTESIAN_POINT ( 'NONE',  ( 112.7156220163423512, -1.087735405160637603, -17.17288456429614030 ) ) ;
#917 = PRODUCT_DEFINITION_FORMATION_WITH_SPECIFIED_SOURCE ( 'ANY', '', #14299, .NOT_KNOWN. ) ;
#918 = CARTESIAN_POINT ( 'NONE',  ( 91.65862616933031859, -25.99489077589524300, -13.39321520033831447 ) ) ;
#919 = CARTESIAN_POINT ( 'NONE',  ( 111.3780948109119890, -5.574606645277164318, -18.38911715685844683 ) ) ;
#920 = DIRECTION ( 'NONE',  ( 0.000000000000000000, -0.6004852223388327248, 0.7996358532186277346 ) ) ;
#921 = PLANE ( 'NONE',  #20121 ) ;
#922 = CARTESIAN_POINT ( 'NONE',  ( 125.2761281442453054, -10.63000616557722466, -14.87417383870573495 ) ) ;
#924 = CARTESIAN_POINT ( 'NONE',  ( 122.2696148109119889, -5.574606645277164318, -18.38911715685844683 ) ) ;
#923 = CARTESIAN_POINT ( 'NONE',  ( 124.0848681442452772, -4.089484607189486809, -7.948022111789456723 ) ) ;
#925 = CARTESIAN_POINT ( 'NONE',  ( 116.7068493634037480, -7.245760568235874999, -17.91803073691438897 ) ) ;
#926 = CARTESIAN_POINT ( 'NONE',  ( 122.0427081442452817, -9.859900752359378018, -12.68260735090039759 ) ) ;
#927 = CARTESIAN_POINT ( 'NONE',  ( 113.6471614775786492, -4.153390946401321671, -8.397313243818183892 ) ) ;
#928 = CARTESIAN_POINT ( 'NONE',  ( 120.6812681442452941, -10.30919188438810075, -12.61870101168855918 ) ) ;
#929 = ORIENTED_EDGE ( 'NONE', *, *, #41606, .T. ) ;
#930 = VERTEX_POINT ( 'NONE', #30764 ) ;
#931 = CARTESIAN_POINT ( 'NONE',  ( 111.8277378519202756, 0.2518737723193609224, -12.14321520033831625 ) ) ;
#932 = CARTESIAN_POINT ( 'NONE',  ( -1.145390592550938447, -14.88589425535891841, -7.393215200338315363 ) ) ;
#933 = CARTESIAN_POINT ( 'NONE',  ( 112.9134265045247645, -2.791137627527939813, -8.388885654883777576 ) ) ;
#934 = CARTESIAN_POINT ( 'NONE',  ( 114.0246765045248196, -2.791137627527939813, -8.388885654883777576 ) ) ;
#935 = EDGE_CURVE ( 'NONE', #32198, #39653, #29454, .T. ) ;
#936 = CARTESIAN_POINT ( 'NONE',  ( 126.0135748109119902, -8.166667518702819706, -8.995218007635861213 ) ) ;
#937 = CARTESIAN_POINT ( 'NONE',  ( 114.3278814775786429, -10.30919188438810075, -12.61870101168855918 ) ) ;
#938 = EDGE_LOOP ( 'NONE', ( #22426, #35188, #1636, #40965 ) ) ;
#939 = CARTESIAN_POINT ( 'NONE',  ( 111.5482748109120053, -0.1624402480850797581, -16.17319339645315424 ) ) ;
#940 = CARTESIAN_POINT ( 'NONE',  ( 107.7044421295247929, 0.8980012041604618078, -13.39321520033831447 ) ) ;
#941 = CARTESIAN_POINT ( 'NONE',  ( 122.0427081442452817, -9.859900752359374465, -12.68260735090038693 ) ) ;
#942 = CARTESIAN_POINT ( 'NONE',  ( 69.69189222814998175, -41.76310523276723785, -4.893215200338314474 ) ) ;
#943 = CARTESIAN_POINT ( 'NONE',  ( 109.2294421295247560, 0.08637466845215115152, -14.75790253999268131 ) ) ;
#944 = CARTESIAN_POINT ( 'NONE',  ( 66.31928500851137187, -14.71576354012722021, -16.39321520033831447 ) ) ;
#945 = CARTESIAN_POINT ( 'NONE',  ( 115.8027748109119841, -0.4660016031367893996, -10.09054647747474043 ) ) ;
#946 = CIRCLE ( 'NONE', #26438, 8.000000000000001776 ) ;
#947 = CARTESIAN_POINT ( 'NONE',  ( 116.4555358795247884, -0.7896495226426338832, -17.46756447353520159 ) ) ;
#948 = CARTESIAN_POINT ( 'NONE',  ( 113.8163171295247764, 0.1403307496149613920, -13.39321520033831447 ) ) ;
#949 = ORIENTED_EDGE ( 'NONE', *, *, #17087, .T. ) ;
#950 = CARTESIAN_POINT ( 'NONE',  ( 126.2184548109105435, -7.866424907533402511, -9.395035934245175469 ) ) ;
#951 = CARTESIAN_POINT ( 'NONE',  ( 117.5045748109119756, -9.859900752359374465, -12.68260735090039404 ) ) ;
#952 = AXIS2_PLACEMENT_3D ( 'NONE', #12557, #23033, #37617 ) ;
#953 = CARTESIAN_POINT ( 'NONE',  ( 116.7104014775786425, -0.4660016031367893996, -10.09054647747474043 ) ) ;
#954 = CARTESIAN_POINT ( 'NONE',  ( 113.5904348109119866, -7.893985811506177619, -18.51759400769804742 ) ) ;
#955 = CARTESIAN_POINT ( 'NONE',  ( 125.1059481442452750, -1.833838273342660141, -17.42832698103878286 ) ) ;
#956 = UNCERTAINTY_MEASURE_WITH_UNIT (LENGTH_MEASURE( 1.000000000000000082E-05 ), #5660, 'distance_accuracy_value', 'NONE');
#957 = CARTESIAN_POINT ( 'NONE',  ( 120.6245414775786458, -0.1624402480850797581, -16.17319339645315424 ) ) ;
#958 = CARTESIAN_POINT ( 'NONE',  ( 117.4478481442453131, -9.565557343593413364, -10.61323700422348004 ) ) ;
#959 = EDGE_LOOP ( 'NONE', ( #4440, #25894, #33864, #38580, #39938 ) ) ;
#960 = CARTESIAN_POINT ( 'NONE',  ( 120.0212673109119805, 0.2312338769422704887, -16.08380026872395874 ) ) ;
#961 = CIRCLE ( 'NONE', #4601, 8.000000000000001776 ) ;
#962 = CARTESIAN_POINT ( 'NONE',  ( 111.7184548109119788, -9.142054238649166109, -15.98131134002176523 ) ) ;
#963 = CARTESIAN_POINT ( 'NONE',  ( 116.8805814775786445, -3.505236298600246325, -18.68346056562440793 ) ) ;
#964 = ORIENTED_EDGE ( 'NONE', *, *, #27844, .T. ) ;
#965 = DIRECTION ( 'NONE',  ( 1.000000000000000000, 0.000000000000000000, 0.000000000000000000 ) ) ;
#966 = CARTESIAN_POINT ( 'NONE',  ( 115.5191414775786569, -3.383040157471821630, -19.15922257007629170 ) ) ;
#967 = CARTESIAN_POINT ( 'NONE',  ( 115.2748327545248657, -2.477300249445798297, -19.15521520033831138 ) ) ;
#968 = CARTESIAN_POINT ( 'NONE',  ( 114.2144281442453178, -1.833838273342658809, -17.42832698103878286 ) ) ;
#969 = ORIENTED_EDGE ( 'NONE', *, *, #34509, .F. ) ;
#970 = VERTEX_POINT ( 'NONE', #23714 ) ;
#971 = CARTESIAN_POINT ( 'NONE',  ( 123.9146881442452894, -10.15424416112533912, -14.75197769757731336 ) ) ;
#972 = EDGE_CURVE ( 'NONE', #3055, #38119, #11731, .T. ) ;
#973 = CARTESIAN_POINT ( 'NONE',  ( 116.3700414775786527, -4.153390946401321671, -8.397313243818183892 ) ) ;
#974 = CARTESIAN_POINT ( 'NONE',  ( 110.2184548109119788, -3.104384172016180887, -16.98539509221845734 ) ) ;
#975 = CARTESIAN_POINT ( 'NONE',  ( 121.6881423109119709, -9.959231468620755479, -10.70263013195267199 ) ) ;
#976 = ORIENTED_EDGE ( 'NONE', *, *, #851, .T. ) ;
#977 = VECTOR ( 'NONE', #13213, 1000.000000000000114 ) ;
#978 = DIRECTION ( 'NONE',  ( -0.5735764363510450492, -0.3127926500124816878, 0.7570804645221038687 ) ) ;
#979 = CARTESIAN_POINT ( 'NONE',  ( 124.6565730087411765, -2.409824777551811792, -5.955873678245978908 ) ) ;
#980 = CARTESIAN_POINT ( 'NONE',  ( 111.9410827545248708, -2.477300249445798297, -19.15521520033831138 ) ) ;
#981 = CIRCLE ( 'NONE', #8996, 1.500000000000001332 ) ;
#982 = CARTESIAN_POINT ( 'NONE',  ( 111.8319081442453182, -5.638512984488999180, -18.83840828888717311 ) ) ;
#983 = CARTESIAN_POINT ( 'NONE',  ( 112.8529881442453302, -1.561330072975668060, -17.79121239304076596 ) ) ;
#984 = CARTESIAN_POINT ( 'NONE',  ( 122.6667014775786413, -2.084020599724406786, -8.691656652584148546 ) ) ;
#985 = FACE_OUTER_BOUND ( 'NONE', #8311, .T. ) ;
#986 = ORIENTED_EDGE ( 'NONE', *, *, #21820, .F. ) ;
#987 = CARTESIAN_POINT ( 'NONE',  ( 119.6601881442453106, -1.833838273342659253, -17.42832698103878286 ) ) ;
#988 = CARTESIAN_POINT ( 'NONE',  ( 115.9693640045247776, -10.62599879583958717, -11.00651665394454604 ) ) ;
#989 = AXIS2_PLACEMENT_3D ( 'NONE', #41662, #38211, #6989 ) ;
#990 = CARTESIAN_POINT ( 'NONE',  ( 117.1500671295247713, 0.1403307496149613920, -13.39321520033831447 ) ) ;
#991 = FACE_OUTER_BOUND ( 'NONE', #6590, .T. ) ;
#992 = CARTESIAN_POINT ( 'NONE',  ( 113.8740681442453138, 0.5811942927096154232, -14.16772938898807155 ) ) ;
#993 = ORIENTED_EDGE ( 'NONE', *, *, #15751, .F. ) ;
#994 = CARTESIAN_POINT ( 'NONE',  ( 118.1852948109119836, -5.638512984488999180, -18.83840828888717311 ) ) ;
#995 = CARTESIAN_POINT ( 'NONE',  ( 114.0442481442453300, -1.834011780172303929, -8.268836392978592187 ) ) ;
#996 = CARTESIAN_POINT ( 'NONE',  ( 113.5385046295247804, -4.863998795839590272, -7.631215200338315796 ) ) ;
#997 = CARTESIAN_POINT ( 'NONE',  ( 115.8027748109119841, -0.4660016031367893996, -10.09054647747474043 ) ) ;
#998 = CARTESIAN_POINT ( 'NONE',  ( 117.4478481442453131, 0.2603800115204892296, -16.42320221600525088 ) ) ;
#999 = CARTESIAN_POINT ( 'NONE',  ( 127.4620922276734092, -10.46289306240577588, -13.90154686030524189 ) ) ;
#1000 = DIRECTION ( 'NONE',  ( 1.000000000000000000, 0.000000000000000000, -0.000000000000000000 ) ) ;
#1001 = CARTESIAN_POINT ( 'NONE',  ( 90.93679655599923706, -18.80572346544368756, -4.893215200338314474 ) ) ;
#1002 = ORIENTED_EDGE ( 'NONE', *, *, #1925, .F. ) ;
#1003 = LINE ( 'NONE', #43187, #23766 ) ;
#1004 = CARTESIAN_POINT ( 'NONE',  ( 109.2294436890326779, -7.171314547180734245, -18.16325295140885387 ) ) ;
#1005 = CARTESIAN_POINT ( 'NONE',  ( 118.9794681442453026, -0.8288870151387760510, -10.36305467784173118 ) ) ;
#1006 = CARTESIAN_POINT ( 'NONE',  ( -1.637506834317598026, -6.775152287193681566, -8.893215200338314474 ) ) ;
#1007 = CARTESIAN_POINT ( 'NONE',  ( 115.6915515045247531, -6.936859964151250502, -18.39754474579286025 ) ) ;
#1008 = CARTESIAN_POINT ( 'NONE',  ( 113.8857702545248003, 0.1403307496149616695, -11.32035403202665336 ) ) ;
#1009 = CARTESIAN_POINT ( 'NONE',  ( 126.3975136127440919, -4.653777249196778598, -8.307659966040843003 ) ) ;
#1010 = CARTESIAN_POINT ( 'NONE',  ( 113.9307948109119764, -10.15424416112533912, -14.75197769757731336 ) ) ;
#1011 = CARTESIAN_POINT ( 'NONE',  ( 125.4584548109119737, -4.863998795839242995, -13.39321520033831447 ) ) ;
#1012 = CARTESIAN_POINT ( 'NONE',  ( 122.5532481442453019, -10.63000616557722466, -14.87417383870573495 ) ) ;
#1013 = CARTESIAN_POINT ( 'NONE',  ( 120.0572748109119772, -3.383040157471821630, -19.15922257007629170 ) ) ;
#1014 = ORIENTED_EDGE ( 'NONE', *, *, #2177, .F. ) ;
#1015 = CARTESIAN_POINT ( 'NONE',  ( 119.8303681442453126, 0.4262465694468514643, -12.03445270309931736 ) ) ;
#1016 = CARTESIAN_POINT ( 'NONE',  ( 125.9568481442452850, -6.344957434206665248, -7.627207830600338134 ) ) ;
#1017 = CARTESIAN_POINT ( 'NONE',  ( 116.8805814775786445, -6.344957434206662583, -7.627207830600332805 ) ) ;
#1018 = CARTESIAN_POINT ( 'NONE',  ( 120.3976348109119812, -7.643976991954077427, -18.09477374809248928 ) ) ;
#1019 = ORIENTED_EDGE ( 'NONE', *, *, #38423, .F. ) ;
#1020 = CARTESIAN_POINT ( 'NONE',  ( 125.2194014775786286, 0.1319031606808879209, -14.10382304977623669 ) ) ;
#1021 = CARTESIAN_POINT ( 'NONE',  ( 121.9859814775786333, 0.2603800115204892296, -16.42320221600525088 ) ) ;
#1022 = CARTESIAN_POINT ( 'NONE',  ( 95.28169473643895060, -27.46631665213706341, -9.831789489566176599 ) ) ;
#1023 = CARTESIAN_POINT ( 'NONE',  ( 110.6909265045248247, -7.250697342233347165, -19.15521520033831138 ) ) ;
#1024 = DIRECTION ( 'NONE',  ( -1.000000000000000000, 0.000000000000000000, 0.000000000000000000 ) ) ;
#1025 = CARTESIAN_POINT ( 'NONE',  ( 116.6447457829843870, 0.6362173239733635022, -14.64321520033831447 ) ) ;
#1026 = EDGE_CURVE ( 'NONE', #25605, #31523, #7613, .T. ) ;
#1027 = CARTESIAN_POINT ( 'NONE',  ( 113.5385046295247804, -4.863998795839590272, -18.39754474579285315 ) ) ;
#1028 = CARTESIAN_POINT ( 'NONE',  ( 116.8805814775786445, -6.344957434206662583, -7.627207830600332805 ) ) ;
#1029 = CARTESIAN_POINT ( 'NONE',  ( 137.4945747549981547, -9.790276493893014020, -12.42916563457901269 ) ) ;
#1030 = CARTESIAN_POINT ( 'NONE',  ( 117.3343948109119737, -6.222761293078241884, -8.102969835052219238 ) ) ;
#1031 = CARTESIAN_POINT ( 'NONE',  ( 126.2333338125975217, -0.7732851963037252752, -10.50508471548512190 ) ) ;
#1032 = CARTESIAN_POINT ( 'NONE',  ( 117.3911214775786505, -7.894159318335806752, -9.358103419637833653 ) ) ;
#1033 = CARTESIAN_POINT ( 'NONE',  ( 108.8156921295247912, -9.868328341294093420, -13.39321520033831447 ) ) ;
#1034 = CARTESIAN_POINT ( 'NONE',  ( 113.2500748109119968, -3.505236298600246325, -18.68346056562440793 ) ) ;
#1035 = EDGE_CURVE ( 'NONE', #40192, #37616, #36694, .T. ) ;
#1036 = CARTESIAN_POINT ( 'NONE',  ( 111.6276609221557550, -2.372251574601221158, -17.96033910819751966 ) ) ;
#1038 = CARTESIAN_POINT ( 'NONE',  ( 119.4900081442453086, -1.834011780172310813, -8.268836392978581529 ) ) ;
#1037 = CARTESIAN_POINT ( 'NONE',  ( 64.06711464991177252, -13.62989902061672431, -8.594543081115894267 ) ) ;
#1039 = B_SPLINE_CURVE_WITH_KNOTS ( 'NONE', 3,
 ( #24514, #35194, #31789, #561, #42073, #10831, #7621, #32236, #7172, #14471 ),
 .UNSPECIFIED., .F., .F.,
 ( 4, 3, 3, 4 ),
 ( 0.000000000000000000, 0.0001671877560958060112, 0.0003343755126086500086, 0.0006438490228505489759 ),
 .UNSPECIFIED. ) ;
#1040 = CARTESIAN_POINT ( 'NONE',  ( 119.2063748109119814, -7.894159318335828068, -9.358103419637847864 ) ) ;
#1041 = CARTESIAN_POINT ( 'NONE',  ( 112.7395348109119766, -4.153390946401321671, -8.397313243818183892 ) ) ;
#1042 = VERTEX_POINT ( 'NONE', #3175 ) ;
#1043 = DIRECTION ( 'NONE',  ( 0.000000000000000000, 0.000000000000000000, -1.000000000000000000 ) ) ;
#1044 = CARTESIAN_POINT ( 'NONE',  ( 121.5321681442453183, -9.988377603198976828, -10.36322818467138340 ) ) ;
#1045 = CARTESIAN_POINT ( 'NONE',  ( 116.5249890045247980, -9.868328341294098749, -11.32035403202665869 ) ) ;
#1046 = CARTESIAN_POINT ( 'NONE',  ( 118.2420214775786320, -6.222761293078241884, -8.102969835052219238 ) ) ;
#1047 = EDGE_CURVE ( 'NONE', #6949, #28070, #36732, .T. ) ;
#1048 = CARTESIAN_POINT ( 'NONE',  ( 116.3133148109120043, -2.084020599724406786, -8.691656652584148546 ) ) ;
#1049 = CARTESIAN_POINT ( 'NONE',  ( 85.01908738548678457, -29.61018707541026629, -10.68033442898624941 ) ) ;
#1050 = CARTESIAN_POINT ( 'NONE',  ( 107.9128015045248219, -2.477300249445798297, -7.631215200338321125 ) ) ;
#1051 = CARTESIAN_POINT ( 'NONE',  ( 123.2339681442453241, -3.505236298600246325, -18.68346056562440793 ) ) ;
#1052 = CARTESIAN_POINT ( 'NONE',  ( 122.3263414775786373, -3.505236298600246325, -18.68346056562440793 ) ) ;
#1053 = CARTESIAN_POINT ( 'NONE',  ( 114.7816948109119863, -9.859900752359374465, -12.68260735090037983 ) ) ;
#1054 = CARTESIAN_POINT ( 'NONE',  ( 109.2294962932281095, -5.361490969279928187, -7.816834419629333119 ) ) ;
#1055 = CARTESIAN_POINT ( 'NONE',  ( 123.2161110609119561, -3.163656168406935087, -18.89861972220014508 ) ) ;
#1056 = CARTESIAN_POINT ( 'NONE',  ( 106.1070202545248407, 0.1403307496149616695, -11.32035403202665336 ) ) ;
#1057 = ADVANCED_FACE ( 'NONE', ( #37605 ), #20955, .T. ) ;
#1058 = CARTESIAN_POINT ( 'NONE',  ( 116.8894182543351405, 1.911972990205162981, -21.02721497854282973 ) ) ;
#1059 = CARTESIAN_POINT ( 'NONE',  ( 83.41361896732357195, -32.98529496753769052, -22.17982263453885494 ) ) ;
#1060 = CARTESIAN_POINT ( 'NONE',  ( 116.1998614775786507, -10.63000616557722466, -14.87417383870573495 ) ) ;
#1061 = CARTESIAN_POINT ( 'NONE',  ( 117.7314814775786260, -4.089484607189486809, -7.948022111789456723 ) ) ;
#1062 = CARTESIAN_POINT ( 'NONE',  ( 110.9687390045248350, 0.8980012041604421569, -15.77991374673208469 ) ) ;
#1063 = CARTESIAN_POINT ( 'NONE',  ( 112.7962614775786676, -3.383040157471821630, -19.15922257007629170 ) ) ;
#1064 = ADVANCED_FACE ( 'NONE', ( #14107 ), #43297, .T. ) ;
#1065 = ADVANCED_FACE ( 'NONE', ( #27355 ), #14883, .T. ) ;
#1066 = ORIENTED_EDGE ( 'NONE', *, *, #25382, .T. ) ;
#1067 = CARTESIAN_POINT ( 'NONE',  ( 65.10287265247757205, -0.4742552606671820992, -16.39321520033831447 ) ) ;
#1068 = AXIS2_PLACEMENT_3D ( 'NONE', #35389, #28345, #42258 ) ;
#1069 = CARTESIAN_POINT ( 'NONE',  ( 115.5191414775786569, -3.383040157471821630, -19.15922257007629170 ) ) ;
#1070 = CARTESIAN_POINT ( 'NONE',  ( 123.5743281442453139, -2.084020599724406786, -8.691656652584148546 ) ) ;
#1071 = APPLICATION_PROTOCOL_DEFINITION ( 'draft international standard', 'automotive_design', 1998, #9054 ) ;
#1072 = CARTESIAN_POINT ( 'NONE',  ( 124.6521348109119884, -1.561330072975668948, -17.79121239304076951 ) ) ;
#1073 = CARTESIAN_POINT ( 'NONE',  ( 121.2485348109119769, -0.4660016031367893996, -10.09054647747474043 ) ) ;
#1074 = AXIS2_PLACEMENT_3D ( 'NONE', #18198, #11365, #39169 ) ;
#1075 = CARTESIAN_POINT ( 'NONE',  ( 113.6079577545248043, -7.250697342233347165, -7.631215200338321125 ) ) ;
#1076 = CARTESIAN_POINT ( 'NONE',  ( 118.0718414775786442, -0.8288870151387760510, -10.36305467784173118 ) ) ;
#1077 = CARTESIAN_POINT ( 'NONE',  ( 122.9382985609119743, -10.36940331770106916, -15.09355782777062061 ) ) ;
#1078 = CARTESIAN_POINT ( 'NONE',  ( 123.6808719482204992, -5.999156839134923480, -18.26265215102791117 ) ) ;
#1079 = ORIENTED_EDGE ( 'NONE', *, *, #19134, .F. ) ;
#1080 = CARTESIAN_POINT ( 'NONE',  ( 121.9659548109119811, -7.554583864224885481, -18.48844787311982785 ) ) ;
#1081 = CARTESIAN_POINT ( 'NONE',  ( 119.7736414775786358, -10.30919188438810075, -12.61870101168855918 ) ) ;
#1082 = ORIENTED_EDGE ( 'NONE', *, *, #17680, .F. ) ;
#1083 = CARTESIAN_POINT ( 'NONE',  ( 80.41643495664496299, -3.865424785743087899, -10.39321520033831625 ) ) ;
#1084 = CARTESIAN_POINT ( 'NONE',  ( 64.05455464101120810, -2.913905561056498339, -7.947895114335570277 ) ) ;
#1085 = CARTESIAN_POINT ( 'NONE',  ( 121.9100498793805230, -2.191907684172563986, -18.20049396185734025 ) ) ;
#1086 = CARTESIAN_POINT ( 'NONE',  ( 115.7460481442453357, -10.15424416112533912, -14.75197769757731336 ) ) ;
#1087 = CARTESIAN_POINT ( 'NONE',  ( 125.4584548109119737, -4.863998795839242995, -13.39321520033831447 ) ) ;
#1088 = CARTESIAN_POINT ( 'NONE',  ( 64.98570645825515157, -35.85007757536534001, -5.722960826911935861 ) ) ;
#1089 = CARTESIAN_POINT ( 'NONE',  ( 123.1205148109119563, -7.643976991954077427, -18.09477374809248928 ) ) ;
#1090 = LINE ( 'NONE', #639, #17142 ) ;
#1091 = CARTESIAN_POINT ( 'NONE',  ( 121.0783548109119749, -9.565557343593413364, -10.61323700422348004 ) ) ;
#1092 = AXIS2_PLACEMENT_3D ( 'NONE', #41329, #44293, #41546 ) ;
#1093 = DIRECTION ( 'NONE',  ( 0.5040994586965589219, 0.8636456077245089347, 0.000000000000000000 ) ) ;
#1094 = CARTESIAN_POINT ( 'NONE',  ( 123.5743281442453139, -2.084020599724406786, -8.691656652584148546 ) ) ;
#1095 = CARTESIAN_POINT ( 'NONE',  ( 112.7962614775786676, -3.383040157471821630, -19.15922257007629170 ) ) ;
#1096 = CARTESIAN_POINT ( 'NONE',  ( 117.6747548109119919, -1.834011780172310813, -8.268836392978581529 ) ) ;
#1097 = CARTESIAN_POINT ( 'NONE',  ( 125.5597614775786326, -7.894159318335828068, -9.358103419637847864 ) ) ;
#1098 = DIRECTION ( 'NONE',  ( -0.000000000000000000, -0.9284778069183720062, -0.3713878862591650232 ) ) ;
#1099 = VECTOR ( 'NONE', #43138, 1000.000000000000114 ) ;
#1100 = CARTESIAN_POINT ( 'NONE',  ( 121.0783548109119749, -9.565557343593413364, -10.61323700422348004 ) ) ;
#1101 = ORIENTED_EDGE ( 'NONE', *, *, #11741, .F. ) ;
#1102 = CARTESIAN_POINT ( 'NONE',  ( 120.3409081442453044, -0.4660016031367893996, -10.09054647747474043 ) ) ;
#1103 = CARTESIAN_POINT ( 'NONE',  ( 115.4137390045248566, -9.868328341294098749, -11.32035403202665869 ) ) ;
#1104 = CARTESIAN_POINT ( 'NONE',  ( 86.84453910206313765, -17.83168818462593919, -7.393215200338315363 ) ) ;
#1105 = FACE_OUTER_BOUND ( 'NONE', #32890, .T. ) ;
#1106 = CARTESIAN_POINT ( 'NONE',  ( 120.4379860609119675, -6.564341423271550902, -7.887810678476487425 ) ) ;
#1107 = CARTESIAN_POINT ( 'NONE',  ( 117.1500671295247713, 0.1403307496149613920, -13.39321520033831447 ) ) ;
#1108 = ORIENTED_EDGE ( 'NONE', *, *, #40951, .T. ) ;
#1109 = CARTESIAN_POINT ( 'NONE',  ( 121.4754414775786131, -1.833838273342659697, -17.42832698103878286 ) ) ;
#1110 = PLANE ( 'NONE',  #3169 ) ;
#1111 = CARTESIAN_POINT ( 'NONE',  ( 63.72671350766138687, -14.88170162854069645, -18.28103043643234571 ) ) ;
#1112 = EDGE_CURVE ( 'NONE', #13294, #44431, #30929, .T. ) ;
#1113 = CARTESIAN_POINT ( 'NONE',  ( 73.01241679510815175, -68.13509210538408922, -39.58160742654554554 ) ) ;
#1114 = CARTESIAN_POINT ( 'NONE',  ( 106.8710046295248759, -4.863998795839590272, -18.39754474579285315 ) ) ;
#1115 = ORIENTED_EDGE ( 'NONE', *, *, #34492, .T. ) ;
#1116 = CARTESIAN_POINT ( 'NONE',  ( 114.7816948109119863, 0.5811942927096154232, -14.16772938898807155 ) ) ;
#1117 = DIRECTION ( 'NONE',  ( -0.3445294493088594256, -0.9387755102040817867, 2.988316619407199162E-16 ) ) ;
#1118 = CARTESIAN_POINT ( 'NONE',  ( 120.8514481442452961, -2.084020599724406786, -8.691656652584148546 ) ) ;
#1119 = CARTESIAN_POINT ( 'NONE',  ( 112.5126281442453120, 0.1319031606808879209, -14.10382304977623669 ) ) ;
#1120 = CARTESIAN_POINT ( 'NONE',  ( 123.8012348109119785, -9.565557343593409811, -10.61323700422347649 ) ) ;
#1121 = EDGE_CURVE ( 'NONE', #44907, #4162, #20514, .T. ) ;
#1122 =( BOUNDED_CURVE ( )  B_SPLINE_CURVE ( 2, ( #19826, #23016, #26445, #40580, #5905, #5451, #44003, #36681, #2485 ),
 .UNSPECIFIED., .F., .T. ) 
 B_SPLINE_CURVE_WITH_KNOTS ( ( 3, 2, 2, 2, 3 ),
 ( 0.5030750193655029179, 0.6250000000000000000, 0.7500000000000000000, 0.8750000000000000000, 0.9588811029394139762 ),
 .UNSPECIFIED. ) 
 CURVE ( )  GEOMETRIC_REPRESENTATION_ITEM ( )  RATIONAL_B_SPLINE_CURVE ( ( 0.9963469806984119881, 0.9257521078043979834, 1.000000000000000000, 0.9238795325112869605, 1.000000000000000000, 0.9238795325112869605, 1.000000000000000000, 0.9489194498462629745, 0.9663939858628869395 ) ) 
 REPRESENTATION_ITEM ( '' )  );
#1123 = CARTESIAN_POINT ( 'NONE',  ( 84.10862215250544693, -25.38011337280982715, -14.88121679464376257 ) ) ;
#1124 = VERTEX_POINT ( 'NONE', #38050 ) ;
#1125 = VECTOR ( 'NONE', #32153, 1000.000000000000227 ) ;
#1126 = LINE ( 'NONE', #14821, #18340 ) ;
#1127 = B_SPLINE_CURVE_WITH_KNOTS ( 'NONE', 3,
 ( #18016, #8205, #28064, #17795, #21663, #18476, #15050, #10739, #18244, #25088 ),
 .UNSPECIFIED., .F., .F.,
 ( 4, 3, 3, 4 ),
 ( 0.000000000000000000, 0.0001671877560958114864, 0.0003343755126086585196, 0.0006438490228507209303 ),
 .UNSPECIFIED. ) ;
#1128 = CARTESIAN_POINT ( 'NONE',  ( 122.1561614775786353, -0.4660016031367893996, -10.09054647747474043 ) ) ;
#1129 = CARTESIAN_POINT ( 'NONE',  ( 137.3802547664382985, -9.320531758105950360, -15.95367587447831248 ) ) ;
#1130 = EDGE_LOOP ( 'NONE', ( #25260, #4271, #38542, #14867, #38250, #1878, #17115, #2078 ) ) ;
#1131 = CARTESIAN_POINT ( 'NONE',  ( 61.69084222814998242, 7.836001204160461420, -12.14321520033831625 ) ) ;
#1132 = CARTESIAN_POINT ( 'NONE',  ( 125.3328548109119964, -9.261995988541697145, -16.69588392320189030 ) ) ;
#1133 = AXIS2_PLACEMENT_3D ( 'NONE', #30931, #41654, #44854 ) ;
#1134 = CARTESIAN_POINT ( 'NONE',  ( 127.0400190879707480, -4.559358201214624096, -18.79541519429530538 ) ) ;
#1135 = CARTESIAN_POINT ( 'NONE',  ( 124.9924948109119924, -5.574606645277164318, -18.38911715685844683 ) ) ;
#1136 = ORIENTED_EDGE ( 'NONE', *, *, #40982, .F. ) ;
#1137 = CARTESIAN_POINT ( 'NONE',  ( 116.3700414775786527, -5.638512984488999180, -18.83840828888717311 ) ) ;
#1138 = B_SPLINE_CURVE_WITH_KNOTS ( 'NONE', 3,
 ( #17671, #28612, #42521, #11282, #39316, #7174, #21084, #21986, #4646, #31567 ),
 .UNSPECIFIED., .F., .F.,
 ( 4, 3, 3, 4 ),
 ( 0.000000000000000000, 0.0001671877560958085049, 0.0003343755126086540201, 0.0006438490228505489759 ),
 .UNSPECIFIED. ) ;
#1139 = PLANE ( 'NONE',  #37208 ) ;
#1140 = CARTESIAN_POINT ( 'NONE',  ( 79.13619734047924226, 4.894407596166499452, -20.89842468304581047 ) ) ;
#1141 = CARTESIAN_POINT ( 'NONE',  ( 135.8419766445523464, -5.597291064638494795, -7.485280051629364273 ) ) ;
#1142 = CARTESIAN_POINT ( 'NONE',  ( 125.1626748109119802, -9.988377603198980381, -10.36322818467138518 ) ) ;
#1143 = CARTESIAN_POINT ( 'NONE',  ( 53.69308256885118169, -7.449060273445263114, -7.393215200338315363 ) ) ;
#1144 = DIRECTION ( 'NONE',  ( 0.1352586133457901185, 0.9908103287288512195, 0.000000000000000000 ) ) ;
#1145 = VECTOR ( 'NONE', #26126, 999.9999999999998863 ) ;
#1146 = CARTESIAN_POINT ( 'NONE',  ( 111.9453614775786434, -7.894159318335828068, -9.358103419637847864 ) ) ;
#1147 = CARTESIAN_POINT ( 'NONE',  ( 124.6521348109119884, -7.894159318335828068, -9.358103419637847864 ) ) ;
#1148 = CARTESIAN_POINT ( 'NONE',  ( 116.6385761563547447, -9.481945103229687533, -15.42247872983044665 ) ) ;
#1149 = CARTESIAN_POINT ( 'NONE',  ( 123.8012348109119642, -9.565557343593413364, -10.61323700422348004 ) ) ;
#1150 = DIRECTION ( 'NONE',  ( 0.5040994586965589219, 0.8636456077245089347, 0.000000000000000000 ) ) ;
#1151 = CARTESIAN_POINT ( 'NONE',  ( 120.9081748109119872, -5.638512984488999180, -18.83840828888717311 ) ) ;
#1152 = EDGE_CURVE ( 'NONE', #10924, #15883, #40363, .T. ) ;
#1153 = ORIENTED_EDGE ( 'NONE', *, *, #29788, .T. ) ;
#1154 = CARTESIAN_POINT ( 'NONE',  ( 114.5066521944298756, 0.6269505268395592079, -12.14321520033831625 ) ) ;
#1155 = CARTESIAN_POINT ( 'NONE',  ( 116.1777233795247781, -8.938348069036489818, -17.46756447353520159 ) ) ;
#1156 = CIRCLE ( 'NONE', #35346, 2.999999999999999556 ) ;
#1157 = CARTESIAN_POINT ( 'NONE',  ( 115.0664733795247798, -1.325403438956436419, -9.854619843455211026 ) ) ;
#1158 = CARTESIAN_POINT ( 'NONE',  ( 114.4413952545248350, -9.868328341294098749, -15.46607636864997204 ) ) ;
#1159 = CARTESIAN_POINT ( 'NONE',  ( 126.2597653975822709, -9.794341843349942067, -12.44453272831780311 ) ) ;
#1160 = CARTESIAN_POINT ( 'NONE',  ( 114.3846081442453197, -10.63000616557722466, -14.87417383870573495 ) ) ;
#1161 = ORIENTED_EDGE ( 'NONE', *, *, #24252, .F. ) ;
#1162 = CARTESIAN_POINT ( 'NONE',  ( 112.3991748109119868, -1.833838273342658809, -17.42832698103878286 ) ) ;
#1163 = CARTESIAN_POINT ( 'NONE',  ( 107.0099108795247815, -8.938348069036489818, -9.318865927141430916 ) ) ;
#1164 = CARTESIAN_POINT ( 'NONE',  ( 85.15861813568058380, -25.99489077589524300, -13.39321520033831625 ) ) ;
#1165 = CARTESIAN_POINT ( 'NONE',  ( 112.3991748109119868, -1.833838273342658809, -17.42832698103878286 ) ) ;
#1166 =( GEOMETRIC_REPRESENTATION_CONTEXT ( 3 ) GLOBAL_UNCERTAINTY_ASSIGNED_CONTEXT ( ( #25138 ) ) GLOBAL_UNIT_ASSIGNED_CONTEXT ( ( #7965, #1788, #11846 ) ) REPRESENTATION_CONTEXT ( 'NONE', 'WORKASPACE' ) );
#1167 = CARTESIAN_POINT ( 'NONE',  ( 119.7563403099118773, -6.348382822066793274, -18.92399070498282754 ) ) ;
#1169 = CIRCLE ( 'NONE', #19398, 10.00000000000000000 ) ;
#1168 = CARTESIAN_POINT ( 'NONE',  ( 70.19189222814998175, -67.83330054016514055, -40.33609291459782753 ) ) ;
#1170 = CARTESIAN_POINT ( 'NONE',  ( 115.6325948109119821, 0.2603800115204892296, -16.42320221600525088 ) ) ;
#1171 = CARTESIAN_POINT ( 'NONE',  ( 111.3854577545248645, -7.250697342233347165, -7.631215200338321125 ) ) ;
#1172 = CARTESIAN_POINT ( 'NONE',  ( 110.2047546295247855, -4.863998795839590272, -18.39754474579285315 ) ) ;
#1173 = ORIENTED_EDGE ( 'NONE', *, *, #20334, .T. ) ;
#1174 = CARTESIAN_POINT ( 'NONE',  ( 126.9733055311805856, -7.218567762708847368, -8.558672424457089534 ) ) ;
#1175 = CARTESIAN_POINT ( 'NONE',  ( 118.9227414775786542, 0.4262465694468514643, -12.03445270309931736 ) ) ;
#1176 = CARTESIAN_POINT ( 'NONE',  ( 114.8384214775786489, 0.9020085738987339008, -11.91225656197089222 ) ) ;
#1177 = EDGE_CURVE ( 'NONE', #1359, #5980, #25246, .T. ) ;
#1178 = CIRCLE ( 'NONE', #8439, 2.000000000000000444 ) ;
#1179 = ADVANCED_FACE ( 'NONE', ( #32760 ), #18434, .T. ) ;
#1180 = CARTESIAN_POINT ( 'NONE',  ( 111.7184548109119788, -9.261995988541697145, -16.69588392320189030 ) ) ;
#1181 = CARTESIAN_POINT ( 'NONE',  ( 124.7655881442452852, -9.859900752359378018, -12.68260735090039759 ) ) ;
#1182 = CARTESIAN_POINT ( 'NONE',  ( 123.1205148109119563, -7.643976991954077427, -18.09477374809248928 ) ) ;
#1183 = CARTESIAN_POINT ( 'NONE',  ( 114.8951481442453115, -8.899110576539710493, -16.42337572283490132 ) ) ;
#1184 = ORIENTED_EDGE ( 'NONE', *, *, #30337, .F. ) ;
#1185 = B_SPLINE_CURVE_WITH_KNOTS ( 'NONE', 3,
 ( #39404, #4514, #28248, #24600 ),
 .UNSPECIFIED., .F., .F.,
 ( 4, 4 ),
 ( 0.005279168639414119624, 0.005761668442105720260 ),
 .UNSPECIFIED. ) ;
#1186 = CARTESIAN_POINT ( 'NONE',  ( 120.9241579359119925, -5.444069387712269226, -19.60292469916370450 ) ) ;
#1187 = AXIS2_PLACEMENT_3D ( 'NONE', #31508, #41577, #10337 ) ;
#1188 = DIRECTION ( 'NONE',  ( 1.000000000000000000, 0.000000000000000000, -0.000000000000000000 ) ) ;
#1189 = CARTESIAN_POINT ( 'NONE',  ( 118.1285681442453068, -2.084020599724406786, -8.691656652584148546 ) ) ;
#1190 = ORIENTED_EDGE ( 'NONE', *, *, #8994, .T. ) ;
#1191 = CARTESIAN_POINT ( 'NONE',  ( 64.46696884418977902, -15.35047623416358142, -10.89321734395795893 ) ) ;
#1192 = CARTESIAN_POINT ( 'NONE',  ( 114.9518748109119883, -1.834011780172310813, -8.268836392978581529 ) ) ;
#1193 = CARTESIAN_POINT ( 'NONE',  ( 114.7192077545248594, -7.250697342233347165, -7.631215200338321125 ) ) ;
#1194 = CARTESIAN_POINT ( 'NONE',  ( 119.1472854349294579, -1.040089454026966287, -17.23633227186632766 ) ) ;
#1195 = ORIENTED_EDGE ( 'NONE', *, *, #29638, .F. ) ;
#1196 = ORIENTED_EDGE ( 'NONE', *, *, #31166, .F. ) ;
#1197 = CARTESIAN_POINT ( 'NONE',  ( 122.7234281442452755, -4.153390946401325223, -8.397313243818185668 ) ) ;
#1198 = CARTESIAN_POINT ( 'NONE',  ( 116.7671281442453335, -7.643976991954077427, -18.09477374809248928 ) ) ;
#1199 = DIRECTION ( 'NONE',  ( 0.000000000000000000, 0.000000000000000000, 1.000000000000000000 ) ) ;
#1200 = VECTOR ( 'NONE', #23710, 1000.000000000000114 ) ;
#1201 = CARTESIAN_POINT ( 'NONE',  ( 121.9659548109119811, -7.554583864224885481, -18.48844787311982785 ) ) ;
#1202 = VERTEX_POINT ( 'NONE', #11813 ) ;
#1203 = CARTESIAN_POINT ( 'NONE',  ( 0.04488520489200759078, -6.166763362545027327, -18.19321520033831519 ) ) ;
#1204 = CARTESIAN_POINT ( 'NONE',  ( 62.03132163408040611, -65.45885774859658568, -44.53126419185489482 ) ) ;
#1205 = CARTESIAN_POINT ( 'NONE',  ( 111.3854577545248645, -7.250697342233347165, -7.631215200338321125 ) ) ;
#1206 =( BOUNDED_CURVE ( )  B_SPLINE_CURVE ( 3, ( #13133, #12913, #34310, #37964 ),
 .UNSPECIFIED., .F., .T. ) 
 B_SPLINE_CURVE_WITH_KNOTS ( ( 4, 4 ),
 ( 3.141592653589795336, 4.712388980384689674 ),
 .UNSPECIFIED. ) 
 CURVE ( )  GEOMETRIC_REPRESENTATION_ITEM ( )  RATIONAL_B_SPLINE_CURVE ( ( 1.000000000000000000, 0.8047378541243649375, 0.8047378541243649375, 1.000000000000000000 ) ) 
 REPRESENTATION_ITEM ( '' )  );
#1207 = CARTESIAN_POINT ( 'NONE',  ( 114.1577014775786552, -6.344957434206662583, -7.627207830600332805 ) ) ;
#1208 = CARTESIAN_POINT ( 'NONE',  ( 126.0703014775786102, -0.1624402480850797581, -16.17319339645315424 ) ) ;
#1209 = CARTESIAN_POINT ( 'NONE',  ( 122.1561614775786353, -8.899110576539710493, -16.42337572283490132 ) ) ;
#1210 = CARTESIAN_POINT ( 'NONE',  ( 72.54180985774836188, -52.30061520688905574, -33.39389990939168484 ) ) ;
#1211 = ORIENTED_EDGE ( 'NONE', *, *, #8860, .T. ) ;
#1212 = CARTESIAN_POINT ( 'NONE',  ( 119.2631014775786298, -9.565557343593413364, -10.61323700422348004 ) ) ;
#1213 = DIRECTION ( 'NONE',  ( -0.1352586133457950590, -0.9908103287288504424, 0.000000000000000000 ) ) ;
#1214 = CARTESIAN_POINT ( 'NONE',  ( 114.0783153663348770, -1.172797794773246416, -17.05961127468924587 ) ) ;
#1215 = CARTESIAN_POINT ( 'NONE',  ( 114.7886608795247696, -8.938348069036489818, -9.318865927141430916 ) ) ;
#1216 = AXIS2_PLACEMENT_3D ( 'NONE', #18061, #29000, #39027 ) ;
#1217 = CARTESIAN_POINT ( 'NONE',  ( 118.7525614775786380, -8.166667518702819706, -8.995218007635861213 ) ) ;
#1218 = ORIENTED_EDGE ( 'NONE', *, *, #5520, .T. ) ;
#1219 = CARTESIAN_POINT ( 'NONE',  ( 115.7460481442453357, 0.9020085738987339008, -11.91225656197089222 ) ) ;
#1220 = CARTESIAN_POINT ( 'NONE',  ( 111.2184548109119788, -4.863998795839242995, -13.39321520033831447 ) ) ;
#1221 = CARTESIAN_POINT ( 'NONE',  ( 106.3848327545248651, -2.477300249445798297, -19.15521520033831138 ) ) ;
#1222 = CARTESIAN_POINT ( 'NONE',  ( 115.8595014775786609, -1.834011780172310813, -8.268836392978581529 ) ) ;
#1223 = CARTESIAN_POINT ( 'NONE',  ( 117.6747548109119919, -1.834011780172310813, -8.268836392978581529 ) ) ;
#1224 = CARTESIAN_POINT ( 'NONE',  ( 126.3063647503472566, -9.895249910033488305, -13.03518212827709988 ) ) ;
#1225 = CARTESIAN_POINT ( 'NONE',  ( 116.6426534889645552, -11.85006152547368430, -6.385399117676209713 ) ) ;
#1226 = CARTESIAN_POINT ( 'NONE',  ( 107.4960827545248350, -6.936859964151250502, -8.388885654883777576 ) ) ;
#1227 = AXIS2_PLACEMENT_3D ( 'NONE', #27267, #34086, #17229 ) ;
#1228 = ORIENTED_EDGE ( 'NONE', *, *, #14201, .T. ) ;
#1229 = CARTESIAN_POINT ( 'NONE',  ( 115.5212212410415873, 0.7607806665037644134, -12.14321520033829493 ) ) ;
#1230 = CARTESIAN_POINT ( 'NONE',  ( 109.2294382629313958, -10.31656828667767734, -14.31165057277949870 ) ) ;
#1231 = CARTESIAN_POINT ( 'NONE',  ( 121.7590748109119687, -2.084020599724406786, -8.691656652584148546 ) ) ;
#1232 = EDGE_CURVE ( 'NONE', #1783, #34215, #3962, .T. ) ;
#1233 = CARTESIAN_POINT ( 'NONE',  ( 114.2330358795247776, -8.402594152722688392, -9.854619843455216355 ) ) ;
#1234 = CARTESIAN_POINT ( 'NONE',  ( 113.5385046295247804, -4.863998795839590272, -18.39754474579285315 ) ) ;
#1235 = CARTESIAN_POINT ( 'NONE',  ( 114.3278814775786429, 0.1319031606808879209, -14.10382304977623669 ) ) ;
#1236 = CARTESIAN_POINT ( 'NONE',  ( 114.1577014775786552, -3.505236298600246325, -18.68346056562440793 ) ) ;
#1237 = DIRECTION ( 'NONE',  ( 0.000000000000000000, 0.000000000000000000, 1.000000000000000000 ) ) ;
#1238 = CARTESIAN_POINT ( 'NONE',  ( 124.0281414775786146, -1.834011780172310813, -8.268836392978581529 ) ) ;
#1239 = CARTESIAN_POINT ( 'NONE',  ( 120.6812681442452941, -10.30919188438810075, -12.61870101168855918 ) ) ;
#1240 = ORIENTED_EDGE ( 'NONE', *, *, #25111, .F. ) ;
#1241 = AXIS2_PLACEMENT_3D ( 'NONE', #14999, #18647, #4950 ) ;
#1242 = CARTESIAN_POINT ( 'NONE',  ( 119.4900081442453086, -7.643976991954077427, -18.09477374809248928 ) ) ;
#1243 = CARTESIAN_POINT ( 'NONE',  ( 112.6260814775786514, -9.261995988541697145, -16.69588392320189030 ) ) ;
#1244 = CARTESIAN_POINT ( 'NONE',  ( 122.0427081442452817, 0.5811942927096110934, -14.16772938898807510 ) ) ;
#1245 = CARTESIAN_POINT ( 'NONE',  ( 118.6391081442452986, -5.574606645277164318, -18.38911715685844683 ) ) ;
#1246 = VERTEX_POINT ( 'NONE', #1315 ) ;
#1247 = CARTESIAN_POINT ( 'NONE',  ( 125.7299414775786346, -10.15424416112533912, -14.75197769757731336 ) ) ;
#1248 = CARTESIAN_POINT ( 'NONE',  ( 121.4187148109119789, -6.344957434206665248, -7.627207830600338134 ) ) ;
#1249 = CARTESIAN_POINT ( 'NONE',  ( 125.0849378844206257, -6.072675180497891567, -6.000667556518594736 ) ) ;
#1250 = VECTOR ( 'NONE', #33138, 1000.000000000000000 ) ;
#1251 = DIRECTION ( 'NONE',  ( 0.2588190451025126904, -0.9659258262890705327, 0.000000000000000000 ) ) ;
#1252 = CARTESIAN_POINT ( 'NONE',  ( 126.3807372594939125, 0.2118326779918614511, -13.62869614777685001 ) ) ;
#1253 = CARTESIAN_POINT ( 'NONE',  ( 114.9970202545248412, 0.1403307496149616695, -11.32035403202665336 ) ) ;
#1254 = CARTESIAN_POINT ( 'NONE',  ( 119.5467348109119712, -4.089484607189486809, -7.948022111789456723 ) ) ;
#1255 = CARTESIAN_POINT ( 'NONE',  ( 136.1332990479119189, -10.28161693900162810, -11.09901496658777376 ) ) ;
#1256 = CARTESIAN_POINT ( 'NONE',  ( 116.6536748109119941, -10.15424416112533912, -14.75197769757731336 ) ) ;
#1257 = CARTESIAN_POINT ( 'NONE',  ( 125.1059481442452750, -8.166667518702819706, -8.995218007635861213 ) ) ;
#1258 = DIRECTION ( 'NONE',  ( 0.000000000000000000, 0.000000000000000000, 1.000000000000000000 ) ) ;
#1259 = CARTESIAN_POINT ( 'NONE',  ( 117.0056648082055801, -0.1020945015694922492, -15.74893487844867401 ) ) ;
#1260 = CARTESIAN_POINT ( 'NONE',  ( 111.6632702545248605, 0.1403307496149616695, -11.32035403202665336 ) ) ;
#1261 = AXIS2_PLACEMENT_3D ( 'NONE', #32042, #144, #7420 ) ;
#1262 = CARTESIAN_POINT ( 'NONE',  ( 112.3424481442453384, -3.505236298600246325, -18.68346056562440793 ) ) ;
#1263 = DIRECTION ( 'NONE',  ( 0.000000000000000000, 0.000000000000000000, 1.000000000000000000 ) ) ;
#1264 = DIRECTION ( 'NONE',  ( -0.7871354856660162103, -0.4483307682966942709, -0.4235767337848251879 ) ) ;
#1266 = CARTESIAN_POINT ( 'NONE',  ( 120.7947214775786193, -9.261995988541697145, -16.69588392320189030 ) ) ;
#1265 = CARTESIAN_POINT ( 'NONE',  ( 62.93954589823548673, -14.63888995810886051, -9.517290379660753530 ) ) ;
#1267 = CARTESIAN_POINT ( 'NONE',  ( 120.2274548109119934, -9.859900752359374465, -12.68260735090039404 ) ) ;
#1268 = CARTESIAN_POINT ( 'NONE',  ( 114.1009748109119784, -5.574606645277164318, -18.38911715685844683 ) ) ;
#1269 = ORIENTED_EDGE ( 'NONE', *, *, #42780, .T. ) ;
#1270 = CARTESIAN_POINT ( 'NONE',  ( 136.1673833308529424, -7.073431297710629728, -7.951451023228969461 ) ) ;
#1271 = CARTESIAN_POINT ( 'NONE',  ( 119.7434548109119703, -5.853704621469987934, -5.454671103420249523 ) ) ;
#1272 = CARTESIAN_POINT ( 'NONE',  ( 112.6356140045247827, 0.1403307496149616695, -15.46607636864997204 ) ) ;
#1273 = CARTESIAN_POINT ( 'NONE',  ( 119.3765548109119834, -10.15424416112533912, -14.75197769757731336 ) ) ;
#1274 = CARTESIAN_POINT ( 'NONE',  ( 120.0005481442453146, -4.153390946401325223, -8.397313243818185668 ) ) ;
#1275 = CARTESIAN_POINT ( 'NONE',  ( 116.1431348109119881, 0.1319031606808879209, -14.10382304977623669 ) ) ;
#1276 = CARTESIAN_POINT ( 'NONE',  ( 85.90654841308125356, -27.46059110997621033, -8.671423226218806235 ) ) ;
#1277 = CARTESIAN_POINT ( 'NONE',  ( 109.5796765045248122, -7.250697342233347165, -19.15521520033831138 ) ) ;
#1278 = CARTESIAN_POINT ( 'NONE',  ( 123.1772414775786189, -5.574606645277164318, -18.38911715685844683 ) ) ;
#1279 = CARTESIAN_POINT ( 'NONE',  ( 123.6310548109119765, -4.153390946401325223, -8.397313243818185668 ) ) ;
#1280 = DIRECTION ( 'NONE',  ( -0.7871354856660162103, -0.4483307682966942709, -0.4235767337848251879 ) ) ;
#1281 = CARTESIAN_POINT ( 'NONE',  ( 112.5126281442453120, 0.1319031606808870605, -14.10382304977625090 ) ) ;
#1282 = CARTESIAN_POINT ( 'NONE',  ( 123.1466579359119891, -5.444069387712269226, -19.60292469916370450 ) ) ;
#1283 = CIRCLE ( 'NONE', #23133, 1.499999999999998002 ) ;
#1284 = CARTESIAN_POINT ( 'NONE',  ( 114.3024890045248156, 0.8980012041604421569, -15.77991374673208469 ) ) ;
#1285 = CARTESIAN_POINT ( 'NONE',  ( -13.48289411298945595, -4.891473392625994343, -19.20673326947127180 ) ) ;
#1286 = CARTESIAN_POINT ( 'NONE',  ( 82.57348731610973402, -31.56754274340543986, -22.29195438618578606 ) ) ;
#1287 = CARTESIAN_POINT ( 'NONE',  ( 115.8027748109119841, -0.4660016031367893996, -10.09054647747474043 ) ) ;
#1288 = CARTESIAN_POINT ( 'NONE',  ( 118.2987481442453088, -1.561330072975668504, -17.79121239304076951 ) ) ;
#1289 = CARTESIAN_POINT ( 'NONE',  ( 105.6208483795248299, -0.7896495226426338832, -9.318865927141430916 ) ) ;
#1290 = CARTESIAN_POINT ( 'NONE',  ( 114.2711548109119803, -9.988377603198976828, -10.36322818467138340 ) ) ;
#1291 = FACE_OUTER_BOUND ( 'NONE', #9136, .T. ) ;
#1292 = ORIENTED_EDGE ( 'NONE', *, *, #34484, .F. ) ;
#1293 = CARTESIAN_POINT ( 'NONE',  ( 80.41643495664496299, -3.865424785743087899, -10.89321520033831447 ) ) ;
#1294 = CARTESIAN_POINT ( 'NONE',  ( 118.1285681442453068, -7.893985811506177619, -18.51759400769804742 ) ) ;
#1295 = CARTESIAN_POINT ( 'NONE',  ( 122.8368814775786291, -7.894159318335828068, -9.358103419637847864 ) ) ;
#1296 = DIRECTION ( 'NONE',  ( 1.000000000000000000, 0.000000000000000000, 0.000000000000000000 ) ) ;
#1297 = CARTESIAN_POINT ( 'NONE',  ( 114.8951481442453115, -8.899110576539710493, -16.42337572283490132 ) ) ;
#1298 = CARTESIAN_POINT ( 'NONE',  ( 122.7234281442452755, -5.638512984488999180, -18.83840828888717311 ) ) ;
#1299 = CARTESIAN_POINT ( 'NONE',  ( 113.3301452545248083, 0.8980012041604421569, -11.00651665394454071 ) ) ;
#1300 = CARTESIAN_POINT ( 'NONE',  ( 118.1852948109119836, -4.153390946401325223, -8.397313243818185668 ) ) ;
#1301 = CARTESIAN_POINT ( 'NONE',  ( 116.7898211891027671, -3.191637679206685618, -18.31208751218940733 ) ) ;
#1302 = DIRECTION ( 'NONE',  ( 0.000000000000000000, 0.4669533266896290780, 0.8842819633428518067 ) ) ;
#1303 = ORIENTED_EDGE ( 'NONE', *, *, #23992, .F. ) ;
#1304 = CARTESIAN_POINT ( 'NONE',  ( 120.7852516859119731, -0.6942167230862511529, -9.935906262978006609 ) ) ;
#1305 = CARTESIAN_POINT ( 'NONE',  ( 117.5613014775786525, 0.9020085738987339008, -11.91225656197089222 ) ) ;
#1306 = ORIENTED_EDGE ( 'NONE', *, *, #37165, .T. ) ;
#1307 = CARTESIAN_POINT ( 'NONE',  ( 125.5030348109119558, -6.222761293078241884, -8.102969835052219238 ) ) ;
#1308 = CARTESIAN_POINT ( 'NONE',  ( -13.00275943959160685, -4.132914642980755282, -7.537981892864975109 ) ) ;
#1309 = DIRECTION ( 'NONE',  ( -0.2768435750659241079, -0.3568721902840695792, 0.8921882507333129819 ) ) ;
#1310 = CARTESIAN_POINT ( 'NONE',  ( 116.5402214775786405, -9.565557343593413364, -10.61323700422348004 ) ) ;
#1311 = CARTESIAN_POINT ( 'NONE',  ( 112.0127758072985529, 0.3208234527006404435, -15.99825685930877661 ) ) ;
#1312 = CARTESIAN_POINT ( 'NONE',  ( 124.5198337258228918, -9.766803879443250125, -12.40978687061016572 ) ) ;
#1313 = CARTESIAN_POINT ( 'NONE',  ( 122.7801548109119665, -6.222761293078241884, -8.102969835052219238 ) ) ;
#1314 = EDGE_CURVE ( 'NONE', #7942, #42460, #4050, .T. ) ;
#1315 = CARTESIAN_POINT ( 'NONE',  ( 128.2184548109119930, -3.719473736431747390, -16.16631137400202078 ) ) ;
#1316 = CARTESIAN_POINT ( 'NONE',  ( 124.4819548109119722, -2.084020599724406786, -8.691656652584148546 ) ) ;
#1317 = CARTESIAN_POINT ( 'NONE',  ( 65.55689610126231059, -13.67296395165911704, -12.39321520033831447 ) ) ;
#1318 = CARTESIAN_POINT ( 'NONE',  ( 124.5386814775786206, -4.153390946401325223, -8.397313243818185668 ) ) ;
#1319 = CARTESIAN_POINT ( 'NONE',  ( 114.3846081442453197, -10.63000616557722466, -14.87417383870573495 ) ) ;
#1320 = CARTESIAN_POINT ( 'NONE',  ( 121.1918081442452859, 0.9020085738987339008, -11.91225656197089222 ) ) ;
#1321 = CARTESIAN_POINT ( 'NONE',  ( 126.4106614775786284, -6.222761293078241884, -8.102969835052219238 ) ) ;
#1322 = DIRECTION ( 'NONE',  ( 0.000000000000000000, 0.000000000000000000, -1.000000000000000000 ) ) ;
#1323 = CARTESIAN_POINT ( 'NONE',  ( 118.9794681442453026, -0.8288870151387760510, -10.36305467784173118 ) ) ;
#1324 = ORIENTED_EDGE ( 'NONE', *, *, #3945, .T. ) ;
#1325 = CARTESIAN_POINT ( 'NONE',  ( 120.1707281442453166, 0.2603800115204892296, -16.42320221600525088 ) ) ;
#1326 = CARTESIAN_POINT ( 'NONE',  ( 114.9970202545248412, 0.1403307496149616695, -11.32035403202665336 ) ) ;
#1327 = DIRECTION ( 'NONE',  ( 0.000000000000000000, -0.3713878862591642460, 0.9284778069183722282 ) ) ;
#1328 = CARTESIAN_POINT ( 'NONE',  ( 114.2144281442453178, -1.833838273342658809, -17.42832698103878286 ) ) ;
#1329 = CARTESIAN_POINT ( 'NONE',  ( 120.2296266859119669, -0.06289925094097945091, -9.412459353600674206 ) ) ;
#1330 = CARTESIAN_POINT ( 'NONE',  ( 59.24641515291911986, -13.72835195454734425, -7.393215200338315363 ) ) ;
#1331 = ORIENTED_EDGE ( 'NONE', *, *, #39829, .F. ) ;
#1332 = CARTESIAN_POINT ( 'NONE',  ( 121.8158014775786171, -4.153390946401325223, -8.397313243818185668 ) ) ;
#1333 = DIRECTION ( 'NONE',  ( 1.000000000000000000, 0.000000000000000000, 0.000000000000000000 ) ) ;
#1334 = CARTESIAN_POINT ( 'NONE',  ( 123.5633766859119760, -0.06289925094097943703, -9.412459353600674206 ) ) ;
#1335 = CARTESIAN_POINT ( 'NONE',  ( 112.1234697116520920, -8.918491192341182483, -16.31914947962552631 ) ) ;
#1336 = CARTESIAN_POINT ( 'NONE',  ( 107.0099108795247815, -1.325403438956436419, -16.93181055722141792 ) ) ;
#1337 = EDGE_CURVE ( 'NONE', #35799, #17886, #22886, .T. ) ;
#1338 = ORIENTED_EDGE ( 'NONE', *, *, #7480, .F. ) ;
#1339 = CARTESIAN_POINT ( 'NONE',  ( 113.4202548109119846, -10.30919188438810075, -12.61870101168855918 ) ) ;
#1340 = CARTESIAN_POINT ( 'NONE',  ( 88.41031260927115909, -11.49916342651943957, -13.77494911842194369 ) ) ;
#1341 = CARTESIAN_POINT ( 'NONE',  ( 118.9794681442453026, -0.8288870151387760510, -10.36305467784173118 ) ) ;
#1342 = CARTESIAN_POINT ( 'NONE',  ( 126.2184548109108420, -4.131345727441387616, -8.447100459282841811 ) ) ;
#1343 = FILL_AREA_STYLE_COLOUR ( '', #11399 ) ;
#1344 = DIRECTION ( 'NONE',  ( 0.000000000000000000, -0.3818493186865927203, 0.9242245927363029745 ) ) ;
#1345 = CARTESIAN_POINT ( 'NONE',  ( 114.8447400025837197, -2.311015703046749081, -18.04188382666269064 ) ) ;
#1346 = EDGE_CURVE ( 'NONE', #29689, #5805, #26565, .T. ) ;
#1347 = CARTESIAN_POINT ( 'NONE',  ( 111.8886348109120092, -3.383040157471821630, -19.15922257007629170 ) ) ;
#1348 = ORIENTED_EDGE ( 'NONE', *, *, #972, .F. ) ;
#1349 = EDGE_CURVE ( 'NONE', #34283, #41097, #1533, .T. ) ;
#1350 = CARTESIAN_POINT ( 'NONE',  ( 114.7192077545248594, -2.791137627527939813, -18.39754474579286025 ) ) ;
#1351 = CARTESIAN_POINT ( 'NONE',  ( 119.5467348109119712, -4.089484607189486809, -7.948022111789456723 ) ) ;
#1352 = CARTESIAN_POINT ( 'NONE',  ( 137.1399781294032039, -8.476060746497974918, -17.35023159224490996 ) ) ;
#1353 = EDGE_LOOP ( 'NONE', ( #6893, #31759, #18475, #18995, #18699 ) ) ;
#1354 = DIRECTION ( 'NONE',  ( -3.317300593186674996E-33, 1.195183497228115774E-16, 1.000000000000000000 ) ) ;
#1355 = CARTESIAN_POINT ( 'NONE',  ( 125.0492214775786266, -6.344957434206665248, -7.627207830600338134 ) ) ;
#1356 = EDGE_CURVE ( 'NONE', #23574, #14619, #40404, .T. ) ;
#1357 = CARTESIAN_POINT ( 'NONE',  ( 111.0381921295247878, -9.868328341294093420, -13.39321520033836599 ) ) ;
#1358 = CARTESIAN_POINT ( 'NONE',  ( 124.0281414775786146, -7.643976991954077427, -18.09477374809248928 ) ) ;
#1359 = VERTEX_POINT ( 'NONE', #24815 ) ;
#1360 = CARTESIAN_POINT ( 'NONE',  ( 117.2776681442452968, -5.638512984488999180, -18.83840828888717311 ) ) ;
#1361 = CYLINDRICAL_SURFACE ( 'NONE', #27421, 5.000000000000004441 ) ;
#1362 = CARTESIAN_POINT ( 'NONE',  ( 64.61935771200890599, -37.86087448816891765, -4.893215200338314474 ) ) ;
#1363 = EDGE_CURVE ( 'NONE', #2333, #17, #20035, .T. ) ;
#1364 = CARTESIAN_POINT ( 'NONE',  ( 112.0020881442453344, -9.565557343593402706, -10.61323700422347649 ) ) ;
#1365 = ADVANCED_FACE ( 'NONE', ( #21395 ), #4280, .T. ) ;
#1366 = EDGE_CURVE ( 'NONE', #32579, #11479, #1090, .T. ) ;
#1367 = CARTESIAN_POINT ( 'NONE',  ( 136.7478768735726931, -5.372037007781774953, -7.792893957613936884 ) ) ;
#1368 = CARTESIAN_POINT ( 'NONE',  ( 124.8223148109119762, 0.9020085738987339008, -11.91225656197089222 ) ) ;
#1369 = DIRECTION ( 'NONE',  ( 0.000000000000000000, 0.6004852223388321697, -0.7996358532186279566 ) ) ;
#1370 = CARTESIAN_POINT ( 'NONE',  ( 59.36680634945873436, -12.84644995903807541, -9.393215200338314474 ) ) ;
#1371 = CARTESIAN_POINT ( 'NONE',  ( 112.0588148109119828, -9.859900752359374465, -12.68260735090039404 ) ) ;
#1372 = CARTESIAN_POINT ( 'NONE',  ( 125.2194014775786286, 0.1319031606808879209, -14.10382304977623669 ) ) ;
#1373 = CARTESIAN_POINT ( 'NONE',  ( 123.9146881442452894, -10.15424416112533912, -14.75197769757731336 ) ) ;
#1374 = DIRECTION ( 'NONE',  ( -1.000000000000000000, 0.000000000000000000, 0.000000000000000000 ) ) ;
#1375 = CARTESIAN_POINT ( 'NONE',  ( 118.5823814775786360, -1.834011780172310813, -8.268836392978581529 ) ) ;
#1376 = ORIENTED_EDGE ( 'NONE', *, *, #23481, .F. ) ;
#1377 = CARTESIAN_POINT ( 'NONE',  ( 114.9275671295247889, -10.62599879583958540, -13.39321520033831447 ) ) ;
#1378 = CARTESIAN_POINT ( 'NONE',  ( 112.0105358795248804, -8.402594152722688392, -9.854619843455216355 ) ) ;
#1379 = CARTESIAN_POINT ( 'NONE',  ( 109.7185827545247889, -6.936859964151250502, -8.388885654883777576 ) ) ;
#1380 = CARTESIAN_POINT ( 'NONE',  ( 126.2940345447968156, -9.794764728668093667, -12.36025030967080163 ) ) ;
#1381 = CARTESIAN_POINT ( 'NONE',  ( 114.6115148109119986, -3.383040157471821630, -19.15922257007629170 ) ) ;
#1382 = ORIENTED_EDGE ( 'NONE', *, *, #8038, .F. ) ;
#1383 = CARTESIAN_POINT ( 'NONE',  ( 115.4056881442453459, -2.084020599724406786, -8.691656652584148546 ) ) ;
#1384 = CARTESIAN_POINT ( 'NONE',  ( 108.8851452545248151, 0.8980012041604421569, -11.00651665394454071 ) ) ;
#1385 = FACE_OUTER_BOUND ( 'NONE', #41858, .T. ) ;
#1386 = CARTESIAN_POINT ( 'NONE',  ( 120.1511205389825250, -6.126425863531494542, -18.50366489541501380 ) ) ;
#1387 =( BOUNDED_SURFACE ( )  B_SPLINE_SURFACE ( 1, 2, ( 
 ( #25518, #884, #11607, #39421, #17994, #43067, #18455, #15247, #18222, #31893, #11835, #7954, #38727, #660, #28492, #7499, #35298, #8412, #14803, #32782, #8186, #35982, #4753, #4300, #32116, #1554, #15476, #25294, #18674, #29382, #11386, #19120, #23224, #22757, #39871, #43975, #8636, #36434, #33004, #2459, #26188, #25966, #12290, #33913, #40097, #8856, #33684, #33234, #2229, #22537, #9315, #36657, #9540, #1778, #23455, #16381, #43522, #5430, #43749, #19570, #26641, #5201, #15704, #20031, #44429 ),
 ( #37103, #12971, #19347, #37340, #5878, #2007, #30508, #26414, #26867, #16158, #15933, #5650, #29832, #29606, #12516, #40324, #9088, #40555, #22990, #33449, #36880, #12739, #30062, #19799, #30283, #44209, #40782, #6112, #2684, #16615, #37574, #7017, #13642, #17724, #20259, #34145, #13197, #31623, #3586, #20487, #41904, #34586, #27772, #27551, #6344, #41019, #31396, #24572, #44885, #10222, #20708, #41463, #2914, #10446, #10003, #27097, #31180, #9773, #23685, #16845, #34802, #13423, #30737, #44660, #21142 ) ),
 .UNSPECIFIED., .F., .F., .T. ) 
 B_SPLINE_SURFACE_WITH_KNOTS ( ( 2, 2 ),
 ( 3, 2, 2, 2, 2, 2, 2, 2, 2, 2, 2, 2, 2, 2, 2, 2, 2, 2, 2, 2, 2, 2, 2, 2, 2, 2, 2, 2, 2, 2, 2, 2, 3 ),
 ( 0.000000000000000000, 1.000000000000000000 ),
 ( 0.000000000000000000, 0.03125000000000000000, 0.06250000000000000000, 0.09375000000000000000, 0.1250000000000000000, 0.1562500000000000000, 0.1875000000000000000, 0.2187500000000000000, 0.2500000000000000000, 0.2812500000000000000, 0.3125000000000000000, 0.3437500000000000000, 0.3750000000000000000, 0.4062500000000000000, 0.4375000000000000000, 0.4687500000000000000, 0.5000000000000000000, 0.5312500000000000000, 0.5625000000000000000, 0.5937500000000000000, 0.6250000000000000000, 0.6562500000000000000, 0.6875000000000000000, 0.7187500000000000000, 0.7500000000000000000, 0.7812500000000000000, 0.8125000000000000000, 0.8437500000000000000, 0.8750000000000000000, 0.9062500000000000000, 0.9375000000000000000, 0.9687500000000000000, 1.000000000000000000 ),
 .UNSPECIFIED. ) 
 GEOMETRIC_REPRESENTATION_ITEM ( )  RATIONAL_B_SPLINE_SURFACE ( (
 ( 1.000000000000000000, 0.9238795325112869605, 1.000000000000000000, 0.9238795325112869605, 1.000000000000000000, 0.9238795325112869605, 1.000000000000000000, 0.9238795325112869605, 1.000000000000000000, 0.9238795325112869605, 1.000000000000000000, 0.9238795325112869605, 1.000000000000000000, 0.9238795325112869605, 1.000000000000000000, 0.9238795325112869605, 1.000000000000000000, 0.9238795325112869605, 1.000000000000000000, 0.9238795325112869605, 1.000000000000000000, 0.9238795325112869605, 1.000000000000000000, 0.9238795325112869605, 1.000000000000000000, 0.9238795325112869605, 1.000000000000000000, 0.9238795325112869605, 1.000000000000000000, 0.9238795325112869605, 1.000000000000000000, 0.9238795325112869605, 1.000000000000000000, 0.9238795325112869605, 1.000000000000000000, 0.9238795325112869605, 1.000000000000000000, 0.9238795325112869605, 1.000000000000000000, 0.9238795325112869605, 1.000000000000000000, 0.9238795325112869605, 1.000000000000000000, 0.9238795325112869605, 1.000000000000000000, 0.9238795325112869605, 1.000000000000000000, 0.9238795325112869605, 1.000000000000000000, 0.9238795325112869605, 1.000000000000000000, 0.9238795325112869605, 1.000000000000000000, 0.9238795325112869605, 1.000000000000000000, 0.9238795325112869605, 1.000000000000000000, 0.9238795325112869605, 1.000000000000000000, 0.9238795325112869605, 1.000000000000000000, 0.9238795325112869605, 1.000000000000000000, 0.9238795325112869605, 1.000000000000000000),
 ( 1.000000000000000000, 0.9238795325112869605, 1.000000000000000000, 0.9238795325112869605, 1.000000000000000000, 0.9238795325112869605, 1.000000000000000000, 0.9238795325112869605, 1.000000000000000000, 0.9238795325112869605, 1.000000000000000000, 0.9238795325112869605, 1.000000000000000000, 0.9238795325112869605, 1.000000000000000000, 0.9238795325112869605, 1.000000000000000000, 0.9238795325112869605, 1.000000000000000000, 0.9238795325112869605, 1.000000000000000000, 0.9238795325112869605, 1.000000000000000000, 0.9238795325112869605, 1.000000000000000000, 0.9238795325112869605, 1.000000000000000000, 0.9238795325112869605, 1.000000000000000000, 0.9238795325112869605, 1.000000000000000000, 0.9238795325112869605, 1.000000000000000000, 0.9238795325112869605, 1.000000000000000000, 0.9238795325112869605, 1.000000000000000000, 0.9238795325112869605, 1.000000000000000000, 0.9238795325112869605, 1.000000000000000000, 0.9238795325112869605, 1.000000000000000000, 0.9238795325112869605, 1.000000000000000000, 0.9238795325112869605, 1.000000000000000000, 0.9238795325112869605, 1.000000000000000000, 0.9238795325112869605, 1.000000000000000000, 0.9238795325112869605, 1.000000000000000000, 0.9238795325112869605, 1.000000000000000000, 0.9238795325112869605, 1.000000000000000000, 0.9238795325112869605, 1.000000000000000000, 0.9238795325112869605, 1.000000000000000000, 0.9238795325112869605, 1.000000000000000000, 0.9238795325112869605, 1.000000000000000000) ) ) 
 REPRESENTATION_ITEM ( '' )  SURFACE ( )  );
#1388 = DIRECTION ( 'NONE',  ( 0.9609149988134839671, -0.1028163501681660097, 0.2570431154366504822 ) ) ;
#1389 = DIRECTION ( 'NONE',  ( 1.000000000000000000, 0.000000000000000000, 0.000000000000000000 ) ) ;
#1390 = CARTESIAN_POINT ( 'NONE',  ( 117.2209414775786485, -7.893985811506177619, -18.51759400769804742 ) ) ;
#1391 = CARTESIAN_POINT ( 'NONE',  ( 109.2324108795247923, -8.938348069036489818, -9.318865927141430916 ) ) ;
#1392 = CARTESIAN_POINT ( 'NONE',  ( 112.5661608795247872, -1.325403438956436419, -16.93181055722141792 ) ) ;
#1393 = ORIENTED_EDGE ( 'NONE', *, *, #39499, .F. ) ;
#1394 = DIRECTION ( 'NONE',  ( 1.000000000000000000, 0.000000000000000000, -0.000000000000000000 ) ) ;
#1395 = CARTESIAN_POINT ( 'NONE',  ( 118.1285681442453068, -2.084020599724406786, -8.691656652584148546 ) ) ;
#1396 = CARTESIAN_POINT ( 'NONE',  ( 116.1431348109119881, -10.30919188438810075, -12.61870101168855918 ) ) ;
#1397 = CARTESIAN_POINT ( 'NONE',  ( 75.95778847736514194, -3.256761025687008537, -10.39321520033831625 ) ) ;
#1398 = CARTESIAN_POINT ( 'NONE',  ( 125.2194014775786286, 0.1319031606808879209, -14.10382304977623669 ) ) ;
#1399 = CARTESIAN_POINT ( 'NONE',  ( 124.9924948109119924, -5.574606645277164318, -18.38911715685844683 ) ) ;
#1400 = CARTESIAN_POINT ( 'NONE',  ( 116.6536748109119941, -10.15424416112533912, -14.75197769757731336 ) ) ;
#1401 = ORIENTED_EDGE ( 'NONE', *, *, #11163, .F. ) ;
#1402 = CARTESIAN_POINT ( 'NONE',  ( 123.7022829359119811, -5.367793381288652910, -18.78638297431638904 ) ) ;
#1403 = CARTESIAN_POINT ( 'NONE',  ( 113.5823964071292806, 0.2518737723193609224, -14.64321520033831447 ) ) ;
#1404 = CARTESIAN_POINT ( 'NONE',  ( 116.4267681442453153, -6.222761293078241884, -8.102969835052219238 ) ) ;
#1405 = ORIENTED_EDGE ( 'NONE', *, *, #32534, .F. ) ;
#1406 = AXIS2_PLACEMENT_3D ( 'NONE', #27701, #24497, #41617 ) ;
#1407 = CARTESIAN_POINT ( 'NONE',  ( 75.95778847736514194, -3.256761025687008537, -15.89321520033831447 ) ) ;
#1408 = CARTESIAN_POINT ( 'NONE',  ( 114.7816948109119863, 0.5811942927096154232, -14.16772938898807155 ) ) ;
#1409 = CARTESIAN_POINT ( 'NONE',  ( 106.5931921295248372, -9.868328341294093420, -13.39321520033831447 ) ) ;
#1410 = CARTESIAN_POINT ( 'NONE',  ( 112.2857214775786474, -5.574606645277164318, -18.38911715685844683 ) ) ;
#1411 = VERTEX_POINT ( 'NONE', #42600 ) ;
#1412 = VERTEX_POINT ( 'NONE', #25272 ) ;
#1413 = CARTESIAN_POINT ( 'NONE',  ( 121.5888948109119809, 0.1319031606808879209, -14.10382304977623669 ) ) ;
#1414 = CARTESIAN_POINT ( 'NONE',  ( 117.3911214775786505, -7.894159318335828068, -9.358103419637847864 ) ) ;
#1415 = DIRECTION ( 'NONE',  ( 0.000000000000000000, 0.000000000000000000, 1.000000000000000000 ) ) ;
#1416 = CARTESIAN_POINT ( 'NONE',  ( 116.0980381415389218, -0.1020945015694922492, -15.74893487844867401 ) ) ;
#1417 = ORIENTED_EDGE ( 'NONE', *, *, #29638, .T. ) ;
#1418 = CARTESIAN_POINT ( 'NONE',  ( 70.19189222814998175, -60.76597359474132531, -37.50918677187066663 ) ) ;
#1419 = CARTESIAN_POINT ( 'NONE',  ( 71.50489436060276205, -24.57757939319463958, -4.893215200338314474 ) ) ;
#1420 = CARTESIAN_POINT ( 'NONE',  ( 112.3578015045248861, -2.477300249445798297, -7.631215200338321125 ) ) ;
#1421 = CARTESIAN_POINT ( 'NONE',  ( 116.8238548109119819, -4.089484607189486809, -7.948022111789456723 ) ) ;
#1423 = CARTESIAN_POINT ( 'NONE',  ( 115.3489614775786407, -0.8288870151387760510, -10.36305467784173118 ) ) ;
#1422 = CARTESIAN_POINT ( 'NONE',  ( 125.1059481442452750, -1.833838273342660141, -17.42832698103878286 ) ) ;
#1424 = ADVANCED_FACE ( 'NONE', ( #42377 ), #25497, .T. ) ;
#1425 = CARTESIAN_POINT ( 'NONE',  ( 121.0216281442452981, -7.894159318335828068, -9.358103419637847864 ) ) ;
#1426 = DIRECTION ( 'NONE',  ( 0.000000000000000000, 0.000000000000000000, 1.000000000000000000 ) ) ;
#1427 = ORIENTED_EDGE ( 'NONE', *, *, #41467, .F. ) ;
#1428 = CARTESIAN_POINT ( 'NONE',  ( 118.2987481442453088, -7.894159318335828068, -9.358103419637847864 ) ) ;
#1429 = CARTESIAN_POINT ( 'NONE',  ( 125.3328548109119964, -0.8288870151387760510, -10.36305467784173118 ) ) ;
#1430 = CARTESIAN_POINT ( 'NONE',  ( 111.5243640045248412, -10.62599879583958717, -11.00651665394454604 ) ) ;
#1431 = CARTESIAN_POINT ( 'NONE',  ( 116.2471765045247594, -2.791137627527939813, -8.388885654883777576 ) ) ;
#1432 = CARTESIAN_POINT ( 'NONE',  ( 115.5526452545247622, 0.8980012041604421569, -11.00651665394454071 ) ) ;
#1433 = AXIS2_PLACEMENT_3D ( 'NONE', #39088, #10833, #7857 ) ;
#1434 = CARTESIAN_POINT ( 'NONE',  ( 118.1285681442453068, -7.893985811506177619, -18.51759400769804742 ) ) ;
#1435 = ORIENTED_EDGE ( 'NONE', *, *, #6611, .F. ) ;
#1436 = CARTESIAN_POINT ( 'NONE',  ( 122.1561614775786353, -0.4660016031367893996, -10.09054647747474043 ) ) ;
#1437 = CARTESIAN_POINT ( 'NONE',  ( 67.37136766119182596, -67.53150897494617766, -41.09057840265009531 ) ) ;
#1438 = CARTESIAN_POINT ( 'NONE',  ( 105.9681140045248355, -10.62599879583958717, -11.00651665394454604 ) ) ;
#1439 = CARTESIAN_POINT ( 'NONE',  ( 116.3700414775786527, -5.638512984488999180, -18.83840828888717311 ) ) ;
#1440 = CARTESIAN_POINT ( 'NONE',  ( 118.9227414775786400, -10.63000616557722466, -14.87417383870573495 ) ) ;
#1441 = CARTESIAN_POINT ( 'NONE',  ( 126.5010429760475574, -10.00445151461793536, -13.30003832786311513 ) ) ;
#1442 = CARTESIAN_POINT ( 'NONE',  ( 117.1639140680481148, -11.17155048450423571, -5.478470727163857745 ) ) ;
#1443 = CARTESIAN_POINT ( 'NONE',  ( 107.0793640045248196, 0.1403307496149616695, -15.46607636864997204 ) ) ;
#1444 = VERTEX_POINT ( 'NONE', #7933 ) ;
#1445 = CARTESIAN_POINT ( 'NONE',  ( 115.6915515045247531, -2.477300249445798297, -7.631215200338321125 ) ) ;
#1446 = AXIS2_PLACEMENT_3D ( 'NONE', #14470, #25412, #11053 ) ;
#1447 = CARTESIAN_POINT ( 'NONE',  ( 83.75466360696344736, -7.807702403958562520, -8.143215200338314474 ) ) ;
#1448 = CARTESIAN_POINT ( 'NONE',  ( 118.7525614775786380, -1.833838273342659253, -17.42832698103878286 ) ) ;
#1449 = CARTESIAN_POINT ( 'NONE',  ( 113.3995983795247895, -8.402594152722688392, -16.93181055722141792 ) ) ;
#1450 = CARTESIAN_POINT ( 'NONE',  ( 105.6208483795248299, -0.7896495226426338832, -9.318865927141430916 ) ) ;
#1451 = AXIS2_PLACEMENT_3D ( 'NONE', #41210, #27296, #19768 ) ;
#1452 = CARTESIAN_POINT ( 'NONE',  ( 112.5126281442453120, 0.1319031606808879209, -14.10382304977623669 ) ) ;
#1453 = DIRECTION ( 'NONE',  ( 0.000000000000000000, 0.9284778069183720062, 0.3713878862591650232 ) ) ;
#1454 = CARTESIAN_POINT ( 'NONE',  ( 112.7962614775786676, -6.222761293078241884, -8.102969835052219238 ) ) ;
#1455 = CARTESIAN_POINT ( 'NONE',  ( 119.2631014775786298, 0.2603800115204892296, -16.42320221600525088 ) ) ;
#1456 = ORIENTED_EDGE ( 'NONE', *, *, #21137, .F. ) ;
#1457 = CARTESIAN_POINT ( 'NONE',  ( 117.8449348109119938, -1.833838273342659253, -17.42832698103878286 ) ) ;
#1458 = CARTESIAN_POINT ( 'NONE',  ( 116.8805814775786445, -6.344957434206662583, -7.627207830600332805 ) ) ;
#1459 = CARTESIAN_POINT ( 'NONE',  ( 120.9649014775786355, -3.383040157471821630, -19.15922257007629170 ) ) ;
#1460 = CARTESIAN_POINT ( 'NONE',  ( 121.4187148109119789, -3.505236298600246325, -18.68346056562440793 ) ) ;
#1461 = ORIENTED_EDGE ( 'NONE', *, *, #33249, .T. ) ;
#1462 = CARTESIAN_POINT ( 'NONE',  ( 123.6310548109119765, -4.153390946401325223, -8.397313243818185668 ) ) ;
#1463 = CARTESIAN_POINT ( 'NONE',  ( 121.0216281442452981, -1.561330072975668948, -17.79121239304076951 ) ) ;
#1464 = CARTESIAN_POINT ( 'NONE',  ( 112.7962614775786676, -6.222761293078241884, -8.102969835052219238 ) ) ;
#1465 = CARTESIAN_POINT ( 'NONE',  ( 120.8514481442452961, -7.893985811506177619, -18.51759400769804742 ) ) ;
#1466 = DIRECTION ( 'NONE',  ( 0.000000000000000000, 0.5905882410490338463, 0.8069730661766898461 ) ) ;
#1467 = CARTESIAN_POINT ( 'NONE',  ( 86.36631847702263087, -24.14644159042263993, -12.62951656296512937 ) ) ;
#1468 = CARTESIAN_POINT ( 'NONE',  ( 114.9275671295247889, 0.1403307496149613920, -13.39321520033831447 ) ) ;
#1469 = VECTOR ( 'NONE', #21811, 1000.000000000000114 ) ;
#1470 = EDGE_CURVE ( 'NONE', #38601, #45059, #39401, .T. ) ;
#1471 = CARTESIAN_POINT ( 'NONE',  ( 123.1466579359119891, -4.360204210389833968, -8.000047426360245240 ) ) ;
#1472 = AXIS2_PLACEMENT_3D ( 'NONE', #16927, #34007, #3226 ) ;
#1473 = CARTESIAN_POINT ( 'NONE',  ( 136.4173705901605160, -10.21087619983626560, -11.18524563227092017 ) ) ;
#1474 = CARTESIAN_POINT ( 'NONE',  ( 114.7249681442453237, -9.565557343593413364, -10.61323700422348004 ) ) ;
#1475 = CARTESIAN_POINT ( 'NONE',  ( 125.6164881442453094, 0.2603800115204892296, -16.42320221600525088 ) ) ;
#1476 = DIRECTION ( 'NONE',  ( 0.000000000000000000, 1.000000000000000000, 0.000000000000000000 ) ) ;
#1477 = B_SPLINE_CURVE_WITH_KNOTS ( 'NONE', 3,
 ( #15560, #4843, #19211, #1859, #4618, #1638, #18762, #32652, #8949, #33090, #22850, #11923, #36741, #18539, #8718, #8274, #32430, #1204, #15118, #32869, #39954, #39730, #29465, #43380, #26051, #8499, #42936, #11697, #22177, #5064, #18979, #36522, #5295, #14589, #10732, #25081, #39436, #14818, #38973 ),
 .UNSPECIFIED., .F., .F.,
 ( 4, 2, 2, 2, 1, 1, 1, 2, 2, 2, 2, 1, 1, 1, 2, 2, 2, 2, 1, 1, 1, 2, 2, 4 ),
 ( 0.000000000000000000, 0.1250000000001450784, 0.1875000000002177425, 0.2187500000002557954, 0.2343750000002725598, 0.2421875000002784162, 0.2460937500002818301, 0.2480468750002813305, 0.2500000000002808309, 0.3750000000002225997, 0.4375000000001940115, 0.4687500000001821321, 0.4843750000001779132, 0.4921875000001740275, 0.4960937500001719735, 0.5000000000001699751, 0.6250000000001478817, 0.6875000000001361133, 0.7187500000001322276, 0.7343750000001287859, 0.7421875000001285638, 0.7460937500001243450, 0.7500000000001200151, 1.000000000000000000 ),
 .UNSPECIFIED. ) ;
#1478 = CARTESIAN_POINT ( 'NONE',  ( 116.1808983795247769, -1.328464889906837199, -9.857681294405580275 ) ) ;
#1479 = CARTESIAN_POINT ( 'NONE',  ( 109.9269421295247753, -9.868328341294093420, -13.39321520033831447 ) ) ;
#1480 = CARTESIAN_POINT ( 'NONE',  ( 115.1787814775786387, -0.1624402480850797581, -16.17319339645315424 ) ) ;
#1481 = CARTESIAN_POINT ( 'NONE',  ( 92.26512299712632625, -23.76310523276723785, -4.893215200338314474 ) ) ;
#1482 = CARTESIAN_POINT ( 'NONE',  ( 122.6213246589382209, -8.341213398351550623, -17.25835129106723542 ) ) ;
#1484 = CARTESIAN_POINT ( 'NONE',  ( 118.6958348109119754, -6.344957434206665248, -7.627207830600338134 ) ) ;
#1483 = CARTESIAN_POINT ( 'NONE',  ( 65.55342193993762123, -16.16218099987542800, -9.830679638262655118 ) ) ;
#1485 = CARTESIAN_POINT ( 'NONE',  ( 121.2485348109119769, -8.899110576539710493, -16.42337572283490132 ) ) ;
#1486 = ORIENTED_EDGE ( 'NONE', *, *, #19177, .T. ) ;
#1487 = CARTESIAN_POINT ( 'NONE',  ( 137.1886586612212113, -7.251019100340859502, -8.638848605701541672 ) ) ;
#1488 = CARTESIAN_POINT ( 'NONE',  ( 66.31928500851137187, -14.71576354012722021, -10.39321520033831625 ) ) ;
#1489 = CARTESIAN_POINT ( 'NONE',  ( 108.1211608795247798, -1.325403438956436419, -16.93181055722141792 ) ) ;
#1490 = CARTESIAN_POINT ( 'NONE',  ( 120.5110881442453206, -3.505236298600246325, -18.68346056562440793 ) ) ;
#1491 = CARTESIAN_POINT ( 'NONE',  ( 123.5176014775786228, -0.8288870151387760510, -10.36305467784173118 ) ) ;
#1492 = CARTESIAN_POINT ( 'NONE',  ( 117.3911214775786505, -7.894159318335828068, -9.358103419637847864 ) ) ;
#1493 = CARTESIAN_POINT ( 'NONE',  ( 121.0016831242421773, -1.016270020561755860, -17.26805140881366896 ) ) ;
#1494 = CARTESIAN_POINT ( 'NONE',  ( 110.2742077545248094, -7.250697342233347165, -7.631215200338321125 ) ) ;
#1495 = CARTESIAN_POINT ( 'NONE',  ( 122.8936081442453059, -9.565557343593413364, -10.61323700422348004 ) ) ;
#1496 = CARTESIAN_POINT ( 'NONE',  ( 123.0070614775786169, -10.15424416112533912, -14.75197769757731336 ) ) ;
#1497 = DIRECTION ( 'NONE',  ( 0.000000000000000000, 0.000000000000000000, -1.000000000000000000 ) ) ;
#1498 = VECTOR ( 'NONE', #3951, 1000.000000000000000 ) ;
#1499 = CARTESIAN_POINT ( 'NONE',  ( 112.5693548109119888, 0.4262465694468579591, -12.03445270309932802 ) ) ;
#1500 = EDGE_CURVE ( 'NONE', #13929, #30417, #29624, .T. ) ;
#1501 = CARTESIAN_POINT ( 'NONE',  ( 119.8823610609119754, -6.340755971794695078, -8.611740276972781771 ) ) ;
#1502 = CARTESIAN_POINT ( 'NONE',  ( 106.1764733795248219, -1.325403438956436419, -9.854619843455211026 ) ) ;
#1503 = CYLINDRICAL_SURFACE ( 'NONE', #31356, 5.999999999999997335 ) ;
#1504 = CARTESIAN_POINT ( 'NONE',  ( 83.65649369947882974, -32.32350872240788675, -21.29440707590126536 ) ) ;
#1505 = CARTESIAN_POINT ( 'NONE',  ( 120.7379948109119709, -10.63000616557722466, -14.87417383870573495 ) ) ;
#1506 = CARTESIAN_POINT ( 'NONE',  ( 117.0507614775786465, -10.30919188438810075, -12.61870101168855918 ) ) ;
#1507 = CARTESIAN_POINT ( 'NONE',  ( 108.2600671295247992, -10.62599879583958540, -13.39321520033831447 ) ) ;
#1508 = CARTESIAN_POINT ( 'NONE',  ( 117.1642148109119859, -9.261995988541697145, -16.69588392320189030 ) ) ;
#1509 = CARTESIAN_POINT ( 'NONE',  ( 88.73939138327467901, -25.99489077589524300, -13.39321520033831625 ) ) ;
#1510 = ORIENTED_EDGE ( 'NONE', *, *, #22776, .F. ) ;
#1511 = DIRECTION ( 'NONE',  ( 1.000000000000000000, 0.000000000000000000, -0.000000000000000000 ) ) ;
#1512 = AXIS2_PLACEMENT_3D ( 'NONE', #9948, #2860, #9716 ) ;
#1513 = CARTESIAN_POINT ( 'NONE',  ( 119.3765548109119834, 0.9020085738987339008, -11.91225656197089222 ) ) ;
#1514 = CARTESIAN_POINT ( 'NONE',  ( 112.0588148109119828, 0.5811942927096154232, -14.16772938898807155 ) ) ;
#1515 = CARTESIAN_POINT ( 'NONE',  ( 0.000000000000000000, 0.000000000000000000, 0.000000000000000000 ) ) ;
#1516 = CARTESIAN_POINT ( 'NONE',  ( 113.0798948109119948, -8.899110576539710493, -16.42337572283490132 ) ) ;
#1517 = CARTESIAN_POINT ( 'NONE',  ( 125.3895814775786448, -7.893985811506177619, -18.51759400769804742 ) ) ;
#1518 = CARTESIAN_POINT ( 'NONE',  ( 110.8298327545248299, -2.477300249445798297, -19.15521520033831138 ) ) ;
#1519 = CARTESIAN_POINT ( 'NONE',  ( 121.5321681442453183, -0.1624402480850797581, -16.17319339645315424 ) ) ;
#1520 = CARTESIAN_POINT ( 'NONE',  ( 111.0001630180080809, 0.7607806665038616689, -14.64321520033831447 ) ) ;
#1521 = CARTESIAN_POINT ( 'NONE',  ( 123.6786990974279945, -6.000569120582374794, -18.26532662605526269 ) ) ;
#1522 = VERTEX_POINT ( 'NONE', #26391 ) ;
#1523 = CARTESIAN_POINT ( 'NONE',  ( 122.5910329359119970, -4.283928203966213211, -7.183505701512925334 ) ) ;
#1524 = CARTESIAN_POINT ( 'NONE',  ( 122.6667014775786413, -7.893985811506177619, -18.51759400769804742 ) ) ;
#1525 = ORIENTED_EDGE ( 'NONE', *, *, #11406, .T. ) ;
#1526 = DIRECTION ( 'NONE',  ( 0.000000000000000000, 0.9284778069183721172, 0.3713878862591650232 ) ) ;
#1527 = CARTESIAN_POINT ( 'NONE',  ( 68.14371629974728251, -1.351251493923715685, -10.39321520033831625 ) ) ;
#1528 = FILL_AREA_STYLE ('',( #35958 ) ) ;
#1529 = CARTESIAN_POINT ( 'NONE',  ( 118.8660148109119774, 0.1319031606808879209, -14.10382304977623669 ) ) ;
#1530 = CARTESIAN_POINT ( 'NONE',  ( 66.05753635973103144, -0.1399854074271419946, -16.39321520033832158 ) ) ;
#1531 = CARTESIAN_POINT ( 'NONE',  ( 64.01282776924008999, -34.86145050234441811, -5.893215200338315363 ) ) ;
#1532 = CARTESIAN_POINT ( 'NONE',  ( 121.7590748109119687, -2.084020599724406786, -8.691656652584148546 ) ) ;
#1533 = LINE ( 'NONE', #39627, #5454 ) ;
#1534 = CARTESIAN_POINT ( 'NONE',  ( 124.5386814775786206, -4.153390946401325223, -8.397313243818185668 ) ) ;
#1535 = CONICAL_SURFACE ( 'NONE', #19024, 1.610000000000000986, 0.9599310885968765916 ) ;
#1536 = CARTESIAN_POINT ( 'NONE',  ( 124.0393428911674505, -11.97802596815495590, -17.05247829970954143 ) ) ;
#1537 = CARTESIAN_POINT ( 'NONE',  ( 118.4122014775786340, -9.859900752359374465, -12.68260735090039404 ) ) ;
#1538 = CARTESIAN_POINT ( 'NONE',  ( 122.6099748109119929, -0.8288870151387760510, -10.36305467784173118 ) ) ;
#1539 = CIRCLE ( 'NONE', #5799, 2.000000000000000000 ) ;
#1540 = CARTESIAN_POINT ( 'NONE',  ( 118.6391081442452986, -4.089484607189486809, -7.948022111789456723 ) ) ;
#1541 = CARTESIAN_POINT ( 'NONE',  ( 117.5045748109119756, 0.5811942927096110934, -14.16772938898807510 ) ) ;
#1542 = CARTESIAN_POINT ( 'NONE',  ( 113.8857702545248003, 0.1403307496149616695, -11.32035403202665336 ) ) ;
#1543 = CARTESIAN_POINT ( 'NONE',  ( 124.0281414775786146, -7.643976991954077427, -18.09477374809248928 ) ) ;
#1544 = ORIENTED_EDGE ( 'NONE', *, *, #25156, .F. ) ;
#1545 = CARTESIAN_POINT ( 'NONE',  ( 121.8158014775786171, -5.638512984488999180, -18.83840828888717311 ) ) ;
#1546 = CARTESIAN_POINT ( 'NONE',  ( 106.4542858795248179, -8.402594152722688392, -9.854619843455216355 ) ) ;
#1547 = CARTESIAN_POINT ( 'NONE',  ( 111.3160046295247838, -4.863998795839590272, -18.39754474579285315 ) ) ;
#1548 = DIRECTION ( 'NONE',  ( 0.000000000000000000, -0.3818493186865936084, 0.9242245927363024194 ) ) ;
#1549 = CARTESIAN_POINT ( 'NONE',  ( 113.3068014775786594, -1.833838273342658809, -17.42832698103878286 ) ) ;
#1550 = CARTESIAN_POINT ( 'NONE',  ( 137.8451516969511204, -2.777385826612674524, -17.42084227926059015 ) ) ;
#1551 = CARTESIAN_POINT ( 'NONE',  ( 125.4463081442452932, -5.638512984488999180, -18.83840828888717311 ) ) ;
#1552 = ORIENTED_EDGE ( 'NONE', *, *, #28698, .T. ) ;
#1553 = CARTESIAN_POINT ( 'NONE',  ( 124.2550481442452792, -0.1624402480850797581, -16.17319339645315424 ) ) ;
#1554 = CARTESIAN_POINT ( 'NONE',  ( 121.4797829359119987, -4.283928203966213211, -7.183505701512925334 ) ) ;
#1555 = CARTESIAN_POINT ( 'NONE',  ( 123.4244704359119709, 1.345710702986147034, -13.97328579221134426 ) ) ;
#1556 = DIRECTION ( 'NONE',  ( 0.000000000000000000, 0.000000000000000000, -1.000000000000000000 ) ) ;
#1557 = CARTESIAN_POINT ( 'NONE',  ( 109.3713171295247832, 0.1403307496149613920, -13.39321520033831447 ) ) ;
#1558 = VERTEX_POINT ( 'NONE', #5408 ) ;
#1559 = CARTESIAN_POINT ( 'NONE',  ( 115.6325948109119821, 0.2603800115204892296, -16.42320221600525088 ) ) ;
#1560 = CARTESIAN_POINT ( 'NONE',  ( 126.0135748109119902, -8.166667518702819706, -8.995218007635861213 ) ) ;
#1561 = CIRCLE ( 'NONE', #20499, 2.445500000000004448 ) ;
#1562 = CARTESIAN_POINT ( 'NONE',  ( 121.4187148109119789, -3.505236298600246325, -18.68346056562440793 ) ) ;
#1563 = CARTESIAN_POINT ( 'NONE',  ( 115.5191414775786569, -6.222761293078241884, -8.102969835052219238 ) ) ;
#1564 = CARTESIAN_POINT ( 'NONE',  ( 143.3676850761856940, -60.26310523276723785, -29.64311716074571379 ) ) ;
#1565 = DIRECTION ( 'NONE',  ( 0.000000000000000000, 0.000000000000000000, -1.000000000000000000 ) ) ;
#1566 = CARTESIAN_POINT ( 'NONE',  ( 113.0798948109119948, -0.4660016031367893996, -10.09054647747474043 ) ) ;
#1567 = EDGE_CURVE ( 'NONE', #31450, #27343, #1756, .T. ) ;
#1568 = CARTESIAN_POINT ( 'NONE',  ( 114.9275671295247889, 0.1403307496149613920, -13.39321520033831447 ) ) ;
#1569 = AXIS2_PLACEMENT_3D ( 'NONE', #40150, #39699, #32835 ) ;
#1570 = CARTESIAN_POINT ( 'NONE',  ( 124.1983214775786166, -8.166667518702819706, -8.995218007635861213 ) ) ;
#1571 = FACE_OUTER_BOUND ( 'NONE', #24276, .T. ) ;
#1572 = EDGE_LOOP ( 'NONE', ( #5834, #26562, #648, #6802 ) ) ;
#1573 = CARTESIAN_POINT ( 'NONE',  ( 113.4769814775786330, -10.63000616557722466, -14.87417383870573495 ) ) ;
#1574 = CARTESIAN_POINT ( 'NONE',  ( 126.1837548109119211, -10.63000616557722466, -14.87417383870573495 ) ) ;
#1575 = CARTESIAN_POINT ( 'NONE',  ( 111.2465515045248168, -6.936859964151197211, -18.39754474579287447 ) ) ;
#1576 = CARTESIAN_POINT ( 'NONE',  ( 122.9503348109119827, -9.859900752359378018, -12.68260735090039759 ) ) ;
#1577 = ORIENTED_EDGE ( 'NONE', *, *, #36322, .F. ) ;
#1578 = CARTESIAN_POINT ( 'NONE',  ( 118.7525614775786380, -8.166667518702819706, -8.995218007635861213 ) ) ;
#1579 = CARTESIAN_POINT ( 'NONE',  ( 109.5102233795247884, -1.325403438956533675, -9.854619843455186157 ) ) ;
#1580 = CARTESIAN_POINT ( 'NONE',  ( 90.04708369096697140, -26.47086644115443832, -13.58986759946190936 ) ) ;
#1581 = CARTESIAN_POINT ( 'NONE',  ( 137.4443952029541265, -4.676119418685644291, -8.312370287078346465 ) ) ;
#1582 = CARTESIAN_POINT ( 'NONE',  ( 114.7249681442453237, -9.565557343593413364, -10.61323700422348004 ) ) ;
#1583 = EDGE_CURVE ( 'NONE', #44494, #13382, #6190, .T. ) ;
#1584 = DIRECTION ( 'NONE',  ( -0.000000000000000000, -0.9284778069183721172, -0.3713878862591650232 ) ) ;
#1585 = VECTOR ( 'NONE', #34649, 1000.000000000000000 ) ;
#1586 = CARTESIAN_POINT ( 'NONE',  ( 125.3439553448850461, -2.495517763063633598, -20.06068668164824231 ) ) ;
#1587 = CARTESIAN_POINT ( 'NONE',  ( 126.2404814775786264, -9.261995988541697145, -16.69588392320189030 ) ) ;
#1588 = CARTESIAN_POINT ( 'NONE',  ( 113.0798948109119948, -0.4660016031367893996, -10.09054647747474043 ) ) ;
#1589 = CARTESIAN_POINT ( 'NONE',  ( 119.7821199480702603, -6.365377317481695663, -18.95617363400926081 ) ) ;
#1590 = CARTESIAN_POINT ( 'NONE',  ( 125.2761281442453054, 0.4262465694468514643, -12.03445270309931736 ) ) ;
#1591 = CARTESIAN_POINT ( 'NONE',  ( 66.31928500851137187, -14.71576354012722021, -16.39321520033831447 ) ) ;
#1592 = CARTESIAN_POINT ( 'NONE',  ( 119.5467348109119712, -4.089484607189486809, -7.948022111789456723 ) ) ;
#1593 = EDGE_CURVE ( 'NONE', #32925, #4162, #18559, .T. ) ;
#1594 = CARTESIAN_POINT ( 'NONE',  ( 120.0572748109119772, -3.383040157471821630, -19.15922257007629170 ) ) ;
#1595 = CARTESIAN_POINT ( 'NONE',  ( 114.8811338361194743, 0.1075849324168598464, -12.14321520033831625 ) ) ;
#1596 = EDGE_CURVE ( 'NONE', #42526, #38298, #5731, .T. ) ;
#1597 = CARTESIAN_POINT ( 'NONE',  ( 116.2471765045247594, -7.250697342233347165, -19.15521520033831138 ) ) ;
#1598 = CARTESIAN_POINT ( 'NONE',  ( 111.8716296295247901, -4.863998795839590272, -8.388885654883775800 ) ) ;
#1599 = CARTESIAN_POINT ( 'NONE',  ( 109.3713171295247832, 0.1403307496149613920, -13.39321520033831447 ) ) ;
#1600 = CARTESIAN_POINT ( 'NONE',  ( 124.9924948109119924, -5.574606645276184658, -18.38911715685858539 ) ) ;
#1601 = CARTESIAN_POINT ( 'NONE',  ( 115.2355081442453155, -10.30919188438810075, -12.61870101168855918 ) ) ;
#1602 = EDGE_LOOP ( 'NONE', ( #39178, #37336, #34760, #27849 ) ) ;
#1603 = CARTESIAN_POINT ( 'NONE',  ( 107.7738952545248310, 0.8980012041604421569, -11.00651665394454071 ) ) ;
#1604 = CARTESIAN_POINT ( 'NONE',  ( 61.69189222814998175, -48.76310523276723785, -24.89321520033831447 ) ) ;
#1605 = CARTESIAN_POINT ( 'NONE',  ( 135.3184548109119874, -7.067465109756605912, -7.812468278694988832 ) ) ;
#1606 = CARTESIAN_POINT ( 'NONE',  ( 112.9512158961590558, -2.263366209404213958, -18.10533625161307114 ) ) ;
#1607 = CARTESIAN_POINT ( 'NONE',  ( 121.1918081442452859, 0.9020085738987339008, -11.91225656197089222 ) ) ;
#1608 = EDGE_CURVE ( 'NONE', #11237, #43860, #16131, .T. ) ;
#1609 = CARTESIAN_POINT ( 'NONE',  ( 109.9963952545248134, 0.8980012041604421569, -11.00651665394454071 ) ) ;
#1610 = CARTESIAN_POINT ( 'NONE',  ( 70.19189222814998175, -50.19222220871606766, -33.27972307567368659 ) ) ;
#1611 = EDGE_LOOP ( 'NONE', ( #21835, #10008, #36290, #40632 ) ) ;
#1612 = CARTESIAN_POINT ( 'NONE',  ( 121.3052614775786395, -7.643976991954073874, -18.09477374809249284 ) ) ;
#1613 = CARTESIAN_POINT ( 'NONE',  ( 119.2063748109119814, -7.894159318335828068, -9.358103419637847864 ) ) ;
#1614 = CARTESIAN_POINT ( 'NONE',  ( 117.7314814775786260, -4.089484607189486809, -7.948022111789456723 ) ) ;
#1615 = B_SPLINE_CURVE_WITH_KNOTS ( 'NONE', 3,
 ( #6118, #2233, #19574, #12520, #5882, #30067, #33917, #30287, #20036, #2688, #44433, #23227, #9093, #16849, #34149, #30741, #13427, #40328, #33691, #33453, #22994, #43979, #12744, #26645, #9319, #2463, #16386, #17866, #39285, #31982, #25162, #24929, #3721, #38374, #28808 ),
 .UNSPECIFIED., .F., .F.,
 ( 4, 2, 2, 1, 1, 1, 2, 2, 2, 2, 1, 1, 2, 2, 2, 2, 1, 1, 2, 2, 4 ),
 ( 0.000000000000000000, 0.1250000000003427814, 0.1875000000005233869, 0.2187500000006241119, 0.2343750000006737666, 0.2421875000006920020, 0.2460937500006886713, 0.2500000000006853407, 0.3750000000005874745, 0.4375000000005401235, 0.4687500000005156431, 0.4843750000005034306, 0.4921875000004973244, 0.5000000000004911627, 0.6250000000004246603, 0.6875000000003913536, 0.7187500000003758105, 0.7343750000003669287, 0.7421875000003596012, 0.7500000000003522738, 1.000000000000000000 ),
 .UNSPECIFIED. ) ;
#1616 = EDGE_CURVE ( 'NONE', #2614, #30875, #3558, .T. ) ;
#1617 = CARTESIAN_POINT ( 'NONE',  ( 118.1222496192402218, -1.111561923218658210, -17.14115599315433158 ) ) ;
#1618 = CARTESIAN_POINT ( 'NONE',  ( 123.1772414775786189, -5.574606645277164318, -18.38911715685844683 ) ) ;
#1619 = CARTESIAN_POINT ( 'NONE',  ( 116.4834948109119779, -7.894159318335828068, -9.358103419637847864 ) ) ;
#1620 = ORIENTED_EDGE ( 'NONE', *, *, #9988, .T. ) ;
#1621 = EDGE_CURVE ( 'NONE', #43791, #29714, #44805, .T. ) ;
#1622 = EDGE_CURVE ( 'NONE', #14508, #21214, #22199, .T. ) ;
#1623 = CARTESIAN_POINT ( 'NONE',  ( 119.9518141859119851, -0.8832429491016019485, -18.19431474523657855 ) ) ;
#1624 = DIRECTION ( 'NONE',  ( 0.9609149988134837450, -0.1028163501681639419, 0.2570431154366518145 ) ) ;
#1625 = CARTESIAN_POINT ( 'NONE',  ( 117.7314814775786260, -5.574606645277164318, -18.38911715685844683 ) ) ;
#1626 = VERTEX_POINT ( 'NONE', #1984 ) ;
#1627 = CARTESIAN_POINT ( 'NONE',  ( 127.0150841466607403, -9.727352494953397155, -15.73620462677915377 ) ) ;
#1628 = CARTESIAN_POINT ( 'NONE',  ( 116.7104014775786425, -0.4660016031367893996, -10.09054647747474043 ) ) ;
#1629 = CARTESIAN_POINT ( 'NONE',  ( 106.2459265045248173, -2.791137627527939813, -8.388885654883777576 ) ) ;
#1630 = CARTESIAN_POINT ( 'NONE',  ( 119.0298762859068944, -1.111561923218657322, -17.14115599315433158 ) ) ;
#1631 = ORIENTED_EDGE ( 'NONE', *, *, #31239, .F. ) ;
#1632 = CIRCLE ( 'NONE', #25668, 7.000000000000000888 ) ;
#1633 = VERTEX_POINT ( 'NONE', #32980 ) ;
#1634 = CARTESIAN_POINT ( 'NONE',  ( 122.5532481442453019, 0.4262465694468514643, -12.03445270309931736 ) ) ;
#1635 = CARTESIAN_POINT ( 'NONE',  ( 118.1285681442453068, -2.084020599724406786, -8.691656652584148546 ) ) ;
#1636 = ORIENTED_EDGE ( 'NONE', *, *, #10913, .F. ) ;
#1637 = DIRECTION ( 'NONE',  ( 0.000000000000000000, 0.6004852223388321697, -0.7996358532186279566 ) ) ;
#1638 = CARTESIAN_POINT ( 'NONE',  ( 61.77599217838784540, -65.91878806257270185, -43.48361792650258906 ) ) ;
#1639 = CARTESIAN_POINT ( 'NONE',  ( 107.6349890045248401, 0.8980012041604421569, -15.77991374673208469 ) ) ;
#1640 = CARTESIAN_POINT ( 'NONE',  ( 117.7882081442453170, -6.344957434206665248, -7.627207830600338134 ) ) ;
#1642 = CARTESIAN_POINT ( 'NONE',  ( 116.5969481442453031, -9.859900752359374465, -12.68260735090039404 ) ) ;
#1641 = CARTESIAN_POINT ( 'NONE',  ( 115.2922348109119781, -10.63000616557722466, -14.87417383870573495 ) ) ;
#1643 =( BOUNDED_CURVE ( )  B_SPLINE_CURVE ( 3, ( #8948, #12374, #30373, #12603 ),
 .UNSPECIFIED., .F., .F. ) 
 B_SPLINE_CURVE_WITH_KNOTS ( ( 4, 4 ),
 ( 4.329840622631089708, 4.712388980384689674 ),
 .UNSPECIFIED. ) 
 CURVE ( )  GEOMETRIC_REPRESENTATION_ITEM ( )  RATIONAL_B_SPLINE_CURVE ( ( 1.000000000000000000, 0.9878418653401740412, 0.9878418653401740412, 1.000000000000000000 ) ) 
 REPRESENTATION_ITEM ( '' )  );
#1644 = CARTESIAN_POINT ( 'NONE',  ( 122.0994348109119443, -10.15424416112533912, -14.75197769757731336 ) ) ;
#1645 = DIRECTION ( 'NONE',  ( 0.000000000000000000, -0.7876185884367603585, 0.6161630946014903243 ) ) ;
#1646 = B_SPLINE_CURVE_WITH_KNOTS ( 'NONE', 3,
 ( #21398, #25274, #21846, #22077, #25046, #17753, #418, #15008, #39171, #7935, #4052, #35741, #32327, #28921, #3614, #11590, #42829, #17530, #31876, #35510, #31427, #641, #14556, #28474, #24818, #41934, #38483, #7258, #42157, #4282, #14334, #35049, #32098, #3833, #866, #14785 ),
 .UNSPECIFIED., .F., .F.,
 ( 4, 2, 2, 2, 2, 1, 2, 2, 2, 2, 2, 2, 2, 1, 2, 2, 2, 2, 4 ),
 ( 0.000000000000000000, 0.06250000000005807854, 0.1250000000001161571, 0.1875000000001742495, 0.2187500000002066125, 0.2343750000002195188, 0.2421875000002254585, 0.2500000000002314260, 0.3750000000001816325, 0.5000000000001318945, 0.6250000000000820455, 0.6875000000000570655, 0.7187500000000491829, 0.7343750000000451861, 0.7421875000000479616, 0.7500000000000507372, 0.8125000000000400791, 0.8750000000000293099, 1.000000000000000000 ),
 .UNSPECIFIED. ) ;
#1647 = EDGE_LOOP ( 'NONE', ( #35667, #1161, #32807, #7658, #11034 ) ) ;
#1648 = CARTESIAN_POINT ( 'NONE',  ( 120.9081748109119872, -4.153390946401325223, -8.397313243818185668 ) ) ;
#1649 = CIRCLE ( 'NONE', #24971, 1.009117809157100254 ) ;
#1650 = EDGE_CURVE ( 'NONE', #26421, #38311, #22043, .T. ) ;
#1651 = DIRECTION ( 'NONE',  ( 0.000000000000000000, -0.6004852223388320587, 0.7996358532186281787 ) ) ;
#1652 = CARTESIAN_POINT ( 'NONE',  ( 111.1076452545248259, 0.8980012041604421569, -11.00651665394454071 ) ) ;
#1653 = CIRCLE ( 'NONE', #29338, 8.000000000000001776 ) ;
#1654 = CARTESIAN_POINT ( 'NONE',  ( 116.6638952545248031, -9.868328341294098749, -15.46607636864997204 ) ) ;
#1655 = CARTESIAN_POINT ( 'NONE',  ( 110.1353015045248469, -2.477300249445798297, -7.631215200338321125 ) ) ;
#1656 = CARTESIAN_POINT ( 'NONE',  ( 120.3976348109119812, -1.834011780172310813, -8.268836392978581529 ) ) ;
#1657 = EDGE_LOOP ( 'NONE', ( #10871, #34682, #25094, #19004 ) ) ;
#1658 = CARTESIAN_POINT ( 'NONE',  ( 121.3619881442452879, -4.089484607189486809, -7.948022111789456723 ) ) ;
#1659 = CARTESIAN_POINT ( 'NONE',  ( 115.5566632127138575, -2.191907684172563986, -18.20049396185734025 ) ) ;
#1660 = CARTESIAN_POINT ( 'NONE',  ( 107.4266296295248821, -4.863998795839590272, -19.15521520033831493 ) ) ;
#1661 = CARTESIAN_POINT ( 'NONE',  ( 116.6536748109119941, 0.9020085738987339008, -11.91225656197089222 ) ) ;
#1662 = CARTESIAN_POINT ( 'NONE',  ( 117.0507614775786465, -10.30919188438810075, -12.61870101168855918 ) ) ;
#1663 = CARTESIAN_POINT ( 'NONE',  ( 111.3319081442453182, -5.568102603702657305, -18.34339073538273013 ) ) ;
#1664 = CARTESIAN_POINT ( 'NONE',  ( 117.1731602005347384, -11.14203525093994251, -5.453018689005371122 ) ) ;
#1665 = VERTEX_POINT ( 'NONE', #26616 ) ;
#1666 = VECTOR ( 'NONE', #17254, 1000.000000000000000 ) ;
#1667 = CARTESIAN_POINT ( 'NONE',  ( -2.527712056240301930, -7.043022739214354289, -7.506402576757856160 ) ) ;
#1668 = CARTESIAN_POINT ( 'NONE',  ( 109.2294421294243136, -10.06703191844256651, -15.14667944815581535 ) ) ;
#1669 = CARTESIAN_POINT ( 'NONE',  ( 118.9227414775786542, 0.4262465694468514643, -12.03445270309931736 ) ) ;
#1670 = CARTESIAN_POINT ( 'NONE',  ( 113.2606921295247702, -9.868328341294093420, -13.39321520033831447 ) ) ;
#1671 = CARTESIAN_POINT ( 'NONE',  ( 115.6220983795247861, -8.402594152722688392, -16.93181055722141792 ) ) ;
#1672 = CARTESIAN_POINT ( 'NONE',  ( 112.8529881442453160, -7.894159318335828068, -9.358103419637847864 ) ) ;
#1673 = CYLINDRICAL_SURFACE ( 'NONE', #5179, 20.00000000000000000 ) ;
#1674 = CARTESIAN_POINT ( 'NONE',  ( 70.92411738817702371, -25.94128094577593657, -5.473262044462485321 ) ) ;
#1675 = CARTESIAN_POINT ( 'NONE',  ( 113.3068014775786594, -1.833838273342658809, -17.42832698103878286 ) ) ;
#1676 = CARTESIAN_POINT ( 'NONE',  ( 118.5256548109119876, -0.4660016031367893996, -10.09054647747474043 ) ) ;
#1677 = ORIENTED_EDGE ( 'NONE', *, *, #32967, .T. ) ;
#1678 = EDGE_CURVE ( 'NONE', #24866, #22218, #24105, .T. ) ;
#1679 = CARTESIAN_POINT ( 'NONE',  ( 120.0005481442453146, -4.153390946401325223, -8.397313243818185668 ) ) ;
#1680 = CARTESIAN_POINT ( 'NONE',  ( 115.3489614775786407, -9.261995988541697145, -16.69588392320189030 ) ) ;
#1681 = CARTESIAN_POINT ( 'NONE',  ( 123.1205148109119563, -1.834011780172310813, -8.268836392978581529 ) ) ;
#1682 = CARTESIAN_POINT ( 'NONE',  ( 119.3765548109119834, -10.15424416112533912, -14.75197769757731336 ) ) ;
#1683 = ORIENTED_EDGE ( 'NONE', *, *, #31150, .F. ) ;
#1684 = EDGE_CURVE ( 'NONE', #41948, #6181, #25963, .T. ) ;
#1685 = CARTESIAN_POINT ( 'NONE',  ( 124.0281414775786146, -7.643976991954077427, -18.09477374809248928 ) ) ;
#1686 = VECTOR ( 'NONE', #20269, 999.9999999999998863 ) ;
#1687 = AXIS2_PLACEMENT_3D ( 'NONE', #22360, #36254, #7999 ) ;
#1688 = CARTESIAN_POINT ( 'NONE',  ( 120.1140014775786398, -1.561330072975668504, -17.79121239304076951 ) ) ;
#1689 = CARTESIAN_POINT ( 'NONE',  ( 125.1375072647497291, -6.121180527655630144, -6.072778184783654609 ) ) ;
#1690 = CARTESIAN_POINT ( 'NONE',  ( 120.0572748109119772, -3.383040157471821630, -19.15922257007629170 ) ) ;
#1691 = CARTESIAN_POINT ( 'NONE',  ( 106.3848327545248651, -2.477300249445798297, -19.15521520033831138 ) ) ;
#1692 = CARTESIAN_POINT ( 'NONE',  ( 120.3685329359119862, -5.367793381288652910, -18.78638297431638904 ) ) ;
#1693 = CARTESIAN_POINT ( 'NONE',  ( 70.19189222814998175, -56.69156685714467159, -35.87943827948784303 ) ) ;
#1694 = CARTESIAN_POINT ( 'NONE',  ( 115.6220983795247861, -8.402594152722688392, -16.93181055722141792 ) ) ;
#1695 = AXIS2_PLACEMENT_3D ( 'NONE', #3814, #41697, #20721 ) ;
#1696 = PLANE ( 'NONE',  #28500 ) ;
#1697 = CARTESIAN_POINT ( 'NONE',  ( 83.82415148905927538, -48.76310523276723785, -24.89321520033831447 ) ) ;
#1698 = CARTESIAN_POINT ( 'NONE',  ( 119.6034614775786196, -3.505236298600246325, -18.68346056562440793 ) ) ;
#1699 = CARTESIAN_POINT ( 'NONE',  ( 124.8223148109119762, 0.9020085738987339008, -11.91225656197089222 ) ) ;
#1700 = CARTESIAN_POINT ( 'NONE',  ( 111.8534302567928478, -9.072100856114243328, -16.09694245754784347 ) ) ;
#1701 = ORIENTED_EDGE ( 'NONE', *, *, #37070, .T. ) ;
#1702 = CARTESIAN_POINT ( 'NONE',  ( 116.1114452545248525, 0.1360012041604422017, -11.32214738847284075 ) ) ;
#1703 = CARTESIAN_POINT ( 'NONE',  ( 111.7327233795247849, -1.325403438956436419, -9.854619843455211026 ) ) ;
#1704 = CARTESIAN_POINT ( 'NONE',  ( 117.1642148109119859, -0.8288870151387760510, -10.36305467784173118 ) ) ;
#1705 = LINE ( 'NONE', #25445, #8559 ) ;
#1706 = CARTESIAN_POINT ( 'NONE',  ( 66.18166293637838749, -0.1100759832042771530, -10.39321520033831625 ) ) ;
#1707 = CARTESIAN_POINT ( 'NONE',  ( -1.923444331009816155, -6.861511549474196947, -18.79244370401574216 ) ) ;
#1709 = CARTESIAN_POINT ( 'NONE',  ( 123.6310548109119765, -5.638512984488999180, -18.83840828888717311 ) ) ;
#1708 = CARTESIAN_POINT ( 'NONE',  ( 65.24959551893836363, -14.08404458135745152, -9.384265616240702101 ) ) ;
#1710 = CARTESIAN_POINT ( 'NONE',  ( 123.5176014775786228, -0.8288870151387760510, -10.36305467784173118 ) ) ;
#1711 = ORIENTED_EDGE ( 'NONE', *, *, #19855, .F. ) ;
#1712 = CARTESIAN_POINT ( 'NONE',  ( 126.1270281442452870, -10.30919188438810075, -12.61870101168855918 ) ) ;
#1713 = CARTESIAN_POINT ( 'NONE',  ( 111.5938171295247940, 0.1403307496149613920, -13.39321520033831447 ) ) ;
#1714 = CARTESIAN_POINT ( 'NONE',  ( 124.3117748109119844, 0.1319031606808879209, -14.10382304977623669 ) ) ;
#1715 = EDGE_CURVE ( 'NONE', #25696, #41400, #24357, .T. ) ;
#1716 = CARTESIAN_POINT ( 'NONE',  ( 121.4754414775786131, -1.833838273342659697, -17.42832698103878286 ) ) ;
#1717 = CARTESIAN_POINT ( 'NONE',  ( 114.7249681442453237, -9.565557343593413364, -10.61323700422348004 ) ) ;
#1718 = CARTESIAN_POINT ( 'NONE',  ( 85.72471707980444933, -15.28778963902104060, -16.89321520033831447 ) ) ;
#1719 = CARTESIAN_POINT ( 'NONE',  ( 108.1211608795247798, -8.938348069036489818, -9.318865927141430916 ) ) ;
#1720 = CONICAL_SURFACE ( 'NONE', #33641, 2.999999999999999556, 0.9599310885968830309 ) ;
#1721 = LINE ( 'NONE', #29548, #15713 ) ;
#1722 = DIRECTION ( 'NONE',  ( 0.9498278979187094739, 0.3127730236694427068, -0.000000000000000000 ) ) ;
#1723 = CARTESIAN_POINT ( 'NONE',  ( 63.69189222814998175, -50.16718729050181480, 3.106784799661685526 ) ) ;
#1724 = CARTESIAN_POINT ( 'NONE',  ( 109.9963952545248134, 0.8980012041604421569, -11.00651665394454071 ) ) ;
#1725 = DIRECTION ( 'NONE',  ( 0.000000000000000000, 0.3713878862591642460, -0.9284778069183722282 ) ) ;
#1726 = CARTESIAN_POINT ( 'NONE',  ( 83.87098973808613778, -31.73904887874523340, -22.52550971913698419 ) ) ;
#1727 = CARTESIAN_POINT ( 'NONE',  ( 120.7947214775786193, -9.261995988541697145, -16.69588392320189030 ) ) ;
#1728 = CARTESIAN_POINT ( 'NONE',  ( 117.6747548109119919, -1.834011780172310813, -8.268836392978581529 ) ) ;
#1729 = CARTESIAN_POINT ( 'NONE',  ( 108.1211608795247798, -8.938348069036489818, -9.318865927141430916 ) ) ;
#1730 = CARTESIAN_POINT ( 'NONE',  ( 117.7314814775786260, -4.089484607189486809, -7.948022111789456723 ) ) ;
#1731 = CARTESIAN_POINT ( 'NONE',  ( 124.4356136130535333, -8.422568683347400054, -17.41241596312869788 ) ) ;
#1732 = ORIENTED_EDGE ( 'NONE', *, *, #30164, .F. ) ;
#1733 = DIRECTION ( 'NONE',  ( 0.000000000000000000, -0.3818493186865936084, 0.9242245927363024194 ) ) ;
#1734 = CONICAL_SURFACE ( 'NONE', #37413, 2.445500000000004448, 0.9599310885968757034 ) ;
#1735 = CARTESIAN_POINT ( 'NONE',  ( 121.3619881442452879, -4.089484607189486809, -7.948022111789456723 ) ) ;
#1736 = CARTESIAN_POINT ( 'NONE',  ( 120.7947214775786193, -9.261995988541697145, -16.69588392320189030 ) ) ;
#1737 = EDGE_CURVE ( 'NONE', #35629, #35146, #2039, .T. ) ;
#1738 = CARTESIAN_POINT ( 'NONE',  ( 124.4819548109119722, -2.084020599724406786, -8.691656652584148546 ) ) ;
#1739 = DIRECTION ( 'NONE',  ( 1.000000000000000000, 0.000000000000000000, 0.000000000000000000 ) ) ;
#1740 = CARTESIAN_POINT ( 'NONE',  ( 112.8529881442453160, -7.894159318335828068, -9.358103419637847864 ) ) ;
#1741 = CARTESIAN_POINT ( 'NONE',  ( 112.1155414775786454, -10.15424416112533912, -14.75197769757731336 ) ) ;
#1742 = CARTESIAN_POINT ( 'NONE',  ( 107.2182702545248105, -10.62599879583958717, -15.77991374673208469 ) ) ;
#1743 = CARTESIAN_POINT ( 'NONE',  ( 120.6812681442452941, 0.1319031606808879209, -14.10382304977623669 ) ) ;
#1744 = CARTESIAN_POINT ( 'NONE',  ( 83.46705746533213244, -32.83968548964498524, -23.89321520033831803 ) ) ;
#1745 = CARTESIAN_POINT ( 'NONE',  ( 85.04324155394569118, -25.99489077589524300, -13.39321520033831447 ) ) ;
#1746 = ORIENTED_EDGE ( 'NONE', *, *, #39630, .T. ) ;
#1747 = CLOSED_SHELL ( 'NONE', ( #4152, #37866, #40832, #17245, #16199, #21143, #36527, #26583, #23655, #20308, #38149, #18533, #35581, #9060, #4115, #13887, #44627, #15699, #28669, #35867, #21510, #34238, #35882, #34304, #5814, #38233, #42050, #33081, #39264, #10525, #29766, #20277, #13735, #40925, #19555, #43598, #6488, #4374, #15680, #7071, #24586, #1064, #38417, #19728, #39940, #41099, #4945, #44561, #38547, #4966, #20625, #26823, #10638, #12784, #14728, #37236, #36466, #14740, #3572, #33654, #43377, #17043, #18627, #23403, #28076, #37922, #4151, #25624, #14144, #30621, #36573, #2068, #37329, #6478, #6539, #28402, #39232, #44240, #532, #16742, #12305, #32549, #31783, #4091, #35680 ) ) ;
#1748 = PLANE ( 'NONE',  #11154 ) ;
#1749 = CARTESIAN_POINT ( 'NONE',  ( 123.8579614775786126, 0.5811942927096110934, -14.16772938898807510 ) ) ;
#1750 = CARTESIAN_POINT ( 'NONE',  ( 73.07463722459043254, -54.57507799681722105, -34.13834222174655508 ) ) ;
#1751 = PRESENTATION_STYLE_ASSIGNMENT (( #8608 ) ) ;
#1752 = CARTESIAN_POINT ( 'NONE',  ( 118.5256548109119876, -8.899110576539710493, -16.42337572283490132 ) ) ;
#1753 = CARTESIAN_POINT ( 'NONE',  ( 83.86216108596053687, -30.76310523276723785, -22.89321520033831803 ) ) ;
#1754 = CARTESIAN_POINT ( 'NONE',  ( 124.5165996254432201, -9.747892374099686563, -12.32126250935987954 ) ) ;
#1755 = CARTESIAN_POINT ( 'NONE',  ( 125.2194014775786286, 0.1319031606808879209, -14.10382304977623669 ) ) ;
#1756 = LINE ( 'NONE', #19547, #36017 ) ;
#1757 = CARTESIAN_POINT ( 'NONE',  ( 124.0848681442452772, -5.574606645277164318, -18.38911715685844683 ) ) ;
#1758 = CARTESIAN_POINT ( 'NONE',  ( 125.2824180292811604, -11.90974677766837075, -14.90133849250740816 ) ) ;
#1759 = CARTESIAN_POINT ( 'NONE',  ( 121.4754414775786131, -8.166667518702819706, -8.995218007635861213 ) ) ;
#1760 = CARTESIAN_POINT ( 'NONE',  ( 116.2565881442453133, -0.8288870151387760510, -10.36305467784173118 ) ) ;
#1761 = CARTESIAN_POINT ( 'NONE',  ( 121.7590748109119687, -2.084020599724406786, -8.691656652584148546 ) ) ;
#1762 = VERTEX_POINT ( 'NONE', #27971 ) ;
#1763 = CARTESIAN_POINT ( 'NONE',  ( 124.2550481442452792, -9.988377603198980381, -10.36322818467138518 ) ) ;
#1764 = CARTESIAN_POINT ( 'NONE',  ( 117.4478481442453131, 0.2603800115204892296, -16.42320221600525088 ) ) ;
#1765 = CARTESIAN_POINT ( 'NONE',  ( 113.7468640045248236, 0.1403307496149616695, -15.46607636864997204 ) ) ;
#1766 = CARTESIAN_POINT ( 'NONE',  ( 113.6471614775786492, -4.153390946401321671, -8.397313243818183892 ) ) ;
#1767 = CARTESIAN_POINT ( 'NONE',  ( 124.2550481442452792, -0.1624402480850797581, -16.17319339645315424 ) ) ;
#1768 = CARTESIAN_POINT ( 'NONE',  ( 120.2274548109119934, 0.5811942927096110934, -14.16772938898807510 ) ) ;
#1769 = CARTESIAN_POINT ( 'NONE',  ( 106.3153796295248412, -4.863998795839590272, -8.388885654883775800 ) ) ;
#1770 = CARTESIAN_POINT ( 'NONE',  ( 111.3854577545248645, -2.791137627527939813, -18.39754474579286025 ) ) ;
#1771 = DIRECTION ( 'NONE',  ( 1.000000000000000000, 0.000000000000000000, -0.000000000000000000 ) ) ;
#1772 = AXIS2_PLACEMENT_3D ( 'NONE', #30439, #24060, #27478 ) ;
#1773 = CARTESIAN_POINT ( 'NONE',  ( 114.7816948109119863, -9.859900752359374465, -12.68260735090039404 ) ) ;
#1774 = CARTESIAN_POINT ( 'NONE',  ( 120.5074391859119913, -8.844754642576884152, -8.592115655440052180 ) ) ;
#1775 = CARTESIAN_POINT ( 'NONE',  ( 125.3895814775786448, -7.893985811506177619, -18.51759400769804742 ) ) ;
#1776 = EDGE_LOOP ( 'NONE', ( #20608, #11474, #27163, #35151 ) ) ;
#1777 = CARTESIAN_POINT ( 'NONE',  ( 125.2194014775786286, 0.1319031606808879209, -14.10382304977623669 ) ) ;
#1778 = CARTESIAN_POINT ( 'NONE',  ( 123.4244704359119709, 1.345710702986147034, -13.97328579221134426 ) ) ;
#1779 = CARTESIAN_POINT ( 'NONE',  ( 121.2714235609119697, 0.6414057260225851653, -11.69287257290600657 ) ) ;
#1780 = DIRECTION ( 'NONE',  ( -0.2768435750659241079, -0.3568721902840695792, 0.8921882507333129819 ) ) ;
#1781 = AXIS2_PLACEMENT_3D ( 'NONE', #24597, #16874, #38481 ) ;
#1782 = CARTESIAN_POINT ( 'NONE',  ( 109.1629577545248395, -2.791137627527939813, -18.39754474579286025 ) ) ;
#1783 = VERTEX_POINT ( 'NONE', #41440 ) ;
#1784 = CARTESIAN_POINT ( 'NONE',  ( 113.9307948109119906, 0.9020085738987339008, -11.91225656197089222 ) ) ;
#1785 = CARTESIAN_POINT ( 'NONE',  ( 113.1933481442453058, -4.089484607189490362, -7.948022111789460276 ) ) ;
#1786 = CARTESIAN_POINT ( 'NONE',  ( 124.8790414775786246, -8.899110576539710493, -16.42337572283490132 ) ) ;
#1787 = CARTESIAN_POINT ( 'NONE',  ( 116.0864081442453113, -0.1624402480850797581, -16.17319339645315424 ) ) ;
#1788 =( NAMED_UNIT ( * ) PLANE_ANGLE_UNIT ( ) SI_UNIT ( $, .RADIAN. ) );
#1789 = DIRECTION ( 'NONE',  ( 0.000000000000000000, 0.000000000000000000, 1.000000000000000000 ) ) ;
#1790 = CARTESIAN_POINT ( 'NONE',  ( 82.31000308962319423, -13.76004065658516673, -8.143215200338314474 ) ) ;
#1791 = CARTESIAN_POINT ( 'NONE',  ( 115.4624148109119943, -5.638512984488999180, -18.83840828888717311 ) ) ;
#1792 = CARTESIAN_POINT ( 'NONE',  ( 111.7327233795247849, -1.325403438956436419, -9.854619843455211026 ) ) ;
#1793 = CARTESIAN_POINT ( 'NONE',  ( 125.3328548109119964, -9.261995988541697145, -16.69588392320189030 ) ) ;
#1794 = CARTESIAN_POINT ( 'NONE',  ( 89.29245855188943892, -9.882163754870950001, -18.64321520033831803 ) ) ;
#1795 = VERTEX_POINT ( 'NONE', #41877 ) ;
#1796 = CARTESIAN_POINT ( 'NONE',  ( 113.7038881442453402, -3.383040157471821630, -19.15922257007629170 ) ) ;
#1797 = CARTESIAN_POINT ( 'NONE',  ( 111.2646414775786496, -8.899110576539710493, -16.42337572283490132 ) ) ;
#1798 = FACE_BOUND ( 'NONE', #15754, .T. ) ;
#1799 = CARTESIAN_POINT ( 'NONE',  ( 112.9664414775786412, 0.5811942927096154232, -14.16772938898807155 ) ) ;
#1800 = CIRCLE ( 'NONE', #6933, 4.999999999999998224 ) ;
#1801 = VERTEX_POINT ( 'NONE', #20460 ) ;
#1802 = CARTESIAN_POINT ( 'NONE',  ( 118.3554748109119998, 0.2603800115204892296, -16.42320221600525088 ) ) ;
#1803 = CARTESIAN_POINT ( 'NONE',  ( 93.93057702947278642, -25.99489077589524300, -13.39321520033831447 ) ) ;
#1804 = CARTESIAN_POINT ( 'NONE',  ( 89.01247232317646763, -25.99489077589524300, -13.39321520033831447 ) ) ;
#1805 = CARTESIAN_POINT ( 'NONE',  ( 126.2184548109119788, -4.863998795839242995, -13.39321520033831447 ) ) ;
#1806 = CARTESIAN_POINT ( 'NONE',  ( 123.6001203708216423, -4.367669542124009929, -15.30311642213100143 ) ) ;
#1807 = AXIS2_PLACEMENT_3D ( 'NONE', #35738, #10915, #29133 ) ;
#1808 = CARTESIAN_POINT ( 'NONE',  ( 113.0798948109119948, -8.899110576539710493, -16.42337572283490132 ) ) ;
#1809 = LINE ( 'NONE', #19599, #44500 ) ;
#1810 = CARTESIAN_POINT ( 'NONE',  ( 121.3587993874819944, -6.063848558940142297, -18.38516058545102183 ) ) ;
#1811 = CARTESIAN_POINT ( 'NONE',  ( 112.0020881442453344, -9.565557343593413364, -10.61323700422348004 ) ) ;
#1812 = CARTESIAN_POINT ( 'NONE',  ( 112.8529881442453302, -1.561330072975668060, -17.79121239304076596 ) ) ;
#1813 = CARTESIAN_POINT ( 'NONE',  ( 116.6540404065295178, -9.155876812127887732, -16.09229352560785031 ) ) ;
#1814 = CARTESIAN_POINT ( 'NONE',  ( 122.4397948109119767, -0.1624402480850797581, -16.17319339645315424 ) ) ;
#1815 = DIRECTION ( 'NONE',  ( -0.5735764363510446051, 0.3127926500124816878, -0.7570804645221042017 ) ) ;
#1816 = CARTESIAN_POINT ( 'NONE',  ( 124.2550481442452792, -9.988377603198980381, -10.36322818467138518 ) ) ;
#1817 = CARTESIAN_POINT ( 'NONE',  ( 122.4397948109119767, -9.988377603198976828, -10.36322818467138340 ) ) ;
#1818 = ORIENTED_EDGE ( 'NONE', *, *, #22126, .F. ) ;
#1819 = CARTESIAN_POINT ( 'NONE',  ( 114.4583197905468808, 0.6938714319018670640, -12.14321520033833579 ) ) ;
#1820 = CARTESIAN_POINT ( 'NONE',  ( 109.9963952545248134, 0.8980012041604421569, -11.00651665394454071 ) ) ;
#1821 = CARTESIAN_POINT ( 'NONE',  ( 111.0381921295247878, -9.868328341294093420, -13.39321520033831447 ) ) ;
#1822 = CARTESIAN_POINT ( 'NONE',  ( 110.7603796295247918, -4.863998795839590272, -8.388885654883775800 ) ) ;
#1823 = CARTESIAN_POINT ( 'NONE',  ( 125.4924948109119924, -4.159894987976798575, -8.443039665293765594 ) ) ;
#1824 = CARTESIAN_POINT ( 'NONE',  ( 114.4413348109119823, -9.261995988541697145, -16.69588392320189030 ) ) ;
#1825 = ORIENTED_EDGE ( 'NONE', *, *, #24490, .T. ) ;
#1826 = CARTESIAN_POINT ( 'NONE',  ( 123.7717360609119623, -3.387241619883791355, -18.17469012370385073 ) ) ;
#1827 = CYLINDRICAL_SURFACE ( 'NONE', #3016, 1.999999999999998890 ) ;
#1828 = CARTESIAN_POINT ( 'NONE',  ( 115.6893214775786447, -9.859900752359374465, -12.68260735090039404 ) ) ;
#1829 = CARTESIAN_POINT ( 'NONE',  ( 122.8176765460471813, -2.191907684172563986, -18.20049396185734025 ) ) ;
#1830 = CARTESIAN_POINT ( 'NONE',  ( 119.7736414775786358, -10.30919188438810075, -12.61870101168855918 ) ) ;
#1831 = CARTESIAN_POINT ( 'NONE',  ( 108.7462390045248242, 0.8980012041604421569, -15.77991374673208469 ) ) ;
#1832 = CARTESIAN_POINT ( 'NONE',  ( 70.19189222814998175, -53.33815113939435548, -34.53808368179734600 ) ) ;
#1833 = VECTOR ( 'NONE', #22228, 1000.000000000000000 ) ;
#1834 = ORIENTED_EDGE ( 'NONE', *, *, #21963, .F. ) ;
#1835 = CARTESIAN_POINT ( 'NONE',  ( 86.34560043013698305, -9.320000780048239619, -16.89321520033831447 ) ) ;
#1836 = CARTESIAN_POINT ( 'NONE',  ( 117.7882081442453170, -3.505236298600246325, -18.68346056562440793 ) ) ;
#1837 = CARTESIAN_POINT ( 'NONE',  ( 116.2565881442452991, -9.261995988541697145, -16.69588392320189030 ) ) ;
#1838 = CARTESIAN_POINT ( 'NONE',  ( 115.5191414775786569, -3.383040157471821630, -19.15922257007629170 ) ) ;
#1839 = CARTESIAN_POINT ( 'NONE',  ( 118.2788031242421596, -1.016270020561755860, -17.26805140881366896 ) ) ;
#1840 = CARTESIAN_POINT ( 'NONE',  ( 123.0070614775786169, -10.15424416112533912, -14.75197769757731336 ) ) ;
#1841 = CARTESIAN_POINT ( 'NONE',  ( 117.8449348109119938, -1.833838273342659253, -17.42832698103878286 ) ) ;
#1842 = ORIENTED_EDGE ( 'NONE', *, *, #22274, .T. ) ;
#1843 = AXIS2_PLACEMENT_3D ( 'NONE', #8029, #11011, #28565 ) ;
#1844 = CARTESIAN_POINT ( 'NONE',  ( 121.8270485609119760, -10.36940331770106916, -15.09355782777062061 ) ) ;
#1845 = CARTESIAN_POINT ( 'NONE',  ( 114.2711548109119803, -9.988377603198976828, -10.36322818467138340 ) ) ;
#1846 = CARTESIAN_POINT ( 'NONE',  ( 116.3700414775786527, -4.153390946401321671, -8.397313243818183892 ) ) ;
#1847 = ORIENTED_EDGE ( 'NONE', *, *, #42590, .F. ) ;
#1848 = DIRECTION ( 'NONE',  ( 0.000000000000000000, -0.9242245927363027524, -0.3818493186865928868 ) ) ;
#1849 = CARTESIAN_POINT ( 'NONE',  ( 114.8384214775786489, 0.9020085738987339008, -11.91225656197089222 ) ) ;
#1850 = ADVANCED_FACE ( 'NONE', ( #27747 ), #30965, .T. ) ;
#1851 = CARTESIAN_POINT ( 'NONE',  ( 115.2053796295247849, -4.863998795839590272, -19.15521520033831493 ) ) ;
#1852 = CARTESIAN_POINT ( 'NONE',  ( 117.3343948109119737, -6.222761293078241884, -8.102969835052219238 ) ) ;
#1853 = ORIENTED_EDGE ( 'NONE', *, *, #33091, .F. ) ;
#1854 = ORIENTED_EDGE ( 'NONE', *, *, #10017, .T. ) ;
#1855 = CARTESIAN_POINT ( 'NONE',  ( 123.3474214775786209, -0.1624402480850797581, -16.17319339645315424 ) ) ;
#1856 = CARTESIAN_POINT ( 'NONE',  ( 120.7947214775786193, -0.8288870151387760510, -10.36305467784173118 ) ) ;
#1857 = PLANE ( 'NONE',  #19264 ) ;
#1858 = DIRECTION ( 'NONE',  ( -0.000000000000000000, -0.9284778069183721172, -0.3713878862591650232 ) ) ;
#1859 = CARTESIAN_POINT ( 'NONE',  ( 61.74332929926398350, -66.01496853250924346, -43.25593076250496694 ) ) ;
#1860 = CIRCLE ( 'NONE', #27379, 2.541999999999999371 ) ;
#1861 = DIRECTION ( 'NONE',  ( 0.9609149988134837450, -0.1028163501681639419, 0.2570431154366518145 ) ) ;
#1862 = CARTESIAN_POINT ( 'NONE',  ( 117.0507614775786465, -10.30919188438810075, -12.61870101168855918 ) ) ;
#1863 = ADVANCED_FACE ( 'NONE', ( #17044 ), #6316, .T. ) ;
#1865 = CARTESIAN_POINT ( 'NONE',  ( 117.5613014775786525, -10.15424416112533912, -14.75197769757731336 ) ) ;
#1864 = CARTESIAN_POINT ( 'NONE',  ( 115.4056881442453459, -7.893985811506177619, -18.51759400769804742 ) ) ;
#1866 = CARTESIAN_POINT ( 'NONE',  ( 121.6456214775786293, 0.4262465694468514643, -12.03445270309931736 ) ) ;
#1867 = CARTESIAN_POINT ( 'NONE',  ( 112.2237824678160933, -1.149058757900094818, -17.09122335155389294 ) ) ;
#1868 = EDGE_CURVE ( 'NONE', #4322, #970, #41663, .T. ) ;
#1869 = EDGE_CURVE ( 'NONE', #30875, #2648, #15615, .T. ) ;
#1870 = ORIENTED_EDGE ( 'NONE', *, *, #31960, .F. ) ;
#1871 = CARTESIAN_POINT ( 'NONE',  ( 118.1285681442453068, -2.084020599724406786, -8.691656652584148546 ) ) ;
#1872 = DIRECTION ( 'NONE',  ( 0.000000000000000000, 0.8069730661766899571, -0.5905882410490339574 ) ) ;
#1873 = CARTESIAN_POINT ( 'NONE',  ( 110.6909265045248247, -7.250697342233347165, -19.15521520033831138 ) ) ;
#1874 = DIRECTION ( 'NONE',  ( 0.000000000000000000, -0.3818493186865936084, 0.9242245927363024194 ) ) ;
#1875 = CARTESIAN_POINT ( 'NONE',  ( 110.8298327545248299, -2.477300249445798297, -19.15521520033831138 ) ) ;
#1876 = VECTOR ( 'NONE', #43079, 1000.000000000000000 ) ;
#1877 = CARTESIAN_POINT ( 'NONE',  ( 119.3198281442452924, 0.5811942927096110934, -14.16772938898807510 ) ) ;
#1878 = ORIENTED_EDGE ( 'NONE', *, *, #1567, .F. ) ;
#1879 = CARTESIAN_POINT ( 'NONE',  ( 122.6099748109119929, -9.261995988541697145, -16.69588392320189030 ) ) ;
#1880 = DIRECTION ( 'NONE',  ( 1.000000000000000000, 0.000000000000000000, -0.000000000000000000 ) ) ;
#1881 = CARTESIAN_POINT ( 'NONE',  ( 106.1070202545248407, -10.62599879583958717, -15.77991374673208469 ) ) ;
#1882 = CARTESIAN_POINT ( 'NONE',  ( 119.8303681442453126, -10.63000616557722466, -14.87417383870573495 ) ) ;
#1883 = CARTESIAN_POINT ( 'NONE',  ( 116.6536748109119941, 0.9020085738987339008, -11.91225656197089222 ) ) ;
#1884 = CARTESIAN_POINT ( 'NONE',  ( 62.60955873541980310, -3.465946903308488647, -19.20240821814916288 ) ) ;
#1885 = CARTESIAN_POINT ( 'NONE',  ( -6.962123463324031647, -11.49046785505262136, -19.39321520033831447 ) ) ;
#1886 = ORIENTED_EDGE ( 'NONE', *, *, #7632, .F. ) ;
#1887 = DIRECTION ( 'NONE',  ( -1.000000000000000000, 0.000000000000000000, 0.000000000000000000 ) ) ;
#1888 = CARTESIAN_POINT ( 'NONE',  ( 109.2294421359564467, -10.14375206540927365, -14.94852355942958155 ) ) ;
#1889 = CARTESIAN_POINT ( 'NONE',  ( 121.3052614775786111, -7.643976991954077427, -18.09477374809248928 ) ) ;
#1890 = AXIS2_PLACEMENT_3D ( 'NONE', #13306, #3694, #31285 ) ;
#1891 = CARTESIAN_POINT ( 'NONE',  ( 114.3024890045248156, -9.868328341294098749, -11.32035403202665869 ) ) ;
#1892 = CARTESIAN_POINT ( 'NONE',  ( 112.4272546295247821, -4.863998795839590272, -18.39754474579285315 ) ) ;
#1893 = CARTESIAN_POINT ( 'NONE',  ( 116.7104014775786425, -8.899110576539710493, -16.42337572283490132 ) ) ;
#1894 = DIRECTION ( 'NONE',  ( 0.000000000000000000, 0.000000000000000000, -1.000000000000000000 ) ) ;
#1895 = CARTESIAN_POINT ( 'NONE',  ( 69.79878637322866552, -26.09957013199193554, -5.786566508650874852 ) ) ;
#1896 = CARTESIAN_POINT ( 'NONE',  ( 126.0703014775786102, -9.988377603198980381, -10.36322818467138518 ) ) ;
#1897 = CARTESIAN_POINT ( 'NONE',  ( 124.2550481442452792, -9.988377603198980381, -10.36322818467138518 ) ) ;
#1898 = ORIENTED_EDGE ( 'NONE', *, *, #39518, .F. ) ;
#1899 = ADVANCED_FACE ( 'NONE', ( #34121 ), #28031, .T. ) ;
#1900 = CARTESIAN_POINT ( 'NONE',  ( 120.3976348109119812, -7.643976991954077427, -18.09477374809248928 ) ) ;
#1901 = CARTESIAN_POINT ( 'NONE',  ( 114.3846081442453197, -10.63000616557722466, -14.87417383870573495 ) ) ;
#1902 = CARTESIAN_POINT ( 'NONE',  ( 121.0216281442452981, -1.561330072975668948, -17.79121239304076951 ) ) ;
#1903 = CARTESIAN_POINT ( 'NONE',  ( 123.1772414775786189, -5.574606645277164318, -18.38911715685844683 ) ) ;
#1904 = ORIENTED_EDGE ( 'NONE', *, *, #32554, .T. ) ;
#1905 = CARTESIAN_POINT ( 'NONE',  ( 123.3474214775786209, -0.1624402480850797581, -16.17319339645315424 ) ) ;
#1906 = ADVANCED_FACE ( 'NONE', ( #2890, #17472 ), #31369, .T. ) ;
#1907 = AXIS2_PLACEMENT_3D ( 'NONE', #5450, #8440, #15500 ) ;
#1908 = ADVANCED_FACE ( 'NONE', ( #17919 ), #25142, .T. ) ;
#1909 = CARTESIAN_POINT ( 'NONE',  ( 123.9146881442452894, 0.9020085738987339008, -11.91225656197089222 ) ) ;
#1910 = CARTESIAN_POINT ( 'NONE',  ( 112.5126281442453120, 0.1319031606808879209, -14.10382304977623669 ) ) ;
#1911 = CARTESIAN_POINT ( 'NONE',  ( 125.9001214775786224, -4.089484607189486809, -7.948022111789456723 ) ) ;
#1912 =( BOUNDED_CURVE ( )  B_SPLINE_CURVE ( 3, ( #16184, #40122, #36238, #36461 ),
 .UNSPECIFIED., .F., .F. ) 
 B_SPLINE_CURVE_WITH_KNOTS ( ( 4, 4 ),
 ( 4.664242276651448194, 4.712388980384689674 ),
 .UNSPECIFIED. ) 
 CURVE ( )  GEOMETRIC_REPRESENTATION_ITEM ( )  RATIONAL_B_SPLINE_CURVE ( ( 1.000000000000000000, 0.9998068339056410680, 0.9998068339056410680, 1.000000000000000000 ) ) 
 REPRESENTATION_ITEM ( '' )  );
#1913 = CARTESIAN_POINT ( 'NONE',  ( 106.4542858795248179, -0.7896495226426338832, -17.46756447353520159 ) ) ;
#1914 = CARTESIAN_POINT ( 'NONE',  ( 110.2184548109119788, -4.863998795839242995, -13.39321520033831447 ) ) ;
#1915 = CARTESIAN_POINT ( 'NONE',  ( 138.0698945632798882, -1.891928339825783345, -16.10198143539211202 ) ) ;
#1916 = CARTESIAN_POINT ( 'NONE',  ( 108.8851452545248151, -9.868328341294098749, -15.46607636864997204 ) ) ;
#1917 = AXIS2_PLACEMENT_3D ( 'NONE', #9833, #40844, #41736 ) ;
#1918 = CARTESIAN_POINT ( 'NONE',  ( 122.7993923109119692, -0.4387604401700512802, -15.73000352943951619 ) ) ;
#1919 = EDGE_CURVE ( 'NONE', #33992, #25917, #8371, .T. ) ;
#1920 = CARTESIAN_POINT ( 'NONE',  ( 137.3019930433563331, -10.07954145175000349, -13.43736401499259614 ) ) ;
#1921 = CARTESIAN_POINT ( 'NONE',  ( 117.8449348109119938, -1.833838273342659253, -17.42832698103878286 ) ) ;
#1922 = CARTESIAN_POINT ( 'NONE',  ( 126.1837548109119211, -10.63000616557722466, -14.87417383870573495 ) ) ;
#1923 = CARTESIAN_POINT ( 'NONE',  ( 121.9470836909669913, -22.29799240495002977, -11.86581792559194426 ) ) ;
#1924 = EDGE_CURVE ( 'NONE', #12824, #19575, #42844, .T. ) ;
#1925 = EDGE_CURVE ( 'NONE', #40221, #22169, #36765, .T. ) ;
#1926 = ORIENTED_EDGE ( 'NONE', *, *, #2248, .F. ) ;
#1927 = CARTESIAN_POINT ( 'NONE',  ( 116.6670702545247593, -9.863998795839588496, -15.46428301220378998 ) ) ;
#1928 = CARTESIAN_POINT ( 'NONE',  ( 108.3989733795247759, -1.325403438956436419, -9.854619843455211026 ) ) ;
#1929 = CARTESIAN_POINT ( 'NONE',  ( 116.4267681442453153, -6.222761293078241884, -8.102969835052219238 ) ) ;
#1930 = CARTESIAN_POINT ( 'NONE',  ( 113.2858169107182249, -2.467220198592768199, -17.83387418641523325 ) ) ;
#1931 = AXIS2_PLACEMENT_3D ( 'NONE', #40032, #8352, #15192 ) ;
#1932 = CARTESIAN_POINT ( 'NONE',  ( 90.06246830635160450, -25.99489077589524300, -13.39321520033831625 ) ) ;
#1933 = CARTESIAN_POINT ( 'NONE',  ( 124.2193060444391790, -1.267766418764731728, -16.93314635290706605 ) ) ;
#1935 = CARTESIAN_POINT ( 'NONE',  ( 122.4397948109119767, -9.988377603198976828, -10.36322818467138340 ) ) ;
#1934 = CARTESIAN_POINT ( 'NONE',  ( 69.87572422742091760, -11.86958442233774313, -21.39321520033831447 ) ) ;
#1936 = CARTESIAN_POINT ( 'NONE',  ( 121.0216281442452981, -7.894159318335828068, -9.358103419637847864 ) ) ;
#1937 = ORIENTED_EDGE ( 'NONE', *, *, #35623, .T. ) ;
#1938 = CARTESIAN_POINT ( 'NONE',  ( 61.69084222814998242, -0.02276961308034231024, -12.14321520033831625 ) ) ;
#1939 = CARTESIAN_POINT ( 'NONE',  ( 126.2471382750665043, 0.06775931372756542614, -14.29995113275557372 ) ) ;
#1940 = CARTESIAN_POINT ( 'NONE',  ( 111.8021765045248372, -2.791137627527939813, -8.388885654883777576 ) ) ;
#1941 = CARTESIAN_POINT ( 'NONE',  ( 121.3052614775786111, -7.643976991954077427, -18.09477374809248928 ) ) ;
#1942 = CIRCLE ( 'NONE', #7033, 2.999999999999999556 ) ;
#1943 = CARTESIAN_POINT ( 'NONE',  ( 121.0216281442452981, -7.894159318335828068, -9.358103419637847864 ) ) ;
#1944 = CARTESIAN_POINT ( 'NONE',  ( 125.1589444732352234, 1.195138823160687869, -17.64039077345892181 ) ) ;
#1945 = CARTESIAN_POINT ( 'NONE',  ( 106.5931921295248372, 0.8980012041604618078, -13.39321520033831447 ) ) ;
#1946 = DIRECTION ( 'NONE',  ( -0.000000000000000000, -0.9284778069183721172, -0.3713878862591650232 ) ) ;
#1947 = DIRECTION ( 'NONE',  ( 0.6725995567522981000, 0.7400066460894877407, -0.000000000000000000 ) ) ;
#1948 = LINE ( 'NONE', #39813, #37916 ) ;
#1949 = CARTESIAN_POINT ( 'NONE',  ( 111.8716296295247901, -4.863998795839590272, -19.15521520033831493 ) ) ;
#1950 = CARTESIAN_POINT ( 'NONE',  ( -13.78505786413266243, -3.796669003528118758, -18.12937505555870388 ) ) ;
#1951 = CARTESIAN_POINT ( 'NONE',  ( 116.3860827545247787, -2.477300249445798297, -19.15521520033831138 ) ) ;
#1952 = CARTESIAN_POINT ( 'NONE',  ( 120.1140014775786398, -1.561330072975668504, -17.79121239304076951 ) ) ;
#1953 = CARTESIAN_POINT ( 'NONE',  ( 121.0783548109119749, 0.2603800115204892296, -16.42320221600525088 ) ) ;
#1954 = LINE ( 'NONE', #12463, #15351 ) ;
#1955 = CARTESIAN_POINT ( 'NONE',  ( 115.8595014775786609, -1.834011780172310813, -8.268836392978581529 ) ) ;
#1956 = LINE ( 'NONE', #39601, #14096 ) ;
#1957 = ORIENTED_EDGE ( 'NONE', *, *, #33681, .T. ) ;
#1958 = CARTESIAN_POINT ( 'NONE',  ( 72.75524511225664526, -25.99489077589583630, -8.393215200338314474 ) ) ;
#1959 = CARTESIAN_POINT ( 'NONE',  ( 122.9503348109119827, 0.5811942927096110934, -14.16772938898807510 ) ) ;
#1960 = CARTESIAN_POINT ( 'NONE',  ( 119.4332814775786318, -0.4660016031367893996, -10.09054647747474043 ) ) ;
#1961 = CARTESIAN_POINT ( 'NONE',  ( 124.9924948109119924, -5.574606645277164318, -18.38911715685844683 ) ) ;
#1962 = AXIS2_PLACEMENT_3D ( 'NONE', #35730, #25036, #28690 ) ;
#1963 = SHAPE_DEFINITION_REPRESENTATION ( #18316, #850 ) ;
#1964 = CYLINDRICAL_SURFACE ( 'NONE', #9953, 4.999999999999997335 ) ;
#1965 = CARTESIAN_POINT ( 'NONE',  ( 113.1366214775786432, -7.643976991954077427, -18.09477374809248928 ) ) ;
#1966 = CARTESIAN_POINT ( 'NONE',  ( 124.2550481442452792, -9.988377603198980381, -10.36322818467138518 ) ) ;
#1967 = VECTOR ( 'NONE', #8831, 1000.000000000000000 ) ;
#1968 = CARTESIAN_POINT ( 'NONE',  ( 107.3571765045248299, -7.250697342233347165, -19.15521520033831138 ) ) ;
#1969 = CARTESIAN_POINT ( 'NONE',  ( 119.0929214775786278, -4.153390946401325223, -8.397313243818185668 ) ) ;
#1970 = CARTESIAN_POINT ( 'NONE',  ( 110.9481121053769073, 0.3967854368539851517, -16.28112951403850062 ) ) ;
#1971 = CARTESIAN_POINT ( 'NONE',  ( 119.7434548109119703, -4.863998795839242995, -13.39321520033831447 ) ) ;
#1972 = VERTEX_POINT ( 'NONE', #3772 ) ;
#1973 = EDGE_CURVE ( 'NONE', #45054, #24842, #32375, .T. ) ;
#1974 = CIRCLE ( 'NONE', #23849, 2.999999999999999556 ) ;
#1975 = CARTESIAN_POINT ( 'NONE',  ( 121.4103298109119748, -7.200787124940443817, -17.81845355600750835 ) ) ;
#1976 = CARTESIAN_POINT ( 'NONE',  ( 122.8936081442453059, 0.2603800115204892296, -16.42320221600525088 ) ) ;
#1977 = CARTESIAN_POINT ( 'NONE',  ( 114.6874464091100947, -0.9924539043446216624, -17.29976612834909133 ) ) ;
#1978 = CARTESIAN_POINT ( 'NONE',  ( 62.64330450333520162, -3.453051920597017155, -7.590354665846188453 ) ) ;
#1979 = CARTESIAN_POINT ( 'NONE',  ( 109.2294421295247844, 0.8460904216231607267, -12.14321520033831625 ) ) ;
#1980 = CARTESIAN_POINT ( 'NONE',  ( 119.0929214775786278, -4.153390946401325223, -8.397313243818185668 ) ) ;
#1981 = CARTESIAN_POINT ( 'NONE',  ( 67.79734085828376067, -0.4026402971269220643, -16.39321520033831447 ) ) ;
#1982 = DIRECTION ( 'NONE',  ( 1.000000000000000000, 0.000000000000000000, 0.000000000000000000 ) ) ;
#1983 = CARTESIAN_POINT ( 'NONE',  ( 122.4397948109119767, -0.1624402480850797581, -16.17319339645315424 ) ) ;
#1984 = CARTESIAN_POINT ( 'NONE',  ( 76.63408154409412987, 1.697290617957241565, -10.89321520033831447 ) ) ;
#1985 = CARTESIAN_POINT ( 'NONE',  ( 135.3184548109119874, -4.105398160058917334, -19.34506575923121474 ) ) ;
#1986 = CARTESIAN_POINT ( 'NONE',  ( 125.2442149668909224, -11.55290408709314320, -16.24813457787868032 ) ) ;
#1988 = CARTESIAN_POINT ( 'NONE',  ( 124.5954081442453116, -3.383040157471821630, -19.15922257007629170 ) ) ;
#1987 = VECTOR ( 'NONE', #43432, 1000.000000000000000 ) ;
#1989 = CARTESIAN_POINT ( 'NONE',  ( 117.3343948109119737, -6.222761293078241884, -8.102969835052219238 ) ) ;
#1990 = CARTESIAN_POINT ( 'NONE',  ( 123.9146881442452894, -10.15424416112533912, -14.75197769757731336 ) ) ;
#1991 = ORIENTED_EDGE ( 'NONE', *, *, #13608, .T. ) ;
#1992 = CARTESIAN_POINT ( 'NONE',  ( 124.1983214775786166, -8.166667518702819706, -8.995218007635861213 ) ) ;
#1993 = EDGE_CURVE ( 'NONE', #43140, #12130, #45032, .T. ) ;
#1994 = CARTESIAN_POINT ( 'NONE',  ( 114.8951481442453115, -0.4660016031367893996, -10.09054647747474043 ) ) ;
#1995 = CARTESIAN_POINT ( 'NONE',  ( 115.6915515045247531, -6.936859964151250502, -18.39754474579286025 ) ) ;
#1996 = CARTESIAN_POINT ( 'NONE',  ( 113.6471614775786492, -5.638512984488995627, -18.83840828888717311 ) ) ;
#1997 = CARTESIAN_POINT ( 'NONE',  ( 123.9714148109119805, -8.899110576539710493, -16.42337572283490132 ) ) ;
#1998 = CARTESIAN_POINT ( 'NONE',  ( 125.6164881442453094, 0.2603800115204892296, -16.42320221600525088 ) ) ;
#1999 = CARTESIAN_POINT ( 'NONE',  ( 113.0523327545247838, -2.477300249445798297, -19.15521520033831138 ) ) ;
#2000 = CARTESIAN_POINT ( 'NONE',  ( 111.0381921295247878, -9.868328341294093420, -13.39321520033831447 ) ) ;
#2001 = DIRECTION ( 'NONE',  ( 1.000000000000000000, 0.000000000000000000, -0.000000000000000000 ) ) ;
#2002 = CARTESIAN_POINT ( 'NONE',  ( 114.8384214775786489, -10.15424416112533912, -14.75197769757731336 ) ) ;
#2003 = CARTESIAN_POINT ( 'NONE',  ( -12.36826994950264336, -4.374949827406453551, -7.393215200338315363 ) ) ;
#2004 = CARTESIAN_POINT ( 'NONE',  ( 112.9134265045247645, -2.791137627527939813, -8.388885654883777576 ) ) ;
#2005 = EDGE_LOOP ( 'NONE', ( #20661, #33610, #40801, #10397 ) ) ;
#2006 = CARTESIAN_POINT ( 'NONE',  ( 124.0281414775786146, -7.643976991954077427, -18.09477374809248928 ) ) ;
#2007 = CARTESIAN_POINT ( 'NONE',  ( 119.5350954359119839, 0.5291689781388270175, -13.89700978578772705 ) ) ;
#2008 = CARTESIAN_POINT ( 'NONE',  ( 122.6604860609119640, -6.564341423271550902, -7.887810678476487425 ) ) ;
#2009 = ORIENTED_EDGE ( 'NONE', *, *, #44122, .T. ) ;
#2010 = AXIS2_PLACEMENT_3D ( 'NONE', #28863, #15173, #18817 ) ;
#2011 = CARTESIAN_POINT ( 'NONE',  ( 87.80477198183443477, -25.99489077589524300, -13.39321520033831625 ) ) ;
#2012 = CARTESIAN_POINT ( 'NONE',  ( 106.9404577545248145, -2.791137627527939813, -18.39754474579286025 ) ) ;
#2013 = EDGE_LOOP ( 'NONE', ( #16435, #12122, #81, #28622 ) ) ;
#2014 = CARTESIAN_POINT ( 'NONE',  ( 119.3765548109119834, 0.9020085738987339008, -11.91225656197089222 ) ) ;
#2015 = CARTESIAN_POINT ( 'NONE',  ( 125.2194014775786286, 0.1319031606808879209, -14.10382304977623669 ) ) ;
#2016 = CARTESIAN_POINT ( 'NONE',  ( 116.4267681442453153, -6.222761293078241884, -8.102969835052219238 ) ) ;
#2017 = DIRECTION ( 'NONE',  ( 1.000000000000000000, 0.000000000000000000, 0.000000000000000000 ) ) ;
#2018 = FACE_OUTER_BOUND ( 'NONE', #39725, .T. ) ;
#2019 = LINE ( 'NONE', #5439, #1876 ) ;
#2020 = CARTESIAN_POINT ( 'NONE',  ( 115.6325948109119821, 0.2603800115204892296, -16.42320221600525088 ) ) ;
#2021 = CARTESIAN_POINT ( 'NONE',  ( 111.9410827545248708, -6.936859964151250502, -8.388885654883777576 ) ) ;
#2022 = AXIS2_PLACEMENT_3D ( 'NONE', #28422, #15182, #21574 ) ;
#2023 = CARTESIAN_POINT ( 'NONE',  ( 123.3474214775786209, -9.988377603198976828, -10.36322818467138340 ) ) ;
#2024 = ORIENTED_EDGE ( 'NONE', *, *, #10295, .T. ) ;
#2025 = CARTESIAN_POINT ( 'NONE',  ( 116.0296814775786345, -8.166667518702817929, -8.995218007635861213 ) ) ;
#2026 = CARTESIAN_POINT ( 'NONE',  ( 115.0653281442453277, -3.505236298600246325, -18.68346056562440793 ) ) ;
#2027 = LINE ( 'NONE', #29855, #19846 ) ;
#2028 = CARTESIAN_POINT ( 'NONE',  ( 111.7751814775786556, -7.893985811506177619, -18.51759400769804742 ) ) ;
#2029 = ORIENTED_EDGE ( 'NONE', *, *, #27260, .F. ) ;
#2030 = CARTESIAN_POINT ( 'NONE',  ( 121.6456214775786293, -10.63000616557722466, -14.87417383870573495 ) ) ;
#2031 = DIRECTION ( 'NONE',  ( 1.000000000000000000, 0.000000000000000000, -0.000000000000000000 ) ) ;
#2032 = CARTESIAN_POINT ( 'NONE',  ( 115.7417048073892687, -1.081026697600512732, -17.18181821144401056 ) ) ;
#2033 = CARTESIAN_POINT ( 'NONE',  ( 124.3431925510704303, -1.240377469759584628, -20.47314632408184920 ) ) ;
#2034 = CARTESIAN_POINT ( 'NONE',  ( -1.145390592550938447, -14.88589425535891841, -8.593215200338315540 ) ) ;
#2035 = CARTESIAN_POINT ( 'NONE',  ( 114.2711548109119803, -0.1624402480850797581, -16.17319339645315424 ) ) ;
#2036 = LINE ( 'NONE', #30314, #37177 ) ;
#2037 = EDGE_CURVE ( 'NONE', #38611, #14451, #22949, .T. ) ;
#2038 = CARTESIAN_POINT ( 'NONE',  ( 125.3463361817452579, -3.037870719615010540, -20.22337043927895550 ) ) ;
#2039 = B_SPLINE_CURVE_WITH_KNOTS ( 'NONE', 3,
 ( #14055, #34342, #44860, #13399 ),
 .UNSPECIFIED., .F., .F.,
 ( 4, 4 ),
 ( 0.000000000000000000, 1.000000000000000000 ),
 .UNSPECIFIED. ) ;
#2040 = CARTESIAN_POINT ( 'NONE',  ( 112.1155414775786454, -10.15424416112533912, -14.75197769757731336 ) ) ;
#2041 = APPLICATION_CONTEXT ( 'automotive_design' ) ;
#2042 = CARTESIAN_POINT ( 'NONE',  ( 112.4559014775786494, -9.988377603198976828, -10.36322818467138340 ) ) ;
#2043 = CARTESIAN_POINT ( 'NONE',  ( 121.4797829359119987, -5.367793381288652910, -18.78638297431638904 ) ) ;
#2044 = CARTESIAN_POINT ( 'NONE',  ( 113.5904348109119866, -7.893985811506177619, -18.51759400769804742 ) ) ;
#2045 = CARTESIAN_POINT ( 'NONE',  ( 115.0653281442453277, -3.505236298600246325, -18.68346056562440793 ) ) ;
#2046 = CARTESIAN_POINT ( 'NONE',  ( 124.4819548109119722, -7.893985811506177619, -18.51759400769804742 ) ) ;
#2047 = CARTESIAN_POINT ( 'NONE',  ( 123.0637881442452937, -0.4660016031367893996, -10.09054647747474043 ) ) ;
#2048 = ORIENTED_EDGE ( 'NONE', *, *, #29511, .T. ) ;
#2049 = CARTESIAN_POINT ( 'NONE',  ( 112.8529881442453302, -1.561330072975668060, -17.79121239304076596 ) ) ;
#2050 = CARTESIAN_POINT ( 'NONE',  ( 113.7468640045248236, -10.62599879583958717, -11.00651665394454604 ) ) ;
#2051 = CARTESIAN_POINT ( 'NONE',  ( 108.8156921295247912, -9.868328341294093420, -13.39321520033831447 ) ) ;
#2052 = CARTESIAN_POINT ( 'NONE',  ( 107.1488171295248861, 0.1403307496149613920, -13.39321520033831447 ) ) ;
#2053 = VECTOR ( 'NONE', #39873, 1000.000000000000000 ) ;
#2054 = CARTESIAN_POINT ( 'NONE',  ( 126.2872529661378564, -9.794462782700913195, -12.37543279432376231 ) ) ;
#2055 = CARTESIAN_POINT ( 'NONE',  ( 119.9438214775786378, -7.893985811506177619, -18.51759400769804742 ) ) ;
#2056 = VERTEX_POINT ( 'NONE', #24984 ) ;
#2057 = CARTESIAN_POINT ( 'NONE',  ( 125.3895814775786448, -7.893985811506177619, -18.51759400769804742 ) ) ;
#2058 = DIRECTION ( 'NONE',  ( 1.000000000000000000, 0.000000000000000000, 0.000000000000000000 ) ) ;
#2059 = FACE_OUTER_BOUND ( 'NONE', #24766, .T. ) ;
#2060 = CARTESIAN_POINT ( 'NONE',  ( 114.3846081442453197, 0.4262465694468514643, -12.03445270309931736 ) ) ;
#2061 = CARTESIAN_POINT ( 'NONE',  ( 119.6034614775786196, -6.344957434206665248, -7.627207830600338134 ) ) ;
#2062 = CARTESIAN_POINT ( 'NONE',  ( 108.2600671295247992, -10.62599879583958540, -13.39321520033831447 ) ) ;
#2063 = DIRECTION ( 'NONE',  ( -1.000000000000000000, 0.000000000000000000, 0.000000000000000000 ) ) ;
#2064 = ORIENTED_EDGE ( 'NONE', *, *, #36464, .F. ) ;
#2065 = CARTESIAN_POINT ( 'NONE',  ( 121.0783548109119749, -9.565557343593393824, -10.61323700422344274 ) ) ;
#2066 = CARTESIAN_POINT ( 'NONE',  ( 122.4965214775786251, 0.1319031606808879209, -14.10382304977623669 ) ) ;
#2067 = CARTESIAN_POINT ( 'NONE',  ( 120.4543614775786295, -4.089484607189486809, -7.948022111789456723 ) ) ;
#2068 = ADVANCED_FACE ( 'NONE', ( #28193 ), #12743, .T. ) ;
#2069 = CARTESIAN_POINT ( 'NONE',  ( 85.04324155394569118, -26.75858941326842810, -11.54476601486570964 ) ) ;
#2070 = CARTESIAN_POINT ( 'NONE',  ( 115.3489614775786407, -9.261995988541697145, -16.69588392320189030 ) ) ;
#2071 = CARTESIAN_POINT ( 'NONE',  ( 135.7171320688292724, -7.236526375436695524, -18.88165896190640680 ) ) ;
#2072 = CARTESIAN_POINT ( 'NONE',  ( 124.3117748109119844, 0.1319031606808879209, -14.10382304977623669 ) ) ;
#2073 = CARTESIAN_POINT ( 'NONE',  ( 119.2063748109119814, -7.894159318335828068, -9.358103419637847864 ) ) ;
#2074 = EDGE_LOOP ( 'NONE', ( #5365, #14211, #39192, #1577, #22410, #32120 ) ) ;
#2075 = CARTESIAN_POINT ( 'NONE',  ( 122.5215798109119874, -2.173413727453600508, -8.297982527556802879 ) ) ;
#2076 = CARTESIAN_POINT ( 'NONE',  ( 111.8886348109120092, -3.383040157471821630, -19.15922257007629170 ) ) ;
#2077 = CARTESIAN_POINT ( 'NONE',  ( 119.7736414775786358, 0.1319031606808879209, -14.10382304977623669 ) ) ;
#2078 = ORIENTED_EDGE ( 'NONE', *, *, #35027, .T. ) ;
#2079 = CARTESIAN_POINT ( 'NONE',  ( 124.3273610609119686, -6.340755971794695078, -8.611740276972781771 ) ) ;
#2080 = CARTESIAN_POINT ( 'NONE',  ( 120.5110881442453206, -6.344957434206665248, -7.627207830600338134 ) ) ;
#2081 = CARTESIAN_POINT ( 'NONE',  ( 112.4967077545247633, -7.250697342233347165, -7.631215200338321125 ) ) ;
#2082 = CARTESIAN_POINT ( 'NONE',  ( 114.9518748109119883, -7.643976991954077427, -18.09477374809248928 ) ) ;
#2083 = ORIENTED_EDGE ( 'NONE', *, *, #25009, .F. ) ;
#2084 = ORIENTED_EDGE ( 'NONE', *, *, #27230, .T. ) ;
#2085 = CARTESIAN_POINT ( 'NONE',  ( 124.5386814775786206, -4.153390946401325223, -8.397313243818185668 ) ) ;
#2086 = CARTESIAN_POINT ( 'NONE',  ( 120.6812681442452941, 0.1319031606808879209, -14.10382304977623669 ) ) ;
#2087 = PLANE ( 'NONE',  #6903 ) ;
#2088 = ORIENTED_EDGE ( 'NONE', *, *, #12602, .T. ) ;
#2089 = CARTESIAN_POINT ( 'NONE',  ( 118.5256548109119876, -0.4660016031367893996, -10.09054647747474043 ) ) ;
#2090 = DIRECTION ( 'NONE',  ( 0.000000000000000000, 0.000000000000000000, 1.000000000000000000 ) ) ;
#2091 = CARTESIAN_POINT ( 'NONE',  ( 116.1998614775786507, -10.63000616557722466, -14.87417383870573495 ) ) ;
#2093 = CARTESIAN_POINT ( 'NONE',  ( 117.9016614775786280, -0.1624402480850797581, -16.17319339645315424 ) ) ;
#2092 = CARTESIAN_POINT ( 'NONE',  ( 114.0442481442453300, -1.834011780172310813, -8.268836392978581529 ) ) ;
#2094 = CARTESIAN_POINT ( 'NONE',  ( 124.9357681442453014, -7.643976991954077427, -18.09477374809248928 ) ) ;
#2095 = CARTESIAN_POINT ( 'NONE',  ( 112.7962614775786676, -3.383040157471821630, -19.15922257007629170 ) ) ;
#2096 = ORIENTED_EDGE ( 'NONE', *, *, #43220, .F. ) ;
#2097 = CARTESIAN_POINT ( 'NONE',  ( 122.4965214775786251, 0.1319031606808879209, -14.10382304977623669 ) ) ;
#2098 = CARTESIAN_POINT ( 'NONE',  ( 114.1210660817262550, -2.423081321603721694, -17.89265170041262465 ) ) ;
#2099 = CARTESIAN_POINT ( 'NONE',  ( 114.6497546295247929, -4.863998795839590272, -7.631215200338315796 ) ) ;
#2100 = CARTESIAN_POINT ( 'NONE',  ( 114.5803015045248117, -6.936859964151250502, -18.39754474579286025 ) ) ;
#2101 = CARTESIAN_POINT ( 'NONE',  ( 111.9410827545248708, -2.477300249445798297, -19.15521520033831138 ) ) ;
#2102 = CARTESIAN_POINT ( 'NONE',  ( 117.0507614775786465, -10.30919188438810075, -12.61870101168855918 ) ) ;
#2103 = ORIENTED_EDGE ( 'NONE', *, *, #8142, .T. ) ;
#2104 = CARTESIAN_POINT ( 'NONE',  ( 121.7023481442452777, -9.261995988541697145, -16.69588392320189030 ) ) ;
#2105 = DIRECTION ( 'NONE',  ( -0.000000000000000000, -0.9284778069183721172, -0.3713878862591650232 ) ) ;
#2106 = CARTESIAN_POINT ( 'NONE',  ( 106.9404577545248145, -7.250697342233347165, -7.631215200338321125 ) ) ;
#2107 = CARTESIAN_POINT ( 'NONE',  ( 119.5467348109119712, -4.089484607189486809, -7.948022111789456723 ) ) ;
#2108 = CARTESIAN_POINT ( 'NONE',  ( 121.4187148109119789, -6.344957434206665248, -7.627207830600338134 ) ) ;
#2109 = CARTESIAN_POINT ( 'NONE',  ( 62.59689981967161998, -3.470785003659166090, -19.20476018416520958 ) ) ;
#2110 = CARTESIAN_POINT ( 'NONE',  ( 116.9195933520218489, -11.60549135878080129, -5.961931887625801174 ) ) ;
#2111 = EDGE_LOOP ( 'NONE', ( #24890, #26882, #38289, #33119 ) ) ;
#2112 = DIRECTION ( 'NONE',  ( 0.000000000000000000, 0.6004852223388321697, -0.7996358532186279566 ) ) ;
#2113 = CARTESIAN_POINT ( 'NONE',  ( 109.2294398899149570, -10.40495872603004912, -13.78690482381271920 ) ) ;
#2114 = CARTESIAN_POINT ( 'NONE',  ( 125.6164881442453094, -9.565557343593413364, -10.61323700422348004 ) ) ;
#2115 = CARTESIAN_POINT ( 'NONE',  ( 112.7050671295247923, 0.1403307496149613920, -13.39321520033831447 ) ) ;
#2116 = CARTESIAN_POINT ( 'NONE',  ( 111.5243640045248412, 0.1403307496149616695, -15.46607636864997204 ) ) ;
#2118 = CIRCLE ( 'NONE', #36346, 2.999999999999999556 ) ;
#2117 = CARTESIAN_POINT ( 'NONE',  ( 116.8805814775786445, -3.505236298600246325, -18.68346056562440793 ) ) ;
#2119 = LINE ( 'NONE', #6857, #35006 ) ;
#2120 = CARTESIAN_POINT ( 'NONE',  ( 69.72146619215227759, -25.52849560314718858, -5.786566508650934360 ) ) ;
#2121 = CARTESIAN_POINT ( 'NONE',  ( 111.2646414775786496, -8.899110576539710493, -16.42337572283490132 ) ) ;
#2122 = CARTESIAN_POINT ( 'NONE',  ( 124.9924948109119924, -4.089484607189486809, -7.948022111789456723 ) ) ;
#2123 = ORIENTED_EDGE ( 'NONE', *, *, #31988, .T. ) ;
#2124 = CARTESIAN_POINT ( 'NONE',  ( 121.0216281442452981, -7.894159318335828068, -9.358103419637847864 ) ) ;
#2125 = CARTESIAN_POINT ( 'NONE',  ( 116.5969481442453031, 0.5811942927096154232, -14.16772938898807155 ) ) ;
#2126 = CARTESIAN_POINT ( 'NONE',  ( 122.4965214775786251, -10.30919188438810075, -12.61870101168855918 ) ) ;
#2127 = CARTESIAN_POINT ( 'NONE',  ( 124.4252281442452812, -0.8288870151387760510, -10.36305467784173118 ) ) ;
#2128 = VERTEX_POINT ( 'NONE', #24757 ) ;
#2129 = CARTESIAN_POINT ( 'NONE',  ( 70.19189222814998175, -59.11650476797663600, -36.84940499091918298 ) ) ;
#2130 = EDGE_CURVE ( 'NONE', #30086, #40322, #14182, .T. ) ;
#2131 = CARTESIAN_POINT ( 'NONE',  ( 123.2339681442453241, -6.344957434206665248, -7.627207830600338134 ) ) ;
#2132 = CARTESIAN_POINT ( 'NONE',  ( 112.9097148109120070, -9.565557343593413364, -10.61323700422348004 ) ) ;
#2133 = CARTESIAN_POINT ( 'NONE',  ( 111.6617281442453304, 0.4262465694468514643, -12.03445270309931736 ) ) ;
#2134 = CARTESIAN_POINT ( 'NONE',  ( 108.3989733795248753, -8.938348069036489818, -17.46756447353520159 ) ) ;
#2135 = CARTESIAN_POINT ( 'NONE',  ( 120.6463454359119822, 0.5291689781388270175, -13.89700978578772705 ) ) ;
#2136 = CARTESIAN_POINT ( 'NONE',  ( 138.2184548109119930, -2.458068653496962686, -15.34808096303632396 ) ) ;
#2137 = CARTESIAN_POINT ( 'NONE',  ( 107.9822546295247889, -4.863998795839590272, -18.39754474579285315 ) ) ;
#2138 = CIRCLE ( 'NONE', #36344, 6.479565957685750277 ) ;
#2139 = CARTESIAN_POINT ( 'NONE',  ( 123.4939235609119663, -9.645473719204776586, -14.86997237629376656 ) ) ;
#2140 = CARTESIAN_POINT ( 'NONE',  ( 118.3554748109119998, -9.565557343593413364, -10.61323700422348004 ) ) ;
#2141 = CARTESIAN_POINT ( 'NONE',  ( 111.3780948109119890, -5.574606645277164318, -18.38911715685844683 ) ) ;
#2142 = CARTESIAN_POINT ( 'NONE',  ( 126.2889637360267159, -5.888109775029882975, -18.32339328746833473 ) ) ;
#2143 = ORIENTED_EDGE ( 'NONE', *, *, #28955, .T. ) ;
#2144 = DIRECTION ( 'NONE',  ( 0.8636456077245086016, -0.5040994586965593660, 0.000000000000000000 ) ) ;
#2145 = CARTESIAN_POINT ( 'NONE',  ( 117.5613014775786525, -10.15424416112533912, -14.75197769757731336 ) ) ;
#2146 = CARTESIAN_POINT ( 'NONE',  ( 113.4821938206745386, -2.348512537728063787, -17.99195118506216318 ) ) ;
#2147 = EDGE_CURVE ( 'NONE', #24167, #2128, #34986, .T. ) ;
#2148 = CARTESIAN_POINT ( 'NONE',  ( 68.16708570727516303, -1.180063502400580999, -10.39321520033831625 ) ) ;
#2149 = DIRECTION ( 'NONE',  ( 0.000000000000000000, 0.2950959089608259922, -0.9554676365605399013 ) ) ;
#2151 = CARTESIAN_POINT ( 'NONE',  ( 123.2339681442453241, -6.344957434206665248, -7.627207830600338134 ) ) ;
#2150 = LINE ( 'NONE', #33157, #11976 ) ;
#2152 = CARTESIAN_POINT ( 'NONE',  ( 123.6877814775786533, -6.222761293078241884, -8.102969835052219238 ) ) ;
#2153 = ORIENTED_EDGE ( 'NONE', *, *, #14241, .F. ) ;
#2154 = CIRCLE ( 'NONE', #26946, 4.999999999999998224 ) ;
#2155 = CARTESIAN_POINT ( 'NONE',  ( 110.1534981608379837, 0.3867979994853637526, -14.64321520033831447 ) ) ;
#2156 = CARTESIAN_POINT ( 'NONE',  ( 65.41257106814472877, -15.47412461924279725, -10.39321520033831625 ) ) ;
#2157 = CARTESIAN_POINT ( 'NONE',  ( 111.7327233795247849, -1.325403438956436419, -9.854619843455211026 ) ) ;
#2158 = EDGE_CURVE ( 'NONE', #13382, #35800, #29749, .T. ) ;
#2159 = CARTESIAN_POINT ( 'NONE',  ( 122.9503348109119827, -9.859900752359378018, -12.68260735090039759 ) ) ;
#2160 = CARTESIAN_POINT ( 'NONE',  ( 119.8870948109119752, -0.8288870151387760510, -10.36305467784173118 ) ) ;
#2161 = EDGE_CURVE ( 'NONE', #34050, #35601, #31920, .T. ) ;
#2162 = CARTESIAN_POINT ( 'NONE',  ( 125.3296504289671844, 1.640368036495027715, -16.28920770532023710 ) ) ;
#2163 = CARTESIAN_POINT ( 'NONE',  ( 115.0664733795247798, -1.325403438956436419, -9.854619843455211026 ) ) ;
#2164 = CARTESIAN_POINT ( 'NONE',  ( 116.5026997424434114, -0.9924539043446216624, -17.29976612834909133 ) ) ;
#2165 = FACE_OUTER_BOUND ( 'NONE', #28094, .T. ) ;
#2166 = DIRECTION ( 'NONE',  ( 1.000000000000000000, 0.000000000000000000, 0.000000000000000000 ) ) ;
#2167 = CARTESIAN_POINT ( 'NONE',  ( 111.4549108795247747, -8.938348069036489818, -9.318865927141430916 ) ) ;
#2168 = CARTESIAN_POINT ( 'NONE',  ( -13.77941350934472808, -4.501197414032524158, -18.63512858394170379 ) ) ;
#2169 = CARTESIAN_POINT ( 'NONE',  ( 112.7745202545247878, -10.62599879583958717, -15.77991374673208469 ) ) ;
#2170 = CARTESIAN_POINT ( 'NONE',  ( 120.2841814775786276, 0.9020085738987339008, -11.91225656197089222 ) ) ;
#2171 = CARTESIAN_POINT ( 'NONE',  ( 123.1205148109119563, -1.834011780172310813, -8.268836392978581529 ) ) ;
#2172 = CARTESIAN_POINT ( 'NONE',  ( 106.1764733795248219, -8.938348069036489818, -17.46756447353520159 ) ) ;
#2173 = CARTESIAN_POINT ( 'NONE',  ( 116.4267681442453153, -3.383040157471821630, -19.15922257007629170 ) ) ;
#2174 = CARTESIAN_POINT ( 'NONE',  ( 114.2144281442453178, -8.166667518702817929, -8.995218007635859436 ) ) ;
#2175 = ORIENTED_EDGE ( 'NONE', *, *, #19187, .F. ) ;
#2176 = CARTESIAN_POINT ( 'NONE',  ( 70.36267391504962632, -5.685877709920933221, -4.893215200338314474 ) ) ;
#2177 = EDGE_CURVE ( 'NONE', #18453, #20631, #29303, .T. ) ;
#2178 = CARTESIAN_POINT ( 'NONE',  ( 112.2857214775786474, -5.574606645277164318, -18.38911715685844683 ) ) ;
#2179 = CARTESIAN_POINT ( 'NONE',  ( 119.4900081442453086, -1.834011780172310813, -8.268836392978581529 ) ) ;
#2180 = AXIS2_PLACEMENT_3D ( 'NONE', #22807, #19390, #12787 ) ;
#2181 = CARTESIAN_POINT ( 'NONE',  ( 124.3685014775786328, 0.4262465694468514643, -12.03445270309931736 ) ) ;
#2182 = CARTESIAN_POINT ( 'NONE',  ( 112.3424481442453384, -3.505236298600246325, -18.68346056562440793 ) ) ;
#2183 = ORIENTED_EDGE ( 'NONE', *, *, #32555, .T. ) ;
#2184 = EDGE_CURVE ( 'NONE', #38164, #19850, #25845, .T. ) ;
#2185 = CARTESIAN_POINT ( 'NONE',  ( 113.4202548109119846, 0.1319031606808879209, -14.10382304977623669 ) ) ;
#2186 = CARTESIAN_POINT ( 'NONE',  ( 125.8433948109119456, -1.834011780172310813, -8.268836392978581529 ) ) ;
#2187 = EDGE_CURVE ( 'NONE', #4486, #33968, #12023, .T. ) ;
#2188 = EDGE_CURVE ( 'NONE', #18093, #38601, #5278, .T. ) ;
#2189 = CARTESIAN_POINT ( 'NONE',  ( 110.1353015045248469, -2.477300249445798297, -7.631215200338321125 ) ) ;
#2190 = AXIS2_PLACEMENT_3D ( 'NONE', #12234, #8583, #22482 ) ;
#2191 = CARTESIAN_POINT ( 'NONE',  ( 120.5678148109119832, -1.833838273342659253, -17.42832698103878286 ) ) ;
#2192 = CARTESIAN_POINT ( 'NONE',  ( 116.7994817539454147, -2.735128593956382748, -18.16285249951504355 ) ) ;
#2193 = CARTESIAN_POINT ( 'NONE',  ( 87.41631446019775353, -26.60966817898065884, -11.90521360603286816 ) ) ;
#2194 = VERTEX_POINT ( 'NONE', #12208 ) ;
#2195 = VECTOR ( 'NONE', #28078, 1000.000000000000000 ) ;
#2196 = CARTESIAN_POINT ( 'NONE',  ( 121.8965016859119856, -0.6942167230862511529, -9.935906262978006609 ) ) ;
#2197 = CARTESIAN_POINT ( 'NONE',  ( 123.7445081442452874, -1.561330072975668948, -17.79121239304076951 ) ) ;
#2198 = CARTESIAN_POINT ( 'NONE',  ( 138.2184548109119930, -5.622599431619523358, -7.441364641445410655 ) ) ;
#2199 = DIRECTION ( 'NONE',  ( -0.7871354856660162103, -0.4483307682966942709, -0.4235767337848251879 ) ) ;
#2200 = CARTESIAN_POINT ( 'NONE',  ( -1.932019669644797988, -4.762702382056356321, -17.89321520033831447 ) ) ;
#2201 = CARTESIAN_POINT ( 'NONE',  ( 114.0923066399283812, 0.4261359969231631739, -14.64321520033831447 ) ) ;
#2202 = CARTESIAN_POINT ( 'NONE',  ( 108.2600671295247992, 0.1403307496149613920, -13.39321520033831447 ) ) ;
#2203 = CARTESIAN_POINT ( 'NONE',  ( 109.4177504229301690, 0.1075849324168598464, -14.64321520033834645 ) ) ;
#2204 = CARTESIAN_POINT ( 'NONE',  ( 70.19189222814998175, -41.58126682492877535, -29.83537093841426469 ) ) ;
#2205 = CONICAL_SURFACE ( 'NONE', #44488, 1.610000000000000986, 0.9599310885968765916 ) ;
#2206 = CARTESIAN_POINT ( 'NONE',  ( 125.3421052277123096, -11.71169103848138526, -15.18956764462613584 ) ) ;
#2207 = FACE_OUTER_BOUND ( 'NONE', #20726, .T. ) ;
#2208 = CARTESIAN_POINT ( 'NONE',  ( 115.9162281442453093, -5.574606645277164318, -18.38911715685844683 ) ) ;
#2209 = CARTESIAN_POINT ( 'NONE',  ( 119.7434548109119419, -0.7786512460255691215, -16.99959486913572704 ) ) ;
#2210 = ORIENTED_EDGE ( 'NONE', *, *, #7604, .T. ) ;
#2211 = CARTESIAN_POINT ( 'NONE',  ( 121.8158014775786171, -5.638512984488999180, -18.83840828888717311 ) ) ;
#2212 = CARTESIAN_POINT ( 'NONE',  ( 114.3278814775786429, -10.30919188438810075, -12.61870101168855918 ) ) ;
#2213 = CARTESIAN_POINT ( 'NONE',  ( 113.5385046295247804, -4.863998795839590272, -18.39754474579285315 ) ) ;
#2214 = DIRECTION ( 'NONE',  ( 0.000000000000000000, 0.6004852223388322807, -0.7996358532186279566 ) ) ;
#2215 = CARTESIAN_POINT ( 'NONE',  ( 122.8368814775786291, -7.894159318335828068, -9.358103419637847864 ) ) ;
#2216 = CARTESIAN_POINT ( 'NONE',  ( 124.1983214775786166, -8.166667518702819706, -8.995218007635861213 ) ) ;
#2217 = CARTESIAN_POINT ( 'NONE',  ( 116.1777233795247781, -8.938348069036489818, -17.46756447353520159 ) ) ;
#2218 = CARTESIAN_POINT ( 'NONE',  ( 107.7044421295247929, -9.868328341294093420, -13.39321520033831447 ) ) ;
#2219 = CARTESIAN_POINT ( 'NONE',  ( 83.19148113855052884, -31.91406586441351934, -23.42170072420262628 ) ) ;
#2220 = CARTESIAN_POINT ( 'NONE',  ( 114.4413348109119823, -0.8288870151387760510, -10.36305467784173118 ) ) ;
#2221 = VECTOR ( 'NONE', #16331, 1000.000000000000000 ) ;
#2222 = CARTESIAN_POINT ( 'NONE',  ( 115.1220548109119761, -1.833838273342658809, -17.42832698103878286 ) ) ;
#2223 = CARTESIAN_POINT ( 'NONE',  ( 61.69189222814998175, -61.90644496644519990, -36.30514255143466329 ) ) ;
#2224 = CARTESIAN_POINT ( 'NONE',  ( 113.1217858795247935, -8.402594152722688392, -9.854619843455216355 ) ) ;
#2225 = VERTEX_POINT ( 'NONE', #26563 ) ;
#2226 = AXIS2_PLACEMENT_3D ( 'NONE', #31900, #39655, #15484 ) ;
#2227 = CARTESIAN_POINT ( 'NONE',  ( 109.2296046993104710, -0.1282053629079296375, -15.30017343217149950 ) ) ;
#2228 = CARTESIAN_POINT ( 'NONE',  ( 124.5386814775786206, -4.153390946401325223, -8.397313243818185668 ) ) ;
#2229 = CARTESIAN_POINT ( 'NONE',  ( 123.0772048109119652, -7.554583864224885481, -18.48844787311982785 ) ) ;
#2230 = CARTESIAN_POINT ( 'NONE',  ( 122.1048610609119720, -3.163656168406935087, -18.89861972220014508 ) ) ;
#2231 = ORIENTED_EDGE ( 'NONE', *, *, #41365, .T. ) ;
#2232 = CARTESIAN_POINT ( 'NONE',  ( -12.36826994950264513, -4.374949827406456215, -19.39321520033831447 ) ) ;
#2233 = CARTESIAN_POINT ( 'NONE',  ( 116.3474387856597758, -11.99696240085007837, -20.96724589306712261 ) ) ;
#2234 = EDGE_LOOP ( 'NONE', ( #6707, #17676, #1870, #18909 ) ) ;
#2235 = CARTESIAN_POINT ( 'NONE',  ( 119.2063748109119814, -1.561330072975668504, -17.79121239304076951 ) ) ;
#2236 = CARTESIAN_POINT ( 'NONE',  ( 125.5597614775786326, -7.894159318335828068, -9.358103419637847864 ) ) ;
#2237 = CARTESIAN_POINT ( 'NONE',  ( 113.1366214775786432, -7.643976991954077427, -18.09477374809248928 ) ) ;
#2238 = SURFACE_STYLE_USAGE ( .BOTH. , #19579 ) ;
#2239 = DIRECTION ( 'NONE',  ( 0.9063289528979890930, 0.4225728684367167087, 0.000000000000000000 ) ) ;
#2240 = CARTESIAN_POINT ( 'NONE',  ( 111.7184548109119788, -9.162420673101799196, -15.99582338542316151 ) ) ;
#2241 = CARTESIAN_POINT ( 'NONE',  ( 116.0864081442453113, -9.988377603198976828, -10.36322818467138340 ) ) ;
#2242 = ADVANCED_FACE ( 'NONE', ( #11984 ), #22304, .T. ) ;
#2243 = CARTESIAN_POINT ( 'NONE',  ( 113.1912390045248031, -9.868328341294098749, -11.32035403202665869 ) ) ;
#2244 = TOROIDAL_SURFACE ( 'NONE', #34311, 10.00000000000000000, 2.000000000000000000 ) ;
#2245 = CARTESIAN_POINT ( 'NONE',  ( 124.3117748109119844, -10.30919188438810075, -12.61870101168855918 ) ) ;
#2246 = LINE ( 'NONE', #37120, #977 ) ;
#2247 = ORIENTED_EDGE ( 'NONE', *, *, #38111, .T. ) ;
#2248 = EDGE_CURVE ( 'NONE', #219, #6975, #23691, .T. ) ;
#2249 = CARTESIAN_POINT ( 'NONE',  ( 114.7816948109119863, 0.5811942927096154232, -14.16772938898807155 ) ) ;
#2250 = CARTESIAN_POINT ( 'NONE',  ( 115.2922348109119781, 0.4262465694468514643, -12.03445270309931736 ) ) ;
#2251 = CARTESIAN_POINT ( 'NONE',  ( 126.2184548109119788, -5.568102603702699049, -18.34339073538272302 ) ) ;
#2252 = CARTESIAN_POINT ( 'NONE',  ( 125.4463081442452932, -4.153390946401325223, -8.397313243818185668 ) ) ;
#2253 = ORIENTED_EDGE ( 'NONE', *, *, #38111, .F. ) ;
#2254 = CIRCLE ( 'NONE', #26288, 2.999999999999999556 ) ;
#2255 = CARTESIAN_POINT ( 'NONE',  ( 120.3409081442453044, -0.4660016031367893996, -10.09054647747474043 ) ) ;
#2256 = DIRECTION ( 'NONE',  ( 1.000000000000000000, 0.000000000000000000, 0.000000000000000000 ) ) ;
#2257 = DIRECTION ( 'NONE',  ( 1.000000000000000000, 0.000000000000000000, -0.000000000000000000 ) ) ;
#2258 = AXIS2_PLACEMENT_3D ( 'NONE', #28724, #666, #4760 ) ;
#2259 = CARTESIAN_POINT ( 'NONE',  ( 112.1155012242753344, -10.15403529472779809, -14.75050927016698310 ) ) ;
#2260 = CARTESIAN_POINT ( 'NONE',  ( 136.3568202015705992, -2.634417929066116937, -8.029337161656213695 ) ) ;
#2261 = CARTESIAN_POINT ( 'NONE',  ( 113.7606148109119886, -7.894159318335828068, -9.358103419637847864 ) ) ;
#2262 = CARTESIAN_POINT ( 'NONE',  ( 111.2184548109119788, -1.295815253274133161, -16.89579513612386563 ) ) ;
#2263 = DIRECTION ( 'NONE',  ( -0.9908103287288503314, 0.1352586133457950868, 0.000000000000000000 ) ) ;
#2264 = CARTESIAN_POINT ( 'NONE',  ( 114.7249681442453237, -9.565557343593413364, -10.61323700422348004 ) ) ;
#2265 = CARTESIAN_POINT ( 'NONE',  ( 115.0086014775786509, -4.089484607189486809, -7.948022111789456723 ) ) ;
#2266 = CARTESIAN_POINT ( 'NONE',  ( 121.6186891859119896, -1.406689858478933353, -17.56299727309130887 ) ) ;
#2267 = CARTESIAN_POINT ( 'NONE',  ( 113.8173414775786512, 0.2603800115204892296, -16.42320221600525088 ) ) ;
#2268 = CARTESIAN_POINT ( 'NONE',  ( 117.3343948109119737, -6.222761293078241884, -8.102969835052219238 ) ) ;
#2269 = CARTESIAN_POINT ( 'NONE',  ( 123.2339681442453241, -6.344957434206665248, -7.627207830600338134 ) ) ;
#2270 = CARTESIAN_POINT ( 'NONE',  ( 123.4041481442452834, -10.30919188438810075, -12.61870101168855918 ) ) ;
#2271 = ORIENTED_EDGE ( 'NONE', *, *, #12226, .T. ) ;
#2272 = CARTESIAN_POINT ( 'NONE',  ( 114.4980614775786592, -7.893985811506177619, -18.51759400769804742 ) ) ;
#2273 = CARTESIAN_POINT ( 'NONE',  ( 110.6214733795247867, -8.938348069036489818, -17.46756447353520159 ) ) ;
#2274 = CARTESIAN_POINT ( 'NONE',  ( 108.4684265045248424, -2.791137627527939813, -8.388885654883777576 ) ) ;
#2275 = CARTESIAN_POINT ( 'NONE',  ( 110.5520202545248054, 0.1403307496149616695, -11.32035403202665336 ) ) ;
#2276 = CIRCLE ( 'NONE', #16889, 0.5000000000000004441 ) ;
#2277 = CARTESIAN_POINT ( 'NONE',  ( 64.01282776924008999, -34.86145050234443943, -5.893215200338315363 ) ) ;
#2278 = CARTESIAN_POINT ( 'NONE',  ( 119.8870948109119752, -9.261995988541697145, -16.69588392320189030 ) ) ;
#2279 = EDGE_LOOP ( 'NONE', ( #24807, #42920, #8491, #13924 ) ) ;
#2280 = CARTESIAN_POINT ( 'NONE',  ( 124.7221293297047851, -9.583721038254804370, -19.61132113298129553 ) ) ;
#2281 = CARTESIAN_POINT ( 'NONE',  ( 109.2294611991032554, -8.247533281633225855, -8.767455091437543757 ) ) ;
#2282 = CARTESIAN_POINT ( 'NONE',  ( 120.6253743740715407, -2.419733177069661512, -17.89711025544711376 ) ) ;
#2283 = CARTESIAN_POINT ( 'NONE',  ( 115.0653281442453277, -3.505236298600246325, -18.68346056562440793 ) ) ;
#2284 = CARTESIAN_POINT ( 'NONE',  ( 105.6903015045248253, -6.936859964151250502, -18.39754474579286025 ) ) ;
#2285 = EDGE_CURVE ( 'NONE', #42482, #30793, #33836, .T. ) ;
#2286 = CARTESIAN_POINT ( 'NONE',  ( 118.6958348109119754, -6.344957434206665248, -7.627207830600338134 ) ) ;
#2287 = CARTESIAN_POINT ( 'NONE',  ( 107.2182702545248105, -10.62599879583958717, -15.77991374673208469 ) ) ;
#2288 = CARTESIAN_POINT ( 'NONE',  ( 116.5944421295247793, -4.863998795839590272, -13.39321520033831447 ) ) ;
#2289 = ORIENTED_EDGE ( 'NONE', *, *, #1500, .F. ) ;
#2290 = CARTESIAN_POINT ( 'NONE',  ( 111.0001630180080809, 0.7607806665038616689, -14.64321520033831447 ) ) ;
#2291 = VECTOR ( 'NONE', #33970, 999.9999999999998863 ) ;
#2292 = CARTESIAN_POINT ( 'NONE',  ( 121.4754414775786131, -1.833838273342659697, -17.42832698103878286 ) ) ;
#2293 = CARTESIAN_POINT ( 'NONE',  ( 120.3409081442453044, -0.4660016031367893996, -10.09054647747474043 ) ) ;
#2294 = CARTESIAN_POINT ( 'NONE',  ( 115.2355081442453155, 0.1319031606808879209, -14.10382304977623669 ) ) ;
#2295 = CARTESIAN_POINT ( 'NONE',  ( 113.7606148109119886, -1.561330072975668060, -17.79121239304076596 ) ) ;
#2296 = CARTESIAN_POINT ( 'NONE',  ( 117.8659193777725278, -1.267766418764730840, -16.93314635290706605 ) ) ;
#2297 = CARTESIAN_POINT ( 'NONE',  ( 126.2455040230451289, -0.9944417698632344038, -10.20348866579734448 ) ) ;
#2298 = CARTESIAN_POINT ( 'NONE',  ( 119.3765548109119834, -10.15424416112533912, -14.75197769757731336 ) ) ;
#2299 = VERTEX_POINT ( 'NONE', #6494 ) ;
#2300 = CARTESIAN_POINT ( 'NONE',  ( 119.6601881442453106, -8.166667518702801942, -8.995218007635848778 ) ) ;
#2301 = EDGE_CURVE ( 'NONE', #39549, #1444, #33117, .T. ) ;
#2302 = CARTESIAN_POINT ( 'NONE',  ( 113.0231681442453322, 0.9020085738987339008, -11.91225656197089222 ) ) ;
#2303 = CARTESIAN_POINT ( 'NONE',  ( 121.3619881442452879, -5.574606645277164318, -18.38911715685844683 ) ) ;
#2304 = ORIENTED_EDGE ( 'NONE', *, *, #38190, .T. ) ;
#2305 = CARTESIAN_POINT ( 'NONE',  ( 120.9936110609119737, -6.340755971794695078, -8.611740276972781771 ) ) ;
#2306 = CARTESIAN_POINT ( 'NONE',  ( 120.2841814775786276, 0.9020085738987339008, -11.91225656197089222 ) ) ;
#2307 = CARTESIAN_POINT ( 'NONE',  ( 112.2188952545247531, 0.8980012041604421569, -11.00651665394454071 ) ) ;
#2308 = CARTESIAN_POINT ( 'NONE',  ( 114.8384214775786489, -10.15424416112533912, -14.75197769757731336 ) ) ;
#2309 = ORIENTED_EDGE ( 'NONE', *, *, #2188, .T. ) ;
#2310 = ORIENTED_EDGE ( 'NONE', *, *, #8142, .F. ) ;
#2311 = AXIS2_PLACEMENT_3D ( 'NONE', #37760, #732, #28339 ) ;
#2312 = CARTESIAN_POINT ( 'NONE',  ( 126.2972081442452890, -2.084020599724406786, -8.691656652584148546 ) ) ;
#2313 = CARTESIAN_POINT ( 'NONE',  ( 121.2485348109119769, -8.899110576539710493, -16.42337572283490132 ) ) ;
#2314 = FILL_AREA_STYLE_COLOUR ( '', #44047 ) ;
#2315 = DIRECTION ( 'NONE',  ( 0.9609149988134837450, -0.1028163501681639419, 0.2570431154366518145 ) ) ;
#2316 = CARTESIAN_POINT ( 'NONE',  ( 120.1707281442453166, 0.2603800115204892296, -16.42320221600525088 ) ) ;
#2317 = DIRECTION ( 'NONE',  ( -0.000000000000000000, -0.9284778069183721172, -0.3713878862591650232 ) ) ;
#2318 = VECTOR ( 'NONE', #7951, 1000.000000000000000 ) ;
#2319 = EDGE_CURVE ( 'NONE', #21889, #31663, #36791, .T. ) ;
#2320 = CARTESIAN_POINT ( 'NONE',  ( 116.5969481442453031, 0.5811942927096154232, -14.16772938898807155 ) ) ;
#2322 = CARTESIAN_POINT ( 'NONE',  ( 114.4980614775786734, -2.084020599724406786, -8.691656652584148546 ) ) ;
#2321 = CARTESIAN_POINT ( 'NONE',  ( 116.2565881442452991, -9.261995988541697145, -16.69588392320189030 ) ) ;
#2323 = CARTESIAN_POINT ( 'NONE',  ( 125.0492214775786266, -3.505236298600246325, -18.68346056562440793 ) ) ;
#2324 = CARTESIAN_POINT ( 'NONE',  ( 113.9875214775786532, -0.4660016031367893996, -10.09054647747474043 ) ) ;
#2325 = EDGE_LOOP ( 'NONE', ( #33811, #7565, #42276, #17085, #17615 ) ) ;
#2326 = CARTESIAN_POINT ( 'NONE',  ( 124.9924948109119924, -5.574606645277164318, -18.38911715685844683 ) ) ;
#2327 = DIRECTION ( 'NONE',  ( 0.000000000000000000, 0.6004852223388321697, -0.7996358532186279566 ) ) ;
#2328 = CYLINDRICAL_SURFACE ( 'NONE', #20561, 8.000000000000001776 ) ;
#2329 = CARTESIAN_POINT ( 'NONE',  ( 113.6774108795247997, -8.938348069036489818, -9.318865927141430916 ) ) ;
#2330 = CARTESIAN_POINT ( 'NONE',  ( 113.9552233795247815, -1.325403438956436419, -9.854619843455211026 ) ) ;
#2331 = CARTESIAN_POINT ( 'NONE',  ( 111.7327233795247849, -8.938348069036489818, -17.46756447353520159 ) ) ;
#2332 = CARTESIAN_POINT ( 'NONE',  ( 121.9292548109119849, -1.561330072975668948, -17.79121239304076951 ) ) ;
#2333 = VERTEX_POINT ( 'NONE', #13563 ) ;
#2334 = CARTESIAN_POINT ( 'NONE',  ( 119.1496481442453046, -3.383040157471821630, -19.15922257007629170 ) ) ;
#2335 = CARTESIAN_POINT ( 'NONE',  ( 112.6260814775786514, -0.8288870151387760510, -10.36305467784173118 ) ) ;
#2336 = DIRECTION ( 'NONE',  ( -0.000000000000000000, -0.3818493186865896671, 0.9242245927363040847 ) ) ;
#2337 = CARTESIAN_POINT ( 'NONE',  ( 119.4332814775786318, -0.4660016031367893996, -10.09054647747474043 ) ) ;
#2338 = CARTESIAN_POINT ( 'NONE',  ( 119.7736414775786358, -10.30919188438810075, -12.61870101168855918 ) ) ;
#2339 = CYLINDRICAL_SURFACE ( 'NONE', #11824, 5.000000000000000000 ) ;
#2340 = CARTESIAN_POINT ( 'NONE',  ( 124.1415948109119540, -3.505236298600246325, -18.68346056562440793 ) ) ;
#2341 = CARTESIAN_POINT ( 'NONE',  ( 125.4584548109119737, -8.702576499751430106, -17.94267422983053706 ) ) ;
#2342 = CARTESIAN_POINT ( 'NONE',  ( 121.6881423109119709, -0.4387604401700512802, -15.73000352943951619 ) ) ;
#2343 = ORIENTED_EDGE ( 'NONE', *, *, #857, .F. ) ;
#2344 = CARTESIAN_POINT ( 'NONE',  ( -2.588851517412736669, -7.061334938601206979, -7.481563165383908753 ) ) ;
#2345 = CARTESIAN_POINT ( 'NONE',  ( 114.4291028165343960, -2.324775150319240868, -18.02356106541842351 ) ) ;
#2346 = CARTESIAN_POINT ( 'NONE',  ( 123.2339681442453241, -3.505236298600246325, -18.68346056562440793 ) ) ;
#2347 = CARTESIAN_POINT ( 'NONE',  ( 106.9404577545248145, -2.791137627527939813, -18.39754474579286025 ) ) ;
#2348 = CARTESIAN_POINT ( 'NONE',  ( 110.7603796295247918, -4.863998795839590272, -8.388885654883775800 ) ) ;
#2349 = CARTESIAN_POINT ( 'NONE',  ( 116.6536748109119941, -10.15424416112533912, -14.75197769757731336 ) ) ;
#2350 = CARTESIAN_POINT ( 'NONE',  ( 69.97727075072853609, -25.42500284328563964, -5.723131632646515143 ) ) ;
#2351 = CARTESIAN_POINT ( 'NONE',  ( 113.4202548109119846, 0.1319031606808879209, -14.10382304977623669 ) ) ;
#2352 = CARTESIAN_POINT ( 'NONE',  ( 123.8579614775786126, 0.5811942927096110934, -14.16772938898807510 ) ) ;
#2353 = ORIENTED_EDGE ( 'NONE', *, *, #972, .T. ) ;
#2354 = CARTESIAN_POINT ( 'NONE',  ( 122.4965214775786251, 0.1319031606808879209, -14.10382304977623669 ) ) ;
#2355 = VECTOR ( 'NONE', #41919, 1000.000000000000000 ) ;
#2356 = CARTESIAN_POINT ( 'NONE',  ( 116.8238548109119819, -4.089484607189486809, -7.948022111789456723 ) ) ;
#2357 = CARTESIAN_POINT ( 'NONE',  ( 124.3117748109119844, -10.30919188438810075, -12.61870101168855918 ) ) ;
#2358 = EDGE_CURVE ( 'NONE', #37481, #40668, #44581, .T. ) ;
#2359 = B_SPLINE_CURVE_WITH_KNOTS ( 'NONE', 3,
 ( #13125, #9933, #40711, #30444, #20419, #10158, #23846, #9471, #34302, #33847 ),
 .UNSPECIFIED., .F., .F.,
 ( 4, 3, 3, 4 ),
 ( 0.000000000000000000, 0.0001671877560958089928, 0.0003343755126086545080, 0.0006438490228505469159 ),
 .UNSPECIFIED. ) ;
#2360 = CARTESIAN_POINT ( 'NONE',  ( 123.7445081442452874, -7.894159318335828068, -9.358103419637847864 ) ) ;
#2361 = VERTEX_POINT ( 'NONE', #31102 ) ;
#2362 = DIRECTION ( 'NONE',  ( 0.000000000000000000, 0.4669533266896289669, 0.8842819633428518067 ) ) ;
#2363 = CARTESIAN_POINT ( 'NONE',  ( 123.4608748109119745, -10.63000616557722466, -14.87417383870573495 ) ) ;
#2364 = CARTESIAN_POINT ( 'NONE',  ( 113.7606148109119886, -7.894159318335828068, -9.358103419637847864 ) ) ;
#2365 = CARTESIAN_POINT ( 'NONE',  ( 126.0703014775786102, -9.988377603198980381, -10.36322818467138518 ) ) ;
#2366 = LINE ( 'NONE', #22448, #1987 ) ;
#2367 = DIRECTION ( 'NONE',  ( 0.000000000000000000, 0.000000000000000000, 1.000000000000000000 ) ) ;
#2368 = ORIENTED_EDGE ( 'NONE', *, *, #32345, .F. ) ;
#2369 = CARTESIAN_POINT ( 'NONE',  ( 128.2184548109119930, -2.520019956603805511, -15.26558354049377009 ) ) ;
#2370 = CARTESIAN_POINT ( 'NONE',  ( 109.4407702545248355, 0.1403307496149616695, -11.32035403202665336 ) ) ;
#2371 = AXIS2_PLACEMENT_3D ( 'NONE', #41951, #5989, #2570 ) ;
#2372 = DIRECTION ( 'NONE',  ( -1.000000000000000000, 0.000000000000000000, 0.000000000000000000 ) ) ;
#2373 = CARTESIAN_POINT ( 'NONE',  ( 118.0151148109119816, 0.4262465694468514643, -12.03445270309931736 ) ) ;
#2374 = CARTESIAN_POINT ( 'NONE',  ( 113.1366214775786432, -7.643976991954077427, -18.09477374809248928 ) ) ;
#2375 = CARTESIAN_POINT ( 'NONE',  ( 126.3858199398357982, -6.059226663227516241, -18.33441212318943769 ) ) ;
#2376 = ORIENTED_EDGE ( 'NONE', *, *, #6085, .T. ) ;
#2377 = CARTESIAN_POINT ( 'NONE',  ( 116.8754296295248025, -4.863998795839590272, -18.39321520033831803 ) ) ;
#2378 = MECHANICAL_DESIGN_GEOMETRIC_PRESENTATION_REPRESENTATION (  '', ( #19877 ), #43182 ) ;
#2379 = CARTESIAN_POINT ( 'NONE',  ( 115.6325948109119821, -9.565557343593413364, -10.61323700422348004 ) ) ;
#2380 = CARTESIAN_POINT ( 'NONE',  ( 113.0798948109119948, -8.899110576539710493, -16.42337572283490132 ) ) ;
#2381 = CONICAL_SURFACE ( 'NONE', #205, 3.999999999999997780, 0.7853981633974476129 ) ;
#2382 = CARTESIAN_POINT ( 'NONE',  ( 61.69189222814998175, -60.36723518915388809, -40.15320052877397217 ) ) ;
#2383 = CARTESIAN_POINT ( 'NONE',  ( 112.0588148109119828, -9.859900752359374465, -12.68260735090039404 ) ) ;
#2385 = CARTESIAN_POINT ( 'NONE',  ( 123.8579614775786126, 0.5811942927096110934, -14.16772938898807510 ) ) ;
#2384 = CARTESIAN_POINT ( 'NONE',  ( 69.87842214007035579, -26.26439233367433346, -5.755590708596306726 ) ) ;
#2386 = CARTESIAN_POINT ( 'NONE',  ( 112.1722681442453222, -0.4660016031367893996, -10.09054647747474043 ) ) ;
#2387 = ORIENTED_EDGE ( 'NONE', *, *, #10017, .F. ) ;
#2388 = CARTESIAN_POINT ( 'NONE',  ( 74.82520252044861309, -48.51951888521425360, -16.39321520033831447 ) ) ;
#2389 = DIRECTION ( 'NONE',  ( 0.000000000000000000, 0.000000000000000000, -1.000000000000000000 ) ) ;
#2390 = CARTESIAN_POINT ( 'NONE',  ( 111.3160046295247838, -4.863998795839590272, -18.39754474579285315 ) ) ;
#2391 = CARTESIAN_POINT ( 'NONE',  ( 123.5743281442453139, -2.084020599724406786, -8.691656652584148546 ) ) ;
#2392 = CARTESIAN_POINT ( 'NONE',  ( 118.3554748109119998, -9.565557343593413364, -10.61323700422348004 ) ) ;
#2393 = CARTESIAN_POINT ( 'NONE',  ( 124.9801526047702538, 2.307970676211291483, -15.90402515948385265 ) ) ;
#2394 = CARTESIAN_POINT ( 'NONE',  ( 114.1635827545248389, -6.936859964151250502, -8.388885654883777576 ) ) ;
#2395 = DIRECTION ( 'NONE',  ( -0.000000000000000000, -0.9284778069183718952, -0.3713878862591649677 ) ) ;
#2396 = LINE ( 'NONE', #31119, #17256 ) ;
#2397 = CARTESIAN_POINT ( 'NONE',  ( 114.6682414775786469, -7.894159318335828068, -9.358103419637847864 ) ) ;
#2398 = CARTESIAN_POINT ( 'NONE',  ( 109.3713171295247832, -10.62599879583958540, -13.39321520033831447 ) ) ;
#2399 = FACE_OUTER_BOUND ( 'NONE', #27872, .T. ) ;
#2400 = CARTESIAN_POINT ( 'NONE',  ( 112.7050671295247923, -10.62599879583958540, -13.39321520033831447 ) ) ;
#2401 = CARTESIAN_POINT ( 'NONE',  ( 121.5321681442453183, -9.988377603198976828, -10.36322818467138340 ) ) ;
#2402 = CARTESIAN_POINT ( 'NONE',  ( 123.3474214775786209, -9.988377603198976828, -10.36322818467138340 ) ) ;
#2403 = CARTESIAN_POINT ( 'NONE',  ( 115.3442858795247759, -0.7896495226426338832, -17.46756447353520159 ) ) ;
#2404 = CARTESIAN_POINT ( 'NONE',  ( 118.0718414775786300, -9.261995988541697145, -16.69588392320189030 ) ) ;
#2405 = CARTESIAN_POINT ( 'NONE',  ( 114.4413348109119823, -9.261995988541697145, -16.69588392320189030 ) ) ;
#2406 = ORIENTED_EDGE ( 'NONE', *, *, #30337, .T. ) ;
#2407 = CARTESIAN_POINT ( 'NONE',  ( 113.7606148109119886, -7.894159318335828068, -9.358103419637847864 ) ) ;
#2408 = CIRCLE ( 'NONE', #38821, 20.00000000000000355 ) ;
#2409 = CARTESIAN_POINT ( 'NONE',  ( 112.1722681442453222, -8.899110576539710493, -16.42337572283490132 ) ) ;
#2410 = CARTESIAN_POINT ( 'NONE',  ( 121.9859814775786333, 0.2603800115204892296, -16.42320221600525088 ) ) ;
#2411 = CARTESIAN_POINT ( 'NONE',  ( 124.9357681442453014, -7.643976991954077427, -18.09477374809248928 ) ) ;
#2412 = CONTEXT_DEPENDENT_SHAPE_REPRESENTATION ( #34663, #39059 ) ;
#2413 = CARTESIAN_POINT ( 'NONE',  ( 112.4559014775786778, -0.1624402480850797581, -16.17319339645315424 ) ) ;
#2414 = ORIENTED_EDGE ( 'NONE', *, *, #17247, .F. ) ;
#2415 = CARTESIAN_POINT ( 'NONE',  ( 119.2631014775786298, -9.565557343593413364, -10.61323700422348004 ) ) ;
#2416 = CARTESIAN_POINT ( 'NONE',  ( 126.1837548109119211, -10.63000616557722466, -14.87417383870573495 ) ) ;
#2417 = ADVANCED_FACE ( 'NONE', ( #37252 ), #6264, .F. ) ;
#2418 = CARTESIAN_POINT ( 'NONE',  ( 107.7044421295247929, 0.8980012041604618078, -13.39321520033831447 ) ) ;
#2419 = AXIS2_PLACEMENT_3D ( 'NONE', #34160, #31634, #16861 ) ;
#2420 = CARTESIAN_POINT ( 'NONE',  ( 119.4900081442453086, -7.643976991954077427, -18.09477374809248928 ) ) ;
#2421 = CARTESIAN_POINT ( 'NONE',  ( 70.19189222814998175, -50.76020450571126474, -33.50691401458669105 ) ) ;
#2422 = CARTESIAN_POINT ( 'NONE',  ( 124.2558810407382026, -2.419733177069661512, -17.89711025544711376 ) ) ;
#2423 = ORIENTED_EDGE ( 'NONE', *, *, #5411, .T. ) ;
#2424 = CARTESIAN_POINT ( 'NONE',  ( 123.3550173109119612, -9.289237151508434209, -11.05642687123711276 ) ) ;
#2425 = EDGE_CURVE ( 'NONE', #6914, #43250, #15665, .T. ) ;
#2426 = CARTESIAN_POINT ( 'NONE',  ( 123.9714148109119805, -0.4660016031367893996, -10.09054647747474043 ) ) ;
#2427 = CARTESIAN_POINT ( 'NONE',  ( 85.82015659721905365, -25.99489077589524300, -13.39321520033831625 ) ) ;
#2428 = DIRECTION ( 'NONE',  ( -0.2768435750659263839, -0.3568721902840676363, 0.8921882507333129819 ) ) ;
#2429 = CARTESIAN_POINT ( 'NONE',  ( 122.8688454359119646, -11.07370829466463391, -12.81314460846528469 ) ) ;
#2430 = LINE ( 'NONE', #16817, #23110 ) ;
#2431 = CARTESIAN_POINT ( 'NONE',  ( 107.2877233795247776, -1.325403438956436419, -9.854619843455211026 ) ) ;
#2432 = CARTESIAN_POINT ( 'NONE',  ( 121.7575954359119521, -11.07370829466463569, -12.81314460846529002 ) ) ;
#2433 = AXIS2_PLACEMENT_3D ( 'NONE', #12240, #12014, #36382 ) ;
#2434 = CARTESIAN_POINT ( 'NONE',  ( 137.3593431606284696, -4.917112010162052016, -18.55357672982330541 ) ) ;
#2435 = CIRCLE ( 'NONE', #27952, 3.000000000000003997 ) ;
#2436 = CARTESIAN_POINT ( 'NONE',  ( 125.1088394146763818, -2.481781793725739593, -17.81448324536422234 ) ) ;
#2437 = CARTESIAN_POINT ( 'NONE',  ( 125.2761281442453054, -10.63000616557722466, -14.87417383870573495 ) ) ;
#2438 = CARTESIAN_POINT ( 'NONE',  ( 118.9794681442453026, -0.8288870151387760510, -10.36305467784173118 ) ) ;
#2439 = CARTESIAN_POINT ( 'NONE',  ( 119.7434548109119703, 0.2385497399887595849, -14.97457365435098886 ) ) ;
#2440 = EDGE_CURVE ( 'NONE', #5770, #22762, #42644, .T. ) ;
#2441 = VERTEX_POINT ( 'NONE', #30434 ) ;
#2442 = CARTESIAN_POINT ( 'NONE',  ( 124.3117748109119844, -10.30919188438810075, -12.61870101168855918 ) ) ;
#2443 = CARTESIAN_POINT ( 'NONE',  ( 115.7460481442453357, 0.9020085738987339008, -11.91225656197089222 ) ) ;
#2444 = CARTESIAN_POINT ( 'NONE',  ( 115.1359265045248605, -2.791137627527939813, -8.388885654883777576 ) ) ;
#2445 = CARTESIAN_POINT ( 'NONE',  ( 113.5904348109119866, -7.893985811506177619, -18.51759400769804742 ) ) ;
#2446 = ADVANCED_FACE ( 'NONE', ( #23836 ), #34069, .T. ) ;
#2447 = EDGE_CURVE ( 'NONE', #41822, #12164, #16995, .T. ) ;
#2448 = CARTESIAN_POINT ( 'NONE',  ( 125.0492214775786266, -3.505236298600246325, -18.68346056562440793 ) ) ;
#2449 = CARTESIAN_POINT ( 'NONE',  ( 123.5743281442453139, -7.893985811506177619, -18.51759400769804742 ) ) ;
#2450 = CARTESIAN_POINT ( 'NONE',  ( 114.2330358795247776, -0.7896495226426338832, -17.46756447353520159 ) ) ;
#2451 = CARTESIAN_POINT ( 'NONE',  ( 110.2047546295247855, -4.863998795839590272, -18.39754474579285315 ) ) ;
#2452 = CARTESIAN_POINT ( 'NONE',  ( 115.4056881442453459, -2.084020599724406786, -8.691656652584148546 ) ) ;
#2453 = CARTESIAN_POINT ( 'NONE',  ( 117.2776681442452968, -4.153390946401325223, -8.397313243818185668 ) ) ;
#2454 = CARTESIAN_POINT ( 'NONE',  ( 66.82415148905926117, -40.21211973637273474, -4.893215200338314474 ) ) ;
#2455 = CARTESIAN_POINT ( 'NONE',  ( 114.5803015045248117, -6.936859964151250502, -18.39754474579286025 ) ) ;
#2456 = ORIENTED_EDGE ( 'NONE', *, *, #43751, .F. ) ;
#2457 = CARTESIAN_POINT ( 'NONE',  ( 109.2294786918755278, -0.01490074043973391681, -15.03572518876057806 ) ) ;
#2458 = CARTESIAN_POINT ( 'NONE',  ( 124.9924948109119924, -5.574606645277164318, -18.38911715685844683 ) ) ;
#2459 = CARTESIAN_POINT ( 'NONE',  ( 122.4521266859119635, -0.06289925094097943703, -9.412459353600674206 ) ) ;
#2460 = CARTESIAN_POINT ( 'NONE',  ( 119.1878298109119783, -7.200787124940443817, -17.81845355600750835 ) ) ;
#2461 = ORIENTED_EDGE ( 'NONE', *, *, #33475, .F. ) ;
#2462 = DIRECTION ( 'NONE',  ( 1.000000000000000000, 0.000000000000000000, 0.000000000000000000 ) ) ;
#2463 = CARTESIAN_POINT ( 'NONE',  ( 117.0819916265821661, -11.36549209999471266, -21.70826808144084907 ) ) ;
#2464 = ORIENTED_EDGE ( 'NONE', *, *, #34499, .F. ) ;
#2465 = CARTESIAN_POINT ( 'NONE',  ( 116.8805814775786445, -6.344957434206662583, -7.627207830600332805 ) ) ;
#2466 = CARTESIAN_POINT ( 'NONE',  ( 124.5954081442453116, -6.222761293078241884, -8.102969835052219238 ) ) ;
#2467 = CARTESIAN_POINT ( 'NONE',  ( 115.1220548109119761, -1.833838273342658809, -17.42832698103878286 ) ) ;
#2468 = CARTESIAN_POINT ( 'NONE',  ( 112.1260814775786514, -8.862178061932382889, -16.39564131203247399 ) ) ;
#2469 = CARTESIAN_POINT ( 'NONE',  ( 121.9292548109119849, -1.561330072975668948, -17.79121239304076951 ) ) ;
#2470 = CARTESIAN_POINT ( 'NONE',  ( 114.8951481442453115, -0.4660016031367893996, -10.09054647747474043 ) ) ;
#2471 = VECTOR ( 'NONE', #41331, 1000.000000000000000 ) ;
#2472 = EDGE_CURVE ( 'NONE', #1202, #29255, #30661, .T. ) ;
#2473 = CARTESIAN_POINT ( 'NONE',  ( 112.3578015045248861, -6.936859964151250502, -18.39754474579286025 ) ) ;
#2474 = CARTESIAN_POINT ( 'NONE',  ( 125.7866681442452688, -0.4660016031367893996, -10.09054647747474043 ) ) ;
#2475 = LINE ( 'NONE', #16400, #43937 ) ;
#2476 = ORIENTED_EDGE ( 'NONE', *, *, #22496, .T. ) ;
#2477 = CARTESIAN_POINT ( 'NONE',  ( 116.3700414775786527, -5.638512984488999180, -18.83840828888717311 ) ) ;
#2478 = CARTESIAN_POINT ( 'NONE',  ( 115.3489614775786407, -0.8288870151387760510, -10.36305467784173118 ) ) ;
#2479 = LINE ( 'NONE', #40116, #8942 ) ;
#2480 = EDGE_CURVE ( 'NONE', #17949, #13081, #30990, .T. ) ;
#2481 = CARTESIAN_POINT ( 'NONE',  ( 126.5808414775786446, -9.859900752359378018, -12.68260735090039759 ) ) ;
#2482 = ORIENTED_EDGE ( 'NONE', *, *, #5224, .F. ) ;
#2483 = CARTESIAN_POINT ( 'NONE',  ( 120.9649014775786355, -3.383040157471821630, -19.15922257007629170 ) ) ;
#2484 = CARTESIAN_POINT ( 'NONE',  ( 115.9294421295247872, 1.035107641088057973, -4.893215200338314474 ) ) ;
#2485 = CARTESIAN_POINT ( 'NONE',  ( 120.2510376736034345, -8.245233026025740486, -17.07659070123625256 ) ) ;
#2486 = CARTESIAN_POINT ( 'NONE',  ( 125.0876622310133399, -1.244021962887375432, -16.96476564598603431 ) ) ;
#2487 = CARTESIAN_POINT ( 'NONE',  ( 116.8238548109119819, -5.574606645277164318, -18.38911715685844683 ) ) ;
#2488 = CARTESIAN_POINT ( 'NONE',  ( 112.4960109814547309, -2.395992375830773291, -17.92872468182854462 ) ) ;
#2489 = CARTESIAN_POINT ( 'NONE',  ( 117.8449348109119938, -1.833838273342659253, -17.42832698103878286 ) ) ;
#2490 = DIRECTION ( 'NONE',  ( 0.9498278979187092519, 0.3127730236694430399, -0.000000000000000000 ) ) ;
#2491 = CARTESIAN_POINT ( 'NONE',  ( 125.3245149615581653, -2.345172624729188193, -20.05245885555360630 ) ) ;
#2492 = CARTESIAN_POINT ( 'NONE',  ( 115.9162281442453093, -5.574606645277164318, -18.38911715685844683 ) ) ;
#2493 = CARTESIAN_POINT ( 'NONE',  ( 117.2776681442452968, -5.638512984488999180, -18.83840828888717311 ) ) ;
#2494 = CARTESIAN_POINT ( 'NONE',  ( 123.1466579359119891, -4.360204210389833968, -8.000047426360245240 ) ) ;
#2495 = CARTESIAN_POINT ( 'NONE',  ( 125.6164881442453094, -9.565557343593413364, -10.61323700422348004 ) ) ;
#2496 = CARTESIAN_POINT ( 'NONE',  ( 114.3846081442453197, 0.4262465694468514643, -12.03445270309931736 ) ) ;
#2497 = CARTESIAN_POINT ( 'NONE',  ( 122.2696148109119889, -4.089484607189486809, -7.948022111789456723 ) ) ;
#2498 = EDGE_CURVE ( 'NONE', #31245, #40595, #41393, .T. ) ;
#2499 = CIRCLE ( 'NONE', #1781, 2.000000000000000444 ) ;
#2500 = CARTESIAN_POINT ( 'NONE',  ( 121.3619881442452879, -4.089484607189486809, -7.948022111789456723 ) ) ;
#2501 = EDGE_LOOP ( 'NONE', ( #40934, #44267, #8046, #3100, #36010, #17499 ) ) ;
#2502 = CARTESIAN_POINT ( 'NONE',  ( 114.3278814775786429, -10.30919188438810075, -12.61870101168855918 ) ) ;
#2503 = CARTESIAN_POINT ( 'NONE',  ( 112.2883483795247770, -0.7896495226426338832, -9.318865927141430916 ) ) ;
#2504 = DIRECTION ( 'NONE',  ( 1.000000000000000000, 0.000000000000000000, -0.000000000000000000 ) ) ;
#2505 = CARTESIAN_POINT ( 'NONE',  ( 106.3848327545248651, -6.936859964151250502, -8.388885654883777576 ) ) ;
#2506 = CARTESIAN_POINT ( 'NONE',  ( 128.0593593558783425, -4.017378915256145433, -15.76970282473099516 ) ) ;
#2507 = CARTESIAN_POINT ( 'NONE',  ( 119.3765548109119834, 0.9020085738987339008, -11.91225656197089222 ) ) ;
#2508 = EDGE_LOOP ( 'NONE', ( #30104, #14540, #30555, #36508, #31890 ) ) ;
#2509 = CARTESIAN_POINT ( 'NONE',  ( -3.429934629567074733, -4.841764211284793618, -19.39321520033831447 ) ) ;
#2510 = LINE ( 'NONE', #19852, #8131 ) ;
#2511 = EDGE_CURVE ( 'NONE', #32422, #8854, #20847, .T. ) ;
#2512 = CARTESIAN_POINT ( 'NONE',  ( 114.7249681442453237, -9.565557343593413364, -10.61323700422348004 ) ) ;
#2513 = CARTESIAN_POINT ( 'NONE',  ( 123.1676081739442878, -4.756192495830094735, -19.39047411591439740 ) ) ;
#2514 = CARTESIAN_POINT ( 'NONE',  ( 119.2063748109119814, -1.561330072975668504, -17.79121239304076951 ) ) ;
#2515 = CARTESIAN_POINT ( 'NONE',  ( 107.5655358795247736, -0.7896495226426338832, -17.46756447353520159 ) ) ;
#2516 = DIRECTION ( 'NONE',  ( 0.2768435750659241079, 0.3568721902840695792, -0.8921882507333129819 ) ) ;
#2517 = VERTEX_POINT ( 'NONE', #9923 ) ;
#2518 = CARTESIAN_POINT ( 'NONE',  ( 93.44708369096697709, -23.96159667187537679, -12.55314669922780979 ) ) ;
#2519 = CARTESIAN_POINT ( 'NONE',  ( 123.8012348109119642, -9.565557343593413364, -10.61323700422348004 ) ) ;
#2520 = CARTESIAN_POINT ( 'NONE',  ( 121.1918081442452859, 0.9020085738987339008, -11.91225656197089222 ) ) ;
#2521 = CARTESIAN_POINT ( 'NONE',  ( 113.2500748109119968, -3.505236298600246325, -18.68346056562440793 ) ) ;
#2522 = CARTESIAN_POINT ( 'NONE',  ( 114.4980614775786592, -7.893985811506177619, -18.51759400769804742 ) ) ;
#2523 = CARTESIAN_POINT ( 'NONE',  ( 118.7315769107182177, -2.467220198592778413, -17.83387418641524391 ) ) ;
#2524 = CARTESIAN_POINT ( 'NONE',  ( 126.5010429760475574, -1.163263821645348584, -9.824252222897710496 ) ) ;
#2525 = CARTESIAN_POINT ( 'NONE',  ( 118.3554748109119998, -9.565557343593413364, -10.61323700422348004 ) ) ;
#2526 = VERTEX_POINT ( 'NONE', #6721 ) ;
#2527 = VECTOR ( 'NONE', #45030, 1000.000000000000000 ) ;
#2528 = CARTESIAN_POINT ( 'NONE',  ( 120.0465871478583466, -3.807985514183269693, -19.09877912889401230 ) ) ;
#2529 = CARTESIAN_POINT ( 'NONE',  ( 112.9664414775786412, 0.5811942927096154232, -14.16772938898807155 ) ) ;
#2530 = CARTESIAN_POINT ( 'NONE',  ( 121.8158014775786171, -4.153390946401325223, -8.397313243818185668 ) ) ;
#2531 = VERTEX_POINT ( 'NONE', #37723 ) ;
#2532 = CARTESIAN_POINT ( 'NONE',  ( 122.1048610609119720, -6.340755971794695078, -8.611740276972781771 ) ) ;
#2533 = CARTESIAN_POINT ( 'NONE',  ( 118.9794681442453026, -9.261995988541697145, -16.69588392320189030 ) ) ;
#2534 = VECTOR ( 'NONE', #27301, 1000.000000000000000 ) ;
#2535 = CARTESIAN_POINT ( 'NONE',  ( 113.2606921295247702, 0.8980012041604618078, -13.39321520033831447 ) ) ;
#2536 = CARTESIAN_POINT ( 'NONE',  ( 116.5969481442453031, -9.859900752359374465, -12.68260735090039404 ) ) ;
#2537 = ORIENTED_EDGE ( 'NONE', *, *, #43419, .T. ) ;
#2538 = VERTEX_POINT ( 'NONE', #20632 ) ;
#2539 = CARTESIAN_POINT ( 'NONE',  ( 112.0588148109119828, 0.5811942927096154232, -14.16772938898807155 ) ) ;
#2540 = CARTESIAN_POINT ( 'NONE',  ( 121.7023481442452777, -0.8288870151387760510, -10.36305467784173118 ) ) ;
#2541 = CARTESIAN_POINT ( 'NONE',  ( 85.43169907558235820, -25.99489077589524300, -13.39321520033831625 ) ) ;
#2542 = EDGE_CURVE ( 'NONE', #17, #4318, #3287, .T. ) ;
#2543 = FACE_BOUND ( 'NONE', #6617, .T. ) ;
#2544 = CARTESIAN_POINT ( 'NONE',  ( 118.4689281442453392, 0.9020085738987339008, -11.91225656197089222 ) ) ;
#2545 = CARTESIAN_POINT ( 'NONE',  ( 107.7044421295247929, 0.8980012041604618078, -13.39321520033831447 ) ) ;
#2546 = CARTESIAN_POINT ( 'NONE',  ( 119.0929214775786278, -5.638512984488999180, -18.83840828888717311 ) ) ;
#2548 = CARTESIAN_POINT ( 'NONE',  ( 118.8660148109119774, 0.1319031606808879209, -14.10382304977623669 ) ) ;
#2547 = CARTESIAN_POINT ( 'NONE',  ( 114.5547881442453217, -5.638512984488999180, -18.83840828888717311 ) ) ;
#2549 = CARTESIAN_POINT ( 'NONE',  ( 124.7088614775786226, -9.565557343593413364, -10.61323700422348004 ) ) ;
#2550 = CARTESIAN_POINT ( 'NONE',  ( 112.0588148109119828, 0.5811942927096154232, -14.16772938898807155 ) ) ;
#2551 = EDGE_LOOP ( 'NONE', ( #41096, #23934, #17870, #2088, #22809, #24035, #12080, #11391, #41619, #30442, #23287, #13989, #19282, #24260, #14132, #38624, #4393, #15346, #42865 ) ) ;
#2552 = CARTESIAN_POINT ( 'NONE',  ( 125.1626748109119802, -0.1624402480850797581, -16.17319339645315424 ) ) ;
#2553 = CARTESIAN_POINT ( 'NONE',  ( 70.19189222814998175, -55.40259354030312267, -35.36385344588251911 ) ) ;
#2554 = CARTESIAN_POINT ( 'NONE',  ( 135.3184548109119874, -9.609004340414083245, -9.721032963308941177 ) ) ;
#2555 = AXIS2_PLACEMENT_3D ( 'NONE', #12768, #9114, #15276 ) ;
#2556 = CARTESIAN_POINT ( 'NONE',  ( 110.4825671295247815, -10.62599879583958540, -13.39321520033831447 ) ) ;
#2557 = CARTESIAN_POINT ( 'NONE',  ( 115.4831921295247952, -9.868328341294093420, -13.39321520033831447 ) ) ;
#2558 = CARTESIAN_POINT ( 'NONE',  ( 111.3854577545248645, -7.250697342233347165, -7.631215200338321125 ) ) ;
#2559 = EDGE_CURVE ( 'NONE', #20329, #10520, #3509, .T. ) ;
#2560 = CARTESIAN_POINT ( 'NONE',  ( 122.5532481442453019, -10.63000616557722466, -14.87417383870573495 ) ) ;
#2561 = CARTESIAN_POINT ( 'NONE',  ( 123.1205148109119563, -7.643976991954077427, -18.09477374809248928 ) ) ;
#2562 = ORIENTED_EDGE ( 'NONE', *, *, #42601, .F. ) ;
#2563 = CARTESIAN_POINT ( 'NONE',  ( 125.1059481442452750, -8.166667518702819706, -8.995218007635861213 ) ) ;
#2564 = CARTESIAN_POINT ( 'NONE',  ( 113.9307948109119764, -10.15424416112533912, -14.75197769757731336 ) ) ;
#2565 = DIRECTION ( 'NONE',  ( 0.5735764363510499342, 0.3127926500124801890, -0.7570804645221008711 ) ) ;
#2566 = CARTESIAN_POINT ( 'NONE',  ( 121.1918081442452859, 0.9020085738987339008, -11.91225656197089222 ) ) ;
#2567 = CARTESIAN_POINT ( 'NONE',  ( 122.6099748109119929, -9.261995988541697145, -16.69588392320189030 ) ) ;
#2568 = CARTESIAN_POINT ( 'NONE',  ( 67.30914723170953096, -56.74361331656334784, -36.79476457314395788 ) ) ;
#2569 = CARTESIAN_POINT ( 'NONE',  ( 124.2550481442452792, -0.1624402480850797581, -16.17319339645315424 ) ) ;
#2570 = DIRECTION ( 'NONE',  ( -1.000000000000000000, 0.000000000000000000, 0.000000000000000000 ) ) ;
#2571 = DIRECTION ( 'NONE',  ( -0.7871354856660162103, -0.4483307682966942709, -0.4235767337848251879 ) ) ;
#2572 = VERTEX_POINT ( 'NONE', #27921 ) ;
#2573 = CARTESIAN_POINT ( 'NONE',  ( -2.615402842485104351, -7.069279208319384722, -7.472031487140878170 ) ) ;
#2574 = CARTESIAN_POINT ( 'NONE',  ( 112.5693548109119888, 0.4262465694468514643, -12.03445270309931736 ) ) ;
#2575 = CARTESIAN_POINT ( 'NONE',  ( 125.0492214775786266, -3.505236298600246325, -18.68346056562440793 ) ) ;
#2576 = CARTESIAN_POINT ( 'NONE',  ( 107.7044421295247929, -9.868328341294093420, -13.39321520033831447 ) ) ;
#2577 = CARTESIAN_POINT ( 'NONE',  ( 110.2047546295247855, -4.863998795839590272, -18.39754474579285315 ) ) ;
#2578 = CARTESIAN_POINT ( 'NONE',  ( 117.4478481442453131, -9.565557343593413364, -10.61323700422348004 ) ) ;
#2579 = CARTESIAN_POINT ( 'NONE',  ( 70.05034961234838420, -25.59043224118723714, -5.724109476187135392 ) ) ;
#2580 = CARTESIAN_POINT ( 'NONE',  ( 115.8027748109119841, -8.899110576539710493, -16.42337572283490132 ) ) ;
#2581 = CARTESIAN_POINT ( 'NONE',  ( 123.1772414775786189, -4.089484607189486809, -7.948022111789456723 ) ) ;
#2582 = VERTEX_POINT ( 'NONE', #1589 ) ;
#2583 = CARTESIAN_POINT ( 'NONE',  ( 121.3619881442452879, -5.574606645277164318, -18.38911715685844683 ) ) ;
#2584 = CARTESIAN_POINT ( 'NONE',  ( 118.0718414775786300, -9.261995988541697145, -16.69588392320189030 ) ) ;
#2585 = CARTESIAN_POINT ( 'NONE',  ( 123.9714148109119805, -0.4660016031367893996, -10.09054647747474043 ) ) ;
#2586 = CARTESIAN_POINT ( 'NONE',  ( 124.1415948109119540, -3.505236298600246325, -18.68346056562440793 ) ) ;
#2587 = VERTEX_POINT ( 'NONE', #32603 ) ;
#2588 = DIRECTION ( 'NONE',  ( 1.000000000000000000, 0.000000000000000000, -0.000000000000000000 ) ) ;
#2589 =( BOUNDED_SURFACE ( )  B_SPLINE_SURFACE ( 1, 2, ( 
 ( #32387, #25114, #36255, #4572, #18040, #1597, #1155, #31935, #15291, #701, #18719, #11880, #15072, #39236, #8000, #39010, #28761, #14621, #28984, #28538, #18268, #21689, #11210, #32163, #1377, #36029, #42444, #29200, #43110, #39691, #25559, #5022, #18938, #32826, #29424, #24883, #15747, #26011, #33495, #2730, #16656, #2050, #44254, #37147, #40367, #29649, #33276, #15974, #5922, #33046, #19844, #43793, #9355, #5248, #30106, #29877, #33732, #44022, #9584, #19166, #40141, #9131, #2503, #23034, #16430, #36922, #37386, #30326, #13010, #12558, #43338, #26909, #19387, #40829, #40597, #23500, #6158, #5692, #20077, #33962, #19611, #26464, #12107, #39915, #43563, #36699, #2273, #16203, #12783, #8905, #8677, #26686, #22580, #12332, #23265, #1820, #36481, #26232, #22803, #5467, #37618, #38061, #6839, #23728, #41942, #24169, #28035, #24387, #41507, #10705, #38273, #10049, #7054, #20965, #16886, #34837, #3185, #20745, #44703, #24608, #34624, #41061, #21183, #10262, #27138, #3622, #9818, #17542, #31435, #3410, #44926, #13685, #13464, #17110, #6392, #17327, #2959, #23953, #27366, #30778, #41287, #202, #27806, #37834, #14118, #38491, #7266, #6612, #35060, #27594, #20299, #20524, #31000, #34404, #13236, #31217, #3841, #30550, #45143, #44471, #34185 ),
 ( #13900, #41721, #10485, #25058, #17761, #4061, #25734, #31885, #11152, #1103, #35975, #4524, #14342, #15020, #14565, #1326, #38719, #15238, #39414, #35288, #28484, #35519, #11378, #18447, #31658, #28256, #11827, #42388, #28708, #8177, #14794, #22087, #25284, #39641, #42165, #426, #42615, #24828, #8405, #28931, #42838, #25509, #11599, #7944, #22309, #4746, #18666, #4291, #36205, #32559, #38951, #29147, #43060, #10926, #7490, #39180, #21407, #17985, #21855, #7718, #650, #21631, #18210, #32108, #35751, #32336, #875, #1770, #1547, #12509, #23214, #5194, #2000, #8629, #5867, #32773, #22749, #26405, #12056, #40315, #9079, #43285, #16371, #43739, #2451, #43965, #15926, #30274, #12729, #29598, #26632, #40545, #36425, #9306, #36650, #22982, #19112, #44199, #36871, #15468, #40770, #29823, #29374, #37093, #25957, #19790, #33673, #5641, #19340, #33225, #32996, #5423, #39864, #19562, #22529, #43515, #15696, #12284, #26180, #12961, #2218, #40088, #26857, #9528, #23444, #8849, #4972, #33439, #16148, #30052, #18882, #9762, #20020, #27541, #41892, #10653, #41232, #38225, #31169, #34355, #23673, #27315, #9992, #45090, #27087, #13846, #37784, #3359, #44418, #24119, #23901, #27761, #38013, #3574, #13184, #2673, #41676, #17058, #10434, #16833, #16605 ) ),
 .UNSPECIFIED., .F., .F., .T. ) 
 B_SPLINE_SURFACE_WITH_KNOTS ( ( 2, 2 ),
 ( 3, 2, 2, 2, 2, 2, 2, 2, 2, 2, 2, 2, 2, 2, 2, 2, 2, 2, 2, 2, 2, 2, 2, 2, 2, 2, 2, 2, 2, 2, 2, 2, 2, 2, 2, 2, 2, 2, 2, 2, 2, 2, 2, 2, 2, 2, 2, 2, 2, 2, 2, 2, 2, 2, 2, 2, 2, 2, 2, 2, 2, 2, 2, 2, 2, 2, 2, 2, 2, 2, 2, 2, 2, 2, 2, 2, 2, 2, 2, 2, 3 ),
 ( 0.000000000000000000, 1.000000000000000000 ),
 ( 0.000000000000000000, 0.01250000000000000069, 0.02500000000000000139, 0.03749999999999999861, 0.05000000000000000278, 0.06250000000000000000, 0.07499999999999999722, 0.08749999999999999445, 0.1000000000000000056, 0.1125000000000000028, 0.1250000000000000000, 0.1375000000000000111, 0.1499999999999999944, 0.1625000000000000056, 0.1749999999999999889, 0.1875000000000000000, 0.2000000000000000111, 0.2124999999999999944, 0.2250000000000000056, 0.2374999999999999889, 0.2500000000000000000, 0.2625000000000000111, 0.2750000000000000222, 0.2874999999999999778, 0.2999999999999999889, 0.3125000000000000000, 0.3250000000000000111, 0.3375000000000000222, 0.3499999999999999778, 0.3624999999999999889, 0.3750000000000000000, 0.3875000000000000111, 0.4000000000000000222, 0.4124999999999999778, 0.4249999999999999889, 0.4375000000000000000, 0.4500000000000000111, 0.4625000000000000222, 0.4749999999999999778, 0.4874999999999999889, 0.5000000000000000000, 0.5124999999999999556, 0.5250000000000000222, 0.5374999999999999778, 0.5500000000000000444, 0.5625000000000000000, 0.5749999999999999556, 0.5875000000000000222, 0.5999999999999999778, 0.6125000000000000444, 0.6250000000000000000, 0.6374999999999999556, 0.6500000000000000222, 0.6624999999999999778, 0.6750000000000000444, 0.6875000000000000000, 0.6999999999999999556, 0.7125000000000000222, 0.7249999999999999778, 0.7375000000000000444, 0.7500000000000000000, 0.7624999999999999556, 0.7750000000000000222, 0.7874999999999999778, 0.8000000000000000444, 0.8125000000000000000, 0.8249999999999999556, 0.8375000000000000222, 0.8499999999999999778, 0.8625000000000000444, 0.8750000000000000000, 0.8874999999999999556, 0.9000000000000000222, 0.9124999999999999778, 0.9250000000000000444, 0.9375000000000000000, 0.9499999999999999556, 0.9625000000000000222, 0.9749999999999999778, 0.9875000000000000444, 1.000000000000000000 ),
 .UNSPECIFIED. ) 
 GEOMETRIC_REPRESENTATION_ITEM ( )  RATIONAL_B_SPLINE_SURFACE ( (
 ( 1.000000000000000000, 0.9238795325112869605, 1.000000000000000000, 0.9238795325112869605, 1.000000000000000000, 0.9238795325112869605, 1.000000000000000000, 0.9238795325112869605, 1.000000000000000000, 0.9238795325112869605, 1.000000000000000000, 0.9238795325112869605, 1.000000000000000000, 0.9238795325112869605, 1.000000000000000000, 0.9238795325112869605, 1.000000000000000000, 0.9238795325112869605, 1.000000000000000000, 0.9238795325112869605, 1.000000000000000000, 0.9238795325112869605, 1.000000000000000000, 0.9238795325112869605, 1.000000000000000000, 0.9238795325112869605, 1.000000000000000000, 0.9238795325112869605, 1.000000000000000000, 0.9238795325112869605, 1.000000000000000000, 0.9238795325112869605, 1.000000000000000000, 0.9238795325112869605, 1.000000000000000000, 0.9238795325112869605, 1.000000000000000000, 0.9238795325112869605, 1.000000000000000000, 0.9238795325112869605, 1.000000000000000000, 0.9238795325112869605, 1.000000000000000000, 0.9238795325112869605, 1.000000000000000000, 0.9238795325112869605, 1.000000000000000000, 0.9238795325112869605, 1.000000000000000000, 0.9238795325112869605, 1.000000000000000000, 0.9238795325112869605, 1.000000000000000000, 0.9238795325112869605, 1.000000000000000000, 0.9238795325112869605, 1.000000000000000000, 0.9238795325112869605, 1.000000000000000000, 0.9238795325112869605, 1.000000000000000000, 0.9238795325112869605, 1.000000000000000000, 0.9238795325112869605, 1.000000000000000000, 0.9238795325112869605, 1.000000000000000000, 0.9238795325112869605, 1.000000000000000000, 0.9238795325112869605, 1.000000000000000000, 0.9238795325112869605, 1.000000000000000000, 0.9238795325112869605, 1.000000000000000000, 0.9238795325112869605, 1.000000000000000000, 0.9238795325112869605, 1.000000000000000000, 0.9238795325112869605, 1.000000000000000000, 0.9238795325112869605, 1.000000000000000000, 0.9238795325112869605, 1.000000000000000000, 0.9238795325112869605, 1.000000000000000000, 0.9238795325112869605, 1.000000000000000000, 0.9238795325112869605, 1.000000000000000000, 0.9238795325112869605, 1.000000000000000000, 0.9238795325112869605, 1.000000000000000000, 0.9238795325112869605, 1.000000000000000000, 0.9238795325112869605, 1.000000000000000000, 0.9238795325112869605, 1.000000000000000000, 0.9238795325112869605, 1.000000000000000000, 0.9238795325112869605, 1.000000000000000000, 0.9238795325112869605, 1.000000000000000000, 0.9238795325112869605, 1.000000000000000000, 0.9238795325112869605, 1.000000000000000000, 0.9238795325112869605, 1.000000000000000000, 0.9238795325112869605, 1.000000000000000000, 0.9238795325112869605, 1.000000000000000000, 0.9238795325112869605, 1.000000000000000000, 0.9238795325112869605, 1.000000000000000000, 0.9238795325112869605, 1.000000000000000000, 0.9238795325112869605, 1.000000000000000000, 0.9238795325112869605, 1.000000000000000000, 0.9238795325112869605, 1.000000000000000000, 0.9238795325112869605, 1.000000000000000000, 0.9238795325112869605, 1.000000000000000000, 0.9238795325112869605, 1.000000000000000000, 0.9238795325112869605, 1.000000000000000000, 0.9238795325112869605, 1.000000000000000000, 0.9238795325112869605, 1.000000000000000000, 0.9238795325112869605, 1.000000000000000000, 0.9238795325112869605, 1.000000000000000000, 0.9238795325112869605, 1.000000000000000000, 0.9238795325112869605, 1.000000000000000000, 0.9238795325112869605, 1.000000000000000000, 0.9238795325112869605, 1.000000000000000000, 0.9238795325112869605, 1.000000000000000000, 0.9238795325112869605, 1.000000000000000000, 0.9238795325112869605, 1.000000000000000000, 0.9238795325112869605, 1.000000000000000000),
 ( 1.000000000000000000, 0.9238795325112869605, 1.000000000000000000, 0.9238795325112869605, 1.000000000000000000, 0.9238795325112869605, 1.000000000000000000, 0.9238795325112869605, 1.000000000000000000, 0.9238795325112869605, 1.000000000000000000, 0.9238795325112869605, 1.000000000000000000, 0.9238795325112869605, 1.000000000000000000, 0.9238795325112869605, 1.000000000000000000, 0.9238795325112869605, 1.000000000000000000, 0.9238795325112869605, 1.000000000000000000, 0.9238795325112869605, 1.000000000000000000, 0.9238795325112869605, 1.000000000000000000, 0.9238795325112869605, 1.000000000000000000, 0.9238795325112869605, 1.000000000000000000, 0.9238795325112869605, 1.000000000000000000, 0.9238795325112869605, 1.000000000000000000, 0.9238795325112869605, 1.000000000000000000, 0.9238795325112869605, 1.000000000000000000, 0.9238795325112869605, 1.000000000000000000, 0.9238795325112869605, 1.000000000000000000, 0.9238795325112869605, 1.000000000000000000, 0.9238795325112869605, 1.000000000000000000, 0.9238795325112869605, 1.000000000000000000, 0.9238795325112869605, 1.000000000000000000, 0.9238795325112869605, 1.000000000000000000, 0.9238795325112869605, 1.000000000000000000, 0.9238795325112869605, 1.000000000000000000, 0.9238795325112869605, 1.000000000000000000, 0.9238795325112869605, 1.000000000000000000, 0.9238795325112869605, 1.000000000000000000, 0.9238795325112869605, 1.000000000000000000, 0.9238795325112869605, 1.000000000000000000, 0.9238795325112869605, 1.000000000000000000, 0.9238795325112869605, 1.000000000000000000, 0.9238795325112869605, 1.000000000000000000, 0.9238795325112869605, 1.000000000000000000, 0.9238795325112869605, 1.000000000000000000, 0.9238795325112869605, 1.000000000000000000, 0.9238795325112869605, 1.000000000000000000, 0.9238795325112869605, 1.000000000000000000, 0.9238795325112869605, 1.000000000000000000, 0.9238795325112869605, 1.000000000000000000, 0.9238795325112869605, 1.000000000000000000, 0.9238795325112869605, 1.000000000000000000, 0.9238795325112869605, 1.000000000000000000, 0.9238795325112869605, 1.000000000000000000, 0.9238795325112869605, 1.000000000000000000, 0.9238795325112869605, 1.000000000000000000, 0.9238795325112869605, 1.000000000000000000, 0.9238795325112869605, 1.000000000000000000, 0.9238795325112869605, 1.000000000000000000, 0.9238795325112869605, 1.000000000000000000, 0.9238795325112869605, 1.000000000000000000, 0.9238795325112869605, 1.000000000000000000, 0.9238795325112869605, 1.000000000000000000, 0.9238795325112869605, 1.000000000000000000, 0.9238795325112869605, 1.000000000000000000, 0.9238795325112869605, 1.000000000000000000, 0.9238795325112869605, 1.000000000000000000, 0.9238795325112869605, 1.000000000000000000, 0.9238795325112869605, 1.000000000000000000, 0.9238795325112869605, 1.000000000000000000, 0.9238795325112869605, 1.000000000000000000, 0.9238795325112869605, 1.000000000000000000, 0.9238795325112869605, 1.000000000000000000, 0.9238795325112869605, 1.000000000000000000, 0.9238795325112869605, 1.000000000000000000, 0.9238795325112869605, 1.000000000000000000, 0.9238795325112869605, 1.000000000000000000, 0.9238795325112869605, 1.000000000000000000, 0.9238795325112869605, 1.000000000000000000, 0.9238795325112869605, 1.000000000000000000, 0.9238795325112869605, 1.000000000000000000, 0.9238795325112869605, 1.000000000000000000, 0.9238795325112869605, 1.000000000000000000, 0.9238795325112869605, 1.000000000000000000, 0.9238795325112869605, 1.000000000000000000, 0.9238795325112869605, 1.000000000000000000, 0.9238795325112869605, 1.000000000000000000, 0.9238795325112869605, 1.000000000000000000) ) ) 
 REPRESENTATION_ITEM ( '' )  SURFACE ( )  );
#2590 = AXIS2_PLACEMENT_3D ( 'NONE', #14721, #584, #27744 ) ;
#2591 = CARTESIAN_POINT ( 'NONE',  ( 125.1626748109119802, -9.988377603198980381, -10.36322818467138518 ) ) ;
#2592 = CARTESIAN_POINT ( 'NONE',  ( 116.1431348109119881, 0.1319031606808879209, -14.10382304977623669 ) ) ;
#2593 = CARTESIAN_POINT ( 'NONE',  ( 124.3117748109119844, -10.30919188438810075, -12.61870101168855918 ) ) ;
#2594 = DIRECTION ( 'NONE',  ( -0.000000000000000000, -0.9284778069183721172, -0.3713878862591650232 ) ) ;
#2595 = AXIS2_PLACEMENT_3D ( 'NONE', #30427, #27464, #13777 ) ;
#2596 = CARTESIAN_POINT ( 'NONE',  ( 121.8965016859119856, -0.6942167230862511529, -9.935906262978006609 ) ) ;
#2597 = ORIENTED_EDGE ( 'NONE', *, *, #22814, .T. ) ;
#2598 = CARTESIAN_POINT ( 'NONE',  ( 60.11760374155740294, -14.70486118635416695, -7.429569208445770734 ) ) ;
#2599 = CARTESIAN_POINT ( 'NONE',  ( 107.4960827545248350, -6.936859964151250502, -8.388885654883777576 ) ) ;
#2600 = CARTESIAN_POINT ( 'NONE',  ( 115.8999108795247821, -1.325403438956436419, -16.93181055722138595 ) ) ;
#2601 = CARTESIAN_POINT ( 'NONE',  ( 117.7882081442453170, -3.505236298600246325, -18.68346056562440793 ) ) ;
#2602 = CARTESIAN_POINT ( 'NONE',  ( 114.4980614775786734, -2.084020599724406786, -8.691656652584148546 ) ) ;
#2603 = CARTESIAN_POINT ( 'NONE',  ( 125.5597614775786326, -7.894159318335813857, -9.358103419637837206 ) ) ;
#2604 = VERTEX_POINT ( 'NONE', #43331 ) ;
#2605 = DIRECTION ( 'NONE',  ( -0.9063289528979890930, -0.4225728684367167087, 0.000000000000000000 ) ) ;
#2606 = CARTESIAN_POINT ( 'NONE',  ( 119.2631014775786298, -9.565557343593413364, -10.61323700422348004 ) ) ;
#2607 = CARTESIAN_POINT ( 'NONE',  ( 113.9307948109119764, -10.15424416112533912, -14.75197769757731336 ) ) ;
#2608 = DIRECTION ( 'NONE',  ( 0.000000000000000000, 0.000000000000000000, 1.000000000000000000 ) ) ;
#2609 = CARTESIAN_POINT ( 'NONE',  ( 111.5020881442453202, -0.2054726073303936307, -16.14774885094461965 ) ) ;
#2611 = CARTESIAN_POINT ( 'NONE',  ( 123.1205148109119563, -1.834011780172310813, -8.268836392978581529 ) ) ;
#2610 = CARTESIAN_POINT ( 'NONE',  ( 70.27122018245525226, -26.36473080579375861, -5.633705330403472544 ) ) ;
#2612 = EDGE_CURVE ( 'NONE', #7036, #28148, #18318, .T. ) ;
#2613 = CARTESIAN_POINT ( 'NONE',  ( 112.5126281442453120, -10.30919188438810075, -12.61870101168855918 ) ) ;
#2614 = VERTEX_POINT ( 'NONE', #11645 ) ;
#2615 = FACE_OUTER_BOUND ( 'NONE', #42287, .T. ) ;
#2616 = CYLINDRICAL_SURFACE ( 'NONE', #6503, 1.999999999999998890 ) ;
#2617 = CARTESIAN_POINT ( 'NONE',  ( 114.5803015045248117, -2.477300249445798297, -7.631215200338321125 ) ) ;
#2618 = CARTESIAN_POINT ( 'NONE',  ( 111.8886348109120092, -3.383040157471821630, -19.15922257007629170 ) ) ;
#2619 = CARTESIAN_POINT ( 'NONE',  ( 120.7947214775786193, -0.8288870151387760510, -10.36305467784173118 ) ) ;
#2620 = LINE ( 'NONE', #6508, #6760 ) ;
#2621 = CARTESIAN_POINT ( 'NONE',  ( 113.8163171295247764, 0.1403307496149613920, -13.39321520033831447 ) ) ;
#2622 = DIRECTION ( 'NONE',  ( -0.9908103287288504424, 0.1352586133457950313, 0.000000000000000000 ) ) ;
#2623 = CARTESIAN_POINT ( 'NONE',  ( 128.2184548109119930, -4.863998795839242995, -13.39321520033831447 ) ) ;
#2624 = CARTESIAN_POINT ( 'NONE',  ( 112.6260814775786514, -0.8288870151387760510, -10.36305467784173118 ) ) ;
#2625 = CARTESIAN_POINT ( 'NONE',  ( 111.3160046295247838, -4.863998795839590272, -7.631215200338315796 ) ) ;
#2626 = CARTESIAN_POINT ( 'NONE',  ( 117.2294421295247844, -10.76310523276723785, -5.182735500338556456 ) ) ;
#2627 = CARTESIAN_POINT ( 'NONE',  ( 112.4967077545247633, -7.250697342233347165, -7.631215200338321125 ) ) ;
#2628 = CARTESIAN_POINT ( 'NONE',  ( 125.8433948109119456, -1.834011780172310813, -8.268836392978581529 ) ) ;
#2629 = CARTESIAN_POINT ( 'NONE',  ( 123.2339681442453241, -6.344957434206665248, -7.627207830600338134 ) ) ;
#2630 = CARTESIAN_POINT ( 'NONE',  ( 115.3931121053768436, 0.3967854368539331933, -16.28112951403852549 ) ) ;
#2631 = STYLED_ITEM ( 'NONE', ( #35992 ), #43323 ) ;
#2632 = CARTESIAN_POINT ( 'NONE',  ( 119.4900081442453086, -1.834011780172310813, -8.268836392978581529 ) ) ;
#2633 = CARTESIAN_POINT ( 'NONE',  ( 114.0442481442453300, -1.834011780172310813, -8.268836392978581529 ) ) ;
#2634 = VERTEX_POINT ( 'NONE', #7773 ) ;
#2635 = CARTESIAN_POINT ( 'NONE',  ( 114.6115148109119986, -6.222761293078241884, -8.102969835052219238 ) ) ;
#2636 = CARTESIAN_POINT ( 'NONE',  ( 112.9097148109120070, -9.565557343593413364, -10.61323700422348004 ) ) ;
#2637 = CARTESIAN_POINT ( 'NONE',  ( 124.7655881442452852, 0.5811942927096110934, -14.16772938898807510 ) ) ;
#2638 = CARTESIAN_POINT ( 'NONE',  ( 113.4202548109119846, -10.30919188438810075, -12.61870101168855918 ) ) ;
#2639 = PRODUCT_CONTEXT ( 'NONE', #2041, 'mechanical' ) ;
#2640 = CARTESIAN_POINT ( 'NONE',  ( 113.1366214775786432, -7.643976991954077427, -18.09477374809248928 ) ) ;
#2641 = ORIENTED_EDGE ( 'NONE', *, *, #30471, .T. ) ;
#2642 = CARTESIAN_POINT ( 'NONE',  ( 116.0296814775786345, -1.833838273342658809, -17.42832698103878286 ) ) ;
#2643 = CARTESIAN_POINT ( 'NONE',  ( 112.5693548109119888, -10.63000616557722466, -14.87417383870573495 ) ) ;
#2644 = CARTESIAN_POINT ( 'NONE',  ( 110.8298327545248299, -6.936859964151250502, -8.388885654883777576 ) ) ;
#2645 = CARTESIAN_POINT ( 'NONE',  ( 123.1772414775786189, -5.574606645277164318, -18.38911715685844683 ) ) ;
#2646 = CARTESIAN_POINT ( 'NONE',  ( 116.8546682094391400, -0.5381813604855363309, -16.38644560622362434 ) ) ;
#2647 = CARTESIAN_POINT ( 'NONE',  ( 66.19909219943727408, -62.82237896425675672, -47.71602681600973739 ) ) ;
#2648 = VERTEX_POINT ( 'NONE', #25778 ) ;
#2649 = CARTESIAN_POINT ( 'NONE',  ( 123.5633766859119760, -9.033780868592240054, -16.85052413769862056 ) ) ;
#2650 = CARTESIAN_POINT ( 'NONE',  ( 125.9568481442452850, -6.344957434206665248, -7.627207830600338134 ) ) ;
#2651 = AXIS2_PLACEMENT_3D ( 'NONE', #8393, #4736, #29364 ) ;
#2652 = CARTESIAN_POINT ( 'NONE',  ( 71.62928943233082180, 0.3619606153155430217, -12.39321520033831447 ) ) ;
#2653 = SURFACE_STYLE_USAGE ( .BOTH. , #30253 ) ;
#2654 = CARTESIAN_POINT ( 'NONE',  ( 117.0590115223097030, 1.678907146655578053, -5.492932798708517694 ) ) ;
#2655 = CARTESIAN_POINT ( 'NONE',  ( 114.0440301496069821, 0.3591747506842615789, -14.64321520033831447 ) ) ;
#2656 = CARTESIAN_POINT ( 'NONE',  ( 109.1629577545248395, -2.791137627527939813, -18.39754474579286025 ) ) ;
#2657 = CARTESIAN_POINT ( 'NONE',  ( 111.2647481608379820, 0.3867979994853637526, -14.64321520033833757 ) ) ;
#2658 = AXIS2_PLACEMENT_3D ( 'NONE', #38258, #38475, #4506 ) ;
#2659 = CARTESIAN_POINT ( 'NONE',  ( 117.9016614775786280, -9.988377603198976828, -10.36322818467138340 ) ) ;
#2660 = LINE ( 'NONE', #10200, #44967 ) ;
#2661 = CARTESIAN_POINT ( 'NONE',  ( 94.99177781699742695, -25.99489077589524300, -13.39321520033831447 ) ) ;
#2662 =( BOUNDED_SURFACE ( )  B_SPLINE_SURFACE ( 1, 2, ( 
 ( #28413, #808, #17921, #1262, #18378, #42101, #42546, #25667, #32266, #4457, #10864, #38648, #15172, #21340, #590, #3774, #28639, #14500, #32041, #1034, #14951, #14726, #29078, #35225, #39572, #22014, #28862, #17698, #21565, #31596, #365, #7419, #14276, #42322, #24759, #42990, #35909, #11084, #4674, #24986, #38880, #7650, #15625, #37029, #15856, #32707, #29980, #26108, #29305, #15401, #22234, #8780, #18816, #1480, #12666, #19716, #33602, #32928, #40477, #33153, #40015, #2379, #19496, #29751, #43218, #25887, #16308, #8560, #5125, #40702, #43663, #19041, #19274, #22911, #12439, #1929, #5797, #22460, #12895, #9238, #33375, #36130, #22684, #4900, #11986, #39789, #36354, #29531, #1704, #30209, #36804, #43446, #44130, #12211, #26793, #2145, #36582, #5358, #26338, #40246, #43898, #9014, #5571, #16076, #26564, #23147, #6026, #19949, #477, #7540, #21457, #20185, #28302, #21010, #27862, #35340, #4112, #256, #27021, #33837, #34070, #21233, #14615, #28083, #16765, #2606, #40936, #18033, #42214, #695, #14165, #24654, #3893, #10975, #31930, #17593, #28532, #31707, #34884, #23606, #38539, #30435, #3672, #2836, #24878, #31487, #14390, #16538, #6265, #35112, #37491, #38770, #9460, #23372, #7314, #17813, #44354, #37253, #24431, #41991, #37, #13114, #9689, #30662, #13950, #41772, #10532, #38323, #7100, #10756, #11202, #25336, #26005, #12101, #926, #11646, #8225, #22131, #4568, #36475, #19158, #1814, #35796, #36024, #11431, #8670, #25779, #35569, #4792, #33039, #25555, #32604, #18713, #15741, #28755, #42438, #36248, #39909, #22573, #25107, #32382, #5242, #39004, #18262, #39461, #1149, #7774, #1373, #11875, #39229, #21681, #39686, #18933, #15286, #29193, #43105, #4342, #32158, #7994, #18492, #14845, #8451, #22354, #5015, #15066, #42885, #15511, #42660, #28980, #21902, #32820, #1590, #29418, #43332, #20070, #26225, #19381, #2495, #30320, #44246, #37142, #44015, #36691, #5686, #33725, #40360, #16424, #5916, #22797, #29643, #23721, #27131, #33489, #41055, #29871, #43557, #9349 ),
 ( #13004, #36915, #40134, #15968, #9812, #16649, #20293, #26903, #40823, #23494, #30544, #37611, #19838, #6385, #6150, #23259, #43786, #9578, #5461, #37380, #9124, #44465, #40590, #33956, #33269, #26458, #2723, #12551, #13230, #34178, #2953, #12326, #8899, #2044, #23028, #12777, #19605, #2267, #16195, #30099, #26679, #41501, #37829, #38486, #31213, #7261, #17103, #30771, #44921, #421, #31653, #20519, #45137, #13678, #28029, #27587, #21178, #10921, #35281, #197, #14113, #10041, #16880, #13896, #3617, #6834, #6606, #38713, #17756, #10257, #34399, #35053, #27802, #3836, #30995, #44697, #24164, #14337, #28251, #3180, #41716, #10481, #24382, #38056, #24822, #7482, #21401, #20739, #38268, #34619, #42160, #41937, #23948, #7049, #13457, #10700, #20960, #3406, #17323, #27361, #34832, #17535, #41281, #31430, #24603, #1096, #4739, #25503, #15012, #32766, #35513, #39857, #22301, #15231, #22520, #35745, #17979, #31879, #21625, #644, #42607, #14559, #1540, #18660, #38944, #18875, #39174, #15461, #29140, #11372, #29367, #42832, #28478, #11819, #7938, #11146, #42382, #4055, #4518, #25050, #7712, #39634, #43278, #12047, #14788, #36198, #28925, #21849, #25950, #8622, #39408, #4285, #18204, #28702, #43053, #32102, #22081, #25278, #869, #18441, #32330, #4963, #11593, #8171, #32551, #25727, #35969, #1320, #8397, #13178, #12954, #16140, #5416, #5860, #12277, #30042, #15918, #23437, #2211, #26850, #43509, #9755, #12721, #19332, #33218, #2666, #40763, #9519, #40308, #37321, #6092, #19782, #26173, #44192, #27080, #20011, #5634, #26624, #36417, #22741, #19554, #33432, #40538, #43958, #41001, #36643, #5185, #30266, #33896, #16599, #19102, #26398, #30492, #32989, #40079, #9299, #9072, #44412, #23207, #33664, #1992, #1763, #2442, #15689, #37085, #16364, #29591, #8842, #29816, #43732, #12501, #22974, #36864, #13840, #6999, #27533, #24113, #41886, #20243, #10205, #34129, #38007, #13623, #374, #2898, #14063, #16827, #13406, #41671, #24336, #38220, #31162, #6781, #30720, #44867, #27756, #34349 ) ),
 .UNSPECIFIED., .F., .F., .T. ) 
 B_SPLINE_SURFACE_WITH_KNOTS ( ( 2, 2 ),
 ( 3, 2, 2, 2, 2, 2, 2, 2, 2, 2, 2, 2, 2, 2, 2, 2, 2, 2, 2, 2, 2, 2, 2, 2, 2, 2, 2, 2, 2, 2, 2, 2, 2, 2, 2, 2, 2, 2, 2, 2, 2, 2, 2, 2, 2, 2, 2, 2, 2, 2, 2, 2, 2, 2, 2, 2, 2, 2, 2, 2, 2, 2, 2, 2, 2, 2, 2, 2, 2, 2, 2, 2, 2, 2, 2, 2, 2, 2, 2, 2, 2, 2, 2, 2, 2, 2, 2, 2, 2, 2, 2, 2, 2, 2, 2, 2, 2, 2, 2, 2, 2, 2, 2, 2, 2, 2, 2, 2, 2, 2, 2, 2, 2, 2, 2, 2, 2, 2, 2, 2, 2, 2, 2, 2, 2, 2, 2, 2, 3 ),
 ( 0.000000000000000000, 1.000000000000000000 ),
 ( 0.000000000000000000, 0.007812500000000000000, 0.01562500000000000000, 0.02343750000000000000, 0.03125000000000000000, 0.03906250000000000000, 0.04687500000000000000, 0.05468750000000000000, 0.06250000000000000000, 0.07031250000000000000, 0.07812500000000000000, 0.08593750000000000000, 0.09375000000000000000, 0.1015625000000000000, 0.1093750000000000000, 0.1171875000000000000, 0.1250000000000000000, 0.1328125000000000000, 0.1406250000000000000, 0.1484375000000000000, 0.1562500000000000000, 0.1640625000000000000, 0.1718750000000000000, 0.1796875000000000000, 0.1875000000000000000, 0.1953125000000000000, 0.2031250000000000000, 0.2109375000000000000, 0.2187500000000000000, 0.2265625000000000000, 0.2343750000000000000, 0.2421875000000000000, 0.2500000000000000000, 0.2578125000000000000, 0.2656250000000000000, 0.2734375000000000000, 0.2812500000000000000, 0.2890625000000000000, 0.2968750000000000000, 0.3046875000000000000, 0.3125000000000000000, 0.3203125000000000000, 0.3281250000000000000, 0.3359375000000000000, 0.3437500000000000000, 0.3515625000000000000, 0.3593750000000000000, 0.3671875000000000000, 0.3750000000000000000, 0.3828125000000000000, 0.3906250000000000000, 0.3984375000000000000, 0.4062500000000000000, 0.4140625000000000000, 0.4218750000000000000, 0.4296875000000000000, 0.4375000000000000000, 0.4453125000000000000, 0.4531250000000000000, 0.4609375000000000000, 0.4687500000000000000, 0.4765625000000000000, 0.4843750000000000000, 0.4921875000000000000, 0.5000000000000000000, 0.5078125000000000000, 0.5156250000000000000, 0.5234375000000000000, 0.5312500000000000000, 0.5390625000000000000, 0.5468750000000000000, 0.5546875000000000000, 0.5625000000000000000, 0.5703125000000000000, 0.5781250000000000000, 0.5859375000000000000, 0.5937500000000000000, 0.6015625000000000000, 0.6093750000000000000, 0.6171875000000000000, 0.6250000000000000000, 0.6328125000000000000, 0.6406250000000000000, 0.6484375000000000000, 0.6562500000000000000, 0.6640625000000000000, 0.6718750000000000000, 0.6796875000000000000, 0.6875000000000000000, 0.6953125000000000000, 0.7031250000000000000, 0.7109375000000000000, 0.7187500000000000000, 0.7265625000000000000, 0.7343750000000000000, 0.7421875000000000000, 0.7500000000000000000, 0.7578125000000000000, 0.7656250000000000000, 0.7734375000000000000, 0.7812500000000000000, 0.7890625000000000000, 0.7968750000000000000, 0.8046875000000000000, 0.8125000000000000000, 0.8203125000000000000, 0.8281250000000000000, 0.8359375000000000000, 0.8437500000000000000, 0.8515625000000000000, 0.8593750000000000000, 0.8671875000000000000, 0.8750000000000000000, 0.8828125000000000000, 0.8906250000000000000, 0.8984375000000000000, 0.9062500000000000000, 0.9140625000000000000, 0.9218750000000000000, 0.9296875000000000000, 0.9375000000000000000, 0.9453125000000000000, 0.9531250000000000000, 0.9609375000000000000, 0.9687500000000000000, 0.9765625000000000000, 0.9843750000000000000, 0.9921875000000000000, 1.000000000000000000 ),
 .UNSPECIFIED. ) 
 GEOMETRIC_REPRESENTATION_ITEM ( )  RATIONAL_B_SPLINE_SURFACE ( (
 ( 1.000000000000000000, 0.9238795325112869605, 1.000000000000000000, 0.9238795325112869605, 1.000000000000000000, 0.9238795325112869605, 1.000000000000000000, 0.9238795325112869605, 1.000000000000000000, 0.9238795325112869605, 1.000000000000000000, 0.9238795325112869605, 1.000000000000000000, 0.9238795325112869605, 1.000000000000000000, 0.9238795325112869605, 1.000000000000000000, 0.9238795325112869605, 1.000000000000000000, 0.9238795325112869605, 1.000000000000000000, 0.9238795325112869605, 1.000000000000000000, 0.9238795325112869605, 1.000000000000000000, 0.9238795325112869605, 1.000000000000000000, 0.9238795325112869605, 1.000000000000000000, 0.9238795325112869605, 1.000000000000000000, 0.9238795325112869605, 1.000000000000000000, 0.9238795325112869605, 1.000000000000000000, 0.9238795325112869605, 1.000000000000000000, 0.9238795325112869605, 1.000000000000000000, 0.9238795325112869605, 1.000000000000000000, 0.9238795325112869605, 1.000000000000000000, 0.9238795325112869605, 1.000000000000000000, 0.9238795325112869605, 1.000000000000000000, 0.9238795325112869605, 1.000000000000000000, 0.9238795325112869605, 1.000000000000000000, 0.9238795325112869605, 1.000000000000000000, 0.9238795325112869605, 1.000000000000000000, 0.9238795325112869605, 1.000000000000000000, 0.9238795325112869605, 1.000000000000000000, 0.9238795325112869605, 1.000000000000000000, 0.9238795325112869605, 1.000000000000000000, 0.9238795325112869605, 1.000000000000000000, 0.9238795325112869605, 1.000000000000000000, 0.9238795325112869605, 1.000000000000000000, 0.9238795325112869605, 1.000000000000000000, 0.9238795325112869605, 1.000000000000000000, 0.9238795325112869605, 1.000000000000000000, 0.9238795325112869605, 1.000000000000000000, 0.9238795325112869605, 1.000000000000000000, 0.9238795325112869605, 1.000000000000000000, 0.9238795325112869605, 1.000000000000000000, 0.9238795325112869605, 1.000000000000000000, 0.9238795325112869605, 1.000000000000000000, 0.9238795325112869605, 1.000000000000000000, 0.9238795325112869605, 1.000000000000000000, 0.9238795325112869605, 1.000000000000000000, 0.9238795325112869605, 1.000000000000000000, 0.9238795325112869605, 1.000000000000000000, 0.9238795325112869605, 1.000000000000000000, 0.9238795325112869605, 1.000000000000000000, 0.9238795325112869605, 1.000000000000000000, 0.9238795325112869605, 1.000000000000000000, 0.9238795325112869605, 1.000000000000000000, 0.9238795325112869605, 1.000000000000000000, 0.9238795325112869605, 1.000000000000000000, 0.9238795325112869605, 1.000000000000000000, 0.9238795325112869605, 1.000000000000000000, 0.9238795325112869605, 1.000000000000000000, 0.9238795325112869605, 1.000000000000000000, 0.9238795325112869605, 1.000000000000000000, 0.9238795325112869605, 1.000000000000000000, 0.9238795325112869605, 1.000000000000000000, 0.9238795325112869605, 1.000000000000000000, 0.9238795325112869605, 1.000000000000000000, 0.9238795325112869605, 1.000000000000000000, 0.9238795325112869605, 1.000000000000000000, 0.9238795325112869605, 1.000000000000000000, 0.9238795325112869605, 1.000000000000000000, 0.9238795325112869605, 1.000000000000000000, 0.9238795325112869605, 1.000000000000000000, 0.9238795325112869605, 1.000000000000000000, 0.9238795325112869605, 1.000000000000000000, 0.9238795325112869605, 1.000000000000000000, 0.9238795325112869605, 1.000000000000000000, 0.9238795325112869605, 1.000000000000000000, 0.9238795325112869605, 1.000000000000000000, 0.9238795325112869605, 1.000000000000000000, 0.9238795325112869605, 1.000000000000000000, 0.9238795325112869605, 1.000000000000000000, 0.9238795325112869605, 1.000000000000000000, 0.9238795325112869605, 1.000000000000000000, 0.9238795325112869605, 1.000000000000000000, 0.9238795325112869605, 1.000000000000000000, 0.9238795325112869605, 1.000000000000000000, 0.9238795325112869605, 1.000000000000000000, 0.9238795325112869605, 1.000000000000000000, 0.9238795325112869605, 1.000000000000000000, 0.9238795325112869605, 1.000000000000000000, 0.9238795325112869605, 1.000000000000000000, 0.9238795325112869605, 1.000000000000000000, 0.9238795325112869605, 1.000000000000000000, 0.9238795325112869605, 1.000000000000000000, 0.9238795325112869605, 1.000000000000000000, 0.9238795325112869605, 1.000000000000000000, 0.9238795325112869605, 1.000000000000000000, 0.9238795325112869605, 1.000000000000000000, 0.9238795325112869605, 1.000000000000000000, 0.9238795325112869605, 1.000000000000000000, 0.9238795325112869605, 1.000000000000000000, 0.9238795325112869605, 1.000000000000000000, 0.9238795325112869605, 1.000000000000000000, 0.9238795325112869605, 1.000000000000000000, 0.9238795325112869605, 1.000000000000000000, 0.9238795325112869605, 1.000000000000000000, 0.9238795325112869605, 1.000000000000000000, 0.9238795325112869605, 1.000000000000000000, 0.9238795325112869605, 1.000000000000000000, 0.9238795325112869605, 1.000000000000000000, 0.9238795325112869605, 1.000000000000000000, 0.9238795325112869605, 1.000000000000000000, 0.9238795325112869605, 1.000000000000000000, 0.9238795325112869605, 1.000000000000000000, 0.9238795325112869605, 1.000000000000000000, 0.9238795325112869605, 1.000000000000000000, 0.9238795325112869605, 1.000000000000000000, 0.9238795325112869605, 1.000000000000000000, 0.9238795325112869605, 1.000000000000000000, 0.9238795325112869605, 1.000000000000000000, 0.9238795325112869605, 1.000000000000000000, 0.9238795325112869605, 1.000000000000000000, 0.9238795325112869605, 1.000000000000000000, 0.9238795325112869605, 1.000000000000000000, 0.9238795325112869605, 1.000000000000000000, 0.9238795325112869605, 1.000000000000000000, 0.9238795325112869605, 1.000000000000000000, 0.9238795325112869605, 1.000000000000000000, 0.9238795325112869605, 1.000000000000000000, 0.9238795325112869605, 1.000000000000000000),
 ( 1.000000000000000000, 0.9238795325112869605, 1.000000000000000000, 0.9238795325112869605, 1.000000000000000000, 0.9238795325112869605, 1.000000000000000000, 0.9238795325112869605, 1.000000000000000000, 0.9238795325112869605, 1.000000000000000000, 0.9238795325112869605, 1.000000000000000000, 0.9238795325112869605, 1.000000000000000000, 0.9238795325112869605, 1.000000000000000000, 0.9238795325112869605, 1.000000000000000000, 0.9238795325112869605, 1.000000000000000000, 0.9238795325112869605, 1.000000000000000000, 0.9238795325112869605, 1.000000000000000000, 0.9238795325112869605, 1.000000000000000000, 0.9238795325112869605, 1.000000000000000000, 0.9238795325112869605, 1.000000000000000000, 0.9238795325112869605, 1.000000000000000000, 0.9238795325112869605, 1.000000000000000000, 0.9238795325112869605, 1.000000000000000000, 0.9238795325112869605, 1.000000000000000000, 0.9238795325112869605, 1.000000000000000000, 0.9238795325112869605, 1.000000000000000000, 0.9238795325112869605, 1.000000000000000000, 0.9238795325112869605, 1.000000000000000000, 0.9238795325112869605, 1.000000000000000000, 0.9238795325112869605, 1.000000000000000000, 0.9238795325112869605, 1.000000000000000000, 0.9238795325112869605, 1.000000000000000000, 0.9238795325112869605, 1.000000000000000000, 0.9238795325112869605, 1.000000000000000000, 0.9238795325112869605, 1.000000000000000000, 0.9238795325112869605, 1.000000000000000000, 0.9238795325112869605, 1.000000000000000000, 0.9238795325112869605, 1.000000000000000000, 0.9238795325112869605, 1.000000000000000000, 0.9238795325112869605, 1.000000000000000000, 0.9238795325112869605, 1.000000000000000000, 0.9238795325112869605, 1.000000000000000000, 0.9238795325112869605, 1.000000000000000000, 0.9238795325112869605, 1.000000000000000000, 0.9238795325112869605, 1.000000000000000000, 0.9238795325112869605, 1.000000000000000000, 0.9238795325112869605, 1.000000000000000000, 0.9238795325112869605, 1.000000000000000000, 0.9238795325112869605, 1.000000000000000000, 0.9238795325112869605, 1.000000000000000000, 0.9238795325112869605, 1.000000000000000000, 0.9238795325112869605, 1.000000000000000000, 0.9238795325112869605, 1.000000000000000000, 0.9238795325112869605, 1.000000000000000000, 0.9238795325112869605, 1.000000000000000000, 0.9238795325112869605, 1.000000000000000000, 0.9238795325112869605, 1.000000000000000000, 0.9238795325112869605, 1.000000000000000000, 0.9238795325112869605, 1.000000000000000000, 0.9238795325112869605, 1.000000000000000000, 0.9238795325112869605, 1.000000000000000000, 0.9238795325112869605, 1.000000000000000000, 0.9238795325112869605, 1.000000000000000000, 0.9238795325112869605, 1.000000000000000000, 0.9238795325112869605, 1.000000000000000000, 0.9238795325112869605, 1.000000000000000000, 0.9238795325112869605, 1.000000000000000000, 0.9238795325112869605, 1.000000000000000000, 0.9238795325112869605, 1.000000000000000000, 0.9238795325112869605, 1.000000000000000000, 0.9238795325112869605, 1.000000000000000000, 0.9238795325112869605, 1.000000000000000000, 0.9238795325112869605, 1.000000000000000000, 0.9238795325112869605, 1.000000000000000000, 0.9238795325112869605, 1.000000000000000000, 0.9238795325112869605, 1.000000000000000000, 0.9238795325112869605, 1.000000000000000000, 0.9238795325112869605, 1.000000000000000000, 0.9238795325112869605, 1.000000000000000000, 0.9238795325112869605, 1.000000000000000000, 0.9238795325112869605, 1.000000000000000000, 0.9238795325112869605, 1.000000000000000000, 0.9238795325112869605, 1.000000000000000000, 0.9238795325112869605, 1.000000000000000000, 0.9238795325112869605, 1.000000000000000000, 0.9238795325112869605, 1.000000000000000000, 0.9238795325112869605, 1.000000000000000000, 0.9238795325112869605, 1.000000000000000000, 0.9238795325112869605, 1.000000000000000000, 0.9238795325112869605, 1.000000000000000000, 0.9238795325112869605, 1.000000000000000000, 0.9238795325112869605, 1.000000000000000000, 0.9238795325112869605, 1.000000000000000000, 0.9238795325112869605, 1.000000000000000000, 0.9238795325112869605, 1.000000000000000000, 0.9238795325112869605, 1.000000000000000000, 0.9238795325112869605, 1.000000000000000000, 0.9238795325112869605, 1.000000000000000000, 0.9238795325112869605, 1.000000000000000000, 0.9238795325112869605, 1.000000000000000000, 0.9238795325112869605, 1.000000000000000000, 0.9238795325112869605, 1.000000000000000000, 0.9238795325112869605, 1.000000000000000000, 0.9238795325112869605, 1.000000000000000000, 0.9238795325112869605, 1.000000000000000000, 0.9238795325112869605, 1.000000000000000000, 0.9238795325112869605, 1.000000000000000000, 0.9238795325112869605, 1.000000000000000000, 0.9238795325112869605, 1.000000000000000000, 0.9238795325112869605, 1.000000000000000000, 0.9238795325112869605, 1.000000000000000000, 0.9238795325112869605, 1.000000000000000000, 0.9238795325112869605, 1.000000000000000000, 0.9238795325112869605, 1.000000000000000000, 0.9238795325112869605, 1.000000000000000000, 0.9238795325112869605, 1.000000000000000000, 0.9238795325112869605, 1.000000000000000000, 0.9238795325112869605, 1.000000000000000000, 0.9238795325112869605, 1.000000000000000000, 0.9238795325112869605, 1.000000000000000000, 0.9238795325112869605, 1.000000000000000000, 0.9238795325112869605, 1.000000000000000000, 0.9238795325112869605, 1.000000000000000000, 0.9238795325112869605, 1.000000000000000000, 0.9238795325112869605, 1.000000000000000000, 0.9238795325112869605, 1.000000000000000000, 0.9238795325112869605, 1.000000000000000000, 0.9238795325112869605, 1.000000000000000000, 0.9238795325112869605, 1.000000000000000000, 0.9238795325112869605, 1.000000000000000000, 0.9238795325112869605, 1.000000000000000000, 0.9238795325112869605, 1.000000000000000000, 0.9238795325112869605, 1.000000000000000000) ) ) 
 REPRESENTATION_ITEM ( '' )  SURFACE ( )  );
#2663 = CARTESIAN_POINT ( 'NONE',  ( 121.0783548109119749, -9.565557343593413364, -10.61323700422348004 ) ) ;
#2664 = CARTESIAN_POINT ( 'NONE',  ( 119.7434548109119703, 0.2775794806942583071, -14.81454154325457928 ) ) ;
#2665 = ORIENTED_EDGE ( 'NONE', *, *, #4911, .T. ) ;
#2666 = CARTESIAN_POINT ( 'NONE',  ( 122.2128881442453263, -1.834011780172310813, -8.268836392978581529 ) ) ;
#2667 = CARTESIAN_POINT ( 'NONE',  ( 120.9081748109119872, -5.638512984488999180, -18.83840828888717311 ) ) ;
#2668 = CARTESIAN_POINT ( 'NONE',  ( 126.0135748109119902, -8.166667518702819706, -8.995218007635861213 ) ) ;
#2669 = CARTESIAN_POINT ( 'NONE',  ( 112.2857214775786474, -5.574606645277164318, -18.38911715685844683 ) ) ;
#2670 = CARTESIAN_POINT ( 'NONE',  ( 113.8740681442453138, 0.5811942927096154232, -14.16772938898807155 ) ) ;
#2671 = CARTESIAN_POINT ( 'NONE',  ( 125.3328548109119964, -9.261995988541697145, -16.69588392320189030 ) ) ;
#2672 = CARTESIAN_POINT ( 'NONE',  ( 112.4272546295247821, -4.863998795839590272, -7.631215200338315796 ) ) ;
#2673 = CARTESIAN_POINT ( 'NONE',  ( 105.2735827545248810, -6.936859964151250502, -8.388885654883777576 ) ) ;
#2674 = CARTESIAN_POINT ( 'NONE',  ( 115.9693640045247776, -10.62599879583958717, -11.00651665394454604 ) ) ;
#2675 = CARTESIAN_POINT ( 'NONE',  ( 115.9729548109119861, -3.505236298600246325, -18.68346056562440793 ) ) ;
#2676 = CARTESIAN_POINT ( 'NONE',  ( 115.2922348109119781, 0.4262465694468514643, -12.03445270309931736 ) ) ;
#2677 = CARTESIAN_POINT ( 'NONE',  ( 112.9389878519202739, 0.2518737723193609224, -12.14321520033831625 ) ) ;
#2678 = CONICAL_SURFACE ( 'NONE', #7079, 2.999999999999999556, 0.9599310885968830309 ) ;
#2679 = CARTESIAN_POINT ( 'NONE',  ( 114.5108483795247878, -8.402594152722688392, -16.93181055722141792 ) ) ;
#2680 = VERTEX_POINT ( 'NONE', #25554 ) ;
#2681 = CARTESIAN_POINT ( 'NONE',  ( 124.0281414775786146, -7.643976991954092526, -18.09477374809249284 ) ) ;
#2682 = CARTESIAN_POINT ( 'NONE',  ( 113.5904348109119866, -7.893985811506177619, -18.51759400769804742 ) ) ;
#2683 = CARTESIAN_POINT ( 'NONE',  ( 113.2134394150595966, -2.423081321603721694, -17.89265170041262465 ) ) ;
#2684 = CARTESIAN_POINT ( 'NONE',  ( 121.1325173109119788, -9.289237151508434209, -11.05642687123711276 ) ) ;
#2685 = CARTESIAN_POINT ( 'NONE',  ( 120.2990798109119766, -7.200787124940443817, -17.81845355600750835 ) ) ;
#2686 = ORIENTED_EDGE ( 'NONE', *, *, #6157, .T. ) ;
#2687 = CARTESIAN_POINT ( 'NONE',  ( 123.5196897444113517, -2.961643921203012564, -14.67744431876825928 ) ) ;
#2688 = CARTESIAN_POINT ( 'NONE',  ( 116.6091619947073070, -11.87124904611273735, -21.21647875974084840 ) ) ;
#2689 = AXIS2_PLACEMENT_3D ( 'NONE', #19513, #5144, #12230 ) ;
#2690 = ORIENTED_EDGE ( 'NONE', *, *, #24599, .T. ) ;
#2691 = CARTESIAN_POINT ( 'NONE',  ( 118.5823814775786360, -1.834011780172310813, -8.268836392978581529 ) ) ;
#2692 = CARTESIAN_POINT ( 'NONE',  ( 123.5176014775786228, -0.8288870151387760510, -10.36305467784173118 ) ) ;
#2693 = CARTESIAN_POINT ( 'NONE',  ( 119.3198281442452924, -9.859900752359374465, -12.68260735090039404 ) ) ;
#2694 = FILL_AREA_STYLE ('',( #16392 ) ) ;
#2695 = LINE ( 'NONE', #16855, #1686 ) ;
#2696 = CARTESIAN_POINT ( 'NONE',  ( 121.6456214775786293, -10.63000616557722466, -14.87417383870573495 ) ) ;
#2697 = CARTESIAN_POINT ( 'NONE',  ( 119.6034614775786196, -6.344957434206665248, -7.627207830600338134 ) ) ;
#2698 = PRESENTATION_LAYER_ASSIGNMENT (  '', '', ( #18717 ) ) ;
#2699 = CARTESIAN_POINT ( 'NONE',  ( 109.9963952545248134, -9.868328341294098749, -15.46607636864997204 ) ) ;
#2700 = CARTESIAN_POINT ( 'NONE',  ( 112.6828081442453282, -2.084020599724406786, -8.691656652584148546 ) ) ;
#2701 = SURFACE_SIDE_STYLE ('',( #6129 ) ) ;
#2702 = EDGE_LOOP ( 'NONE', ( #16935, #35690, #26572, #28944, #26319, #39425 ) ) ;
#2703 = CARTESIAN_POINT ( 'NONE',  ( 117.7882081442453170, -6.344957434206665248, -7.627207830600338134 ) ) ;
#2704 = ADVANCED_FACE ( 'NONE', ( #21680 ), #17131, .F. ) ;
#2705 = B_SPLINE_CURVE_WITH_KNOTS ( 'NONE', 3,
 ( #25216, #28195, #39346, #32487, #35683, #39116, #3999, #25444, #8113, #34988 ),
 .UNSPECIFIED., .F., .F.,
 ( 4, 3, 3, 4 ),
 ( 0.000000000000000000, 0.0001671877560958114864, 0.0003343755126086559717, 0.0006438490228507209303 ),
 .UNSPECIFIED. ) ;
#2706 = CARTESIAN_POINT ( 'NONE',  ( 114.3846081442453197, 0.4262465694468514643, -12.03445270309931736 ) ) ;
#2707 = DIRECTION ( 'NONE',  ( -0.9908103287288504424, 0.1352586133457950313, 0.000000000000000000 ) ) ;
#2708 = CARTESIAN_POINT ( 'NONE',  ( 125.6164881442453094, -9.565557343593413364, -10.61323700422348004 ) ) ;
#2709 = ORIENTED_EDGE ( 'NONE', *, *, #14877, .F. ) ;
#2710 = CARTESIAN_POINT ( 'NONE',  ( 122.0994348109119443, 0.9020085738987339008, -11.91225656197089222 ) ) ;
#2712 = CARTESIAN_POINT ( 'NONE',  ( 90.45092582798827152, -25.23119213852205789, -15.24166438581092109 ) ) ;
#2711 = CIRCLE ( 'NONE', #38373, 2.000000000000000444 ) ;
#2713 = CARTESIAN_POINT ( 'NONE',  ( 113.6471614775786492, -4.153390946401321671, -8.397313243818183892 ) ) ;
#2714 = LINE ( 'NONE', #30534, #38940 ) ;
#2715 = DIRECTION ( 'NONE',  ( 0.000000000000000000, -0.9242245927363029745, -0.3818493186865927758 ) ) ;
#2716 = CARTESIAN_POINT ( 'NONE',  ( 116.0864081442453113, -0.1624402480850797581, -16.17319339645315424 ) ) ;
#2717 = CARTESIAN_POINT ( 'NONE',  ( 123.4043428172204386, -3.870068077801122719, -15.96576694716182310 ) ) ;
#2718 = CARTESIAN_POINT ( 'NONE',  ( 118.2987481442453088, -7.894159318335828068, -9.358103419637847864 ) ) ;
#2719 = FACE_OUTER_BOUND ( 'NONE', #35178, .T. ) ;
#2720 = CARTESIAN_POINT ( 'NONE',  ( 117.3343948109119737, -6.222761293078241884, -8.102969835052219238 ) ) ;
#2721 = CARTESIAN_POINT ( 'NONE',  ( 117.0507614775786465, -10.30919188438810075, -12.61870101168855918 ) ) ;
#2722 = CARTESIAN_POINT ( 'NONE',  ( 121.9659548109119811, -2.527210466738041728, -8.967976844669124148 ) ) ;
#2723 = CARTESIAN_POINT ( 'NONE',  ( 113.1933481442453058, -4.089484607189486809, -7.948022111789456723 ) ) ;
#2724 = CARTESIAN_POINT ( 'NONE',  ( 114.2711548109119803, -0.1624402480850797581, -16.17319339645315424 ) ) ;
#2725 = CARTESIAN_POINT ( 'NONE',  ( 122.8368814775786291, -1.561330072975668948, -17.79121239304076951 ) ) ;
#2726 = AXIS2_PLACEMENT_3D ( 'NONE', #41402, #17220, #20195 ) ;
#2727 = CARTESIAN_POINT ( 'NONE',  ( 117.5045748109119756, -9.859900752359374465, -12.68260735090039404 ) ) ;
#2728 = EDGE_LOOP ( 'NONE', ( #24589, #42370, #39697, #41041, #8031 ) ) ;
#2729 = CARTESIAN_POINT ( 'NONE',  ( 112.0020881442453344, 0.2603800115204892296, -16.42320221600525088 ) ) ;
#2730 = CARTESIAN_POINT ( 'NONE',  ( 113.8857702545248003, -10.62599879583958717, -15.77991374673208469 ) ) ;
#2731 = ADVANCED_FACE ( 'NONE', ( #28250 ), #4742, .T. ) ;
#2732 = CARTESIAN_POINT ( 'NONE',  ( 106.1764733795248219, -1.325403438956436419, -9.854619843455211026 ) ) ;
#2733 = LINE ( 'NONE', #16658, #34177 ) ;
#2734 = CARTESIAN_POINT ( 'NONE',  ( 109.5102233795247884, -8.938348069036441856, -17.46756447353520869 ) ) ;
#2735 = CARTESIAN_POINT ( 'NONE',  ( 119.2063748109119814, -1.561330072975668504, -17.79121239304076951 ) ) ;
#2736 = ORIENTED_EDGE ( 'NONE', *, *, #23139, .F. ) ;
#2737 = CARTESIAN_POINT ( 'NONE',  ( 125.5030348109119558, -3.383040157471821630, -19.15922257007629170 ) ) ;
#2738 = CARTESIAN_POINT ( 'NONE',  ( 125.3328548109119964, -9.261995988541379177, -16.69588392320231307 ) ) ;
#2739 = CARTESIAN_POINT ( 'NONE',  ( 113.8173414775786512, -9.565557343593413364, -10.61323700422348004 ) ) ;
#2740 = ADVANCED_FACE ( 'NONE', ( #41500 ), #7791, .T. ) ;
#2741 = CARTESIAN_POINT ( 'NONE',  ( 124.7088614775786226, 0.2603800115204892296, -16.42320221600525088 ) ) ;
#2742 = EDGE_CURVE ( 'NONE', #41727, #37027, #24256, .T. ) ;
#2743 = CARTESIAN_POINT ( 'NONE',  ( 106.2459265045248173, -7.250697342233347165, -19.15521520033831138 ) ) ;
#2744 = CARTESIAN_POINT ( 'NONE',  ( 72.54180985774836188, -62.51387108299115170, -37.47916665824249804 ) ) ;
#2745 = VERTEX_POINT ( 'NONE', #70 ) ;
#2746 = FACE_OUTER_BOUND ( 'NONE', #2770, .T. ) ;
#2747 = CARTESIAN_POINT ( 'NONE',  ( 124.0848681442452772, -5.574606645277164318, -18.38911715685844683 ) ) ;
#2748 = CARTESIAN_POINT ( 'NONE',  ( 118.4122014775786340, 0.5811942927096110934, -14.16772938898807510 ) ) ;
#2749 = VECTOR ( 'NONE', #7883, 1000.000000000000000 ) ;
#2750 = CARTESIAN_POINT ( 'NONE',  ( 113.7606148109119886, -7.894159318335828068, -9.358103419637847864 ) ) ;
#2751 = CARTESIAN_POINT ( 'NONE',  ( 116.9373081442452929, -8.166667518702817929, -8.995218007635861213 ) ) ;
#2752 = DIRECTION ( 'NONE',  ( 1.000000000000000000, 0.000000000000000000, -0.000000000000000000 ) ) ;
#2753 = DIRECTION ( 'NONE',  ( -0.8636456077245080465, 0.5040994586965603652, 0.000000000000000000 ) ) ;
#2754 = CARTESIAN_POINT ( 'NONE',  ( 118.8660148109119774, 0.1319031606808879209, -14.10382304977623669 ) ) ;
#2755 = ORIENTED_EDGE ( 'NONE', *, *, #6941, .T. ) ;
#2756 = EDGE_CURVE ( 'NONE', #29406, #5805, #23817, .T. ) ;
#2757 = CARTESIAN_POINT ( 'NONE',  ( 123.9800954359119771, -11.07370829466463569, -12.81314460846529002 ) ) ;
#2758 = CARTESIAN_POINT ( 'NONE',  ( 112.3991748109119868, -8.166667518702817929, -8.995218007635859436 ) ) ;
#2759 = CARTESIAN_POINT ( 'NONE',  ( 122.8936081442453059, -9.565557343593413364, -10.61323700422348004 ) ) ;
#2760 = EDGE_LOOP ( 'NONE', ( #31215, #432, #27283, #35161 ) ) ;
#2761 = EDGE_CURVE ( 'NONE', #36562, #29748, #3265, .T. ) ;
#2762 = CARTESIAN_POINT ( 'NONE',  ( 120.8547048109119686, -2.527210466738041728, -8.967976844669124148 ) ) ;
#2763 = CARTESIAN_POINT ( 'NONE',  ( 137.3374356171238730, -0.3302559494014912223, -10.88373700413916900 ) ) ;
#2764 = EDGE_CURVE ( 'NONE', #19894, #21045, #30863, .T. ) ;
#2765 = ADVANCED_FACE ( 'NONE', ( #3491 ), #31297, .T. ) ;
#2766 = CARTESIAN_POINT ( 'NONE',  ( 117.7314814775786260, -4.089484607189486809, -7.948022111789456723 ) ) ;
#2767 = CARTESIAN_POINT ( 'NONE',  ( 114.0246765045248196, -7.250697342233347165, -19.15521520033831138 ) ) ;
#2768 = CARTESIAN_POINT ( 'NONE',  ( 116.0864081442453113, -0.1624402480850797581, -16.17319339645315424 ) ) ;
#2769 = ORIENTED_EDGE ( 'NONE', *, *, #28952, .T. ) ;
#2770 = EDGE_LOOP ( 'NONE', ( #24436, #33308, #33257, #30830 ) ) ;
#2771 = CARTESIAN_POINT ( 'NONE',  ( 124.3685014775786328, 0.4262465694468514643, -12.03445270309931736 ) ) ;
#2772 = CARTESIAN_POINT ( 'NONE',  ( 120.9649014775786355, -6.222761293078241884, -8.102969835052219238 ) ) ;
#2773 = DIRECTION ( 'NONE',  ( 0.000000000000000000, 0.000000000000000000, 1.000000000000000000 ) ) ;
#2774 = CARTESIAN_POINT ( 'NONE',  ( 86.09323753712084226, -26.60966817898065884, -11.90521360603286816 ) ) ;
#2775 = CARTESIAN_POINT ( 'NONE',  ( 121.8158014775786171, -5.638512984488999180, -18.83840828888717311 ) ) ;
#2776 = CARTESIAN_POINT ( 'NONE',  ( 111.5672066102589213, -9.129161674847271257, -16.62002394948158113 ) ) ;
#2777 = CIRCLE ( 'NONE', #23195, 2.999999999999999556 ) ;
#2778 = CARTESIAN_POINT ( 'NONE',  ( 117.1127004873411863, -2.348512537728064675, -17.99195118506216318 ) ) ;
#2779 = CARTESIAN_POINT ( 'NONE',  ( 119.2063748109119814, -1.561330072975668504, -17.79121239304076951 ) ) ;
#2781 = CARTESIAN_POINT ( 'NONE',  ( 120.1140014775786398, -7.894159318335828068, -9.358103419637847864 ) ) ;
#2780 = CARTESIAN_POINT ( 'NONE',  ( 119.2063748109119814, -1.561330072975668504, -17.79121239304076951 ) ) ;
#2782 = CARTESIAN_POINT ( 'NONE',  ( 125.2761281442453054, 0.4262465694468514643, -12.03445270309931736 ) ) ;
#2783 = CARTESIAN_POINT ( 'NONE',  ( 112.9097148109120070, 0.2603800115204892296, -16.42320221600525088 ) ) ;
#2784 = EDGE_LOOP ( 'NONE', ( #37832, #25173, #5289, #36988 ) ) ;
#2785 = CARTESIAN_POINT ( 'NONE',  ( 121.8725281442453223, -6.222761293078241884, -8.102969835052219238 ) ) ;
#2786 = CARTESIAN_POINT ( 'NONE',  ( 46.47434218039879283, -17.93412427487546523, -8.593215200338315540 ) ) ;
#2787 = FACE_OUTER_BOUND ( 'NONE', #19625, .T. ) ;
#2788 = CARTESIAN_POINT ( 'NONE',  ( 109.3713171295247832, -10.62599879583958540, -13.39321520033831447 ) ) ;
#2789 = CARTESIAN_POINT ( 'NONE',  ( 115.1359265045248605, -2.791137627527939813, -8.388885654883777576 ) ) ;
#2790 = CARTESIAN_POINT ( 'NONE',  ( 108.1211608795247798, -8.938348069036489818, -9.318865927141430916 ) ) ;
#2791 = CARTESIAN_POINT ( 'NONE',  ( 121.5888948109119809, -10.30919188438810075, -12.61870101168855918 ) ) ;
#2792 = CARTESIAN_POINT ( 'NONE',  ( 122.0994348109119443, -10.15424416112533912, -14.75197769757731336 ) ) ;
#2793 = ORIENTED_EDGE ( 'NONE', *, *, #28718, .T. ) ;
#2794 = CARTESIAN_POINT ( 'NONE',  ( 125.0492214775786266, -6.344957434206665248, -7.627207830600338134 ) ) ;
#2795 = CARTESIAN_POINT ( 'NONE',  ( 113.7038881442453402, -6.222761293078241884, -8.102969835052219238 ) ) ;
#2796 = CARTESIAN_POINT ( 'NONE',  ( 121.7023481442452919, -0.8288870151387517371, -10.36305467784176315 ) ) ;
#2797 = CARTESIAN_POINT ( 'NONE',  ( 119.2631014775786298, 0.2603800115204892296, -16.42320221600525088 ) ) ;
#2798 = B_SPLINE_CURVE_WITH_KNOTS ( 'NONE', 3,
 ( #31205, #41491, #37603, #20285, #17095, #6595, #34169, #23938, #30987, #20512, #38048, #6826, #13670, #27578, #23249, #37131, #5907, #21840, #4508, #32322, #21168, #42597, #11360, #41708, #17971, #25269, #41928, #39166 ),
 .UNSPECIFIED., .F., .F.,
 ( 4, 2, 2, 1, 1, 1, 1, 1, 2, 2, 2, 1, 1, 1, 1, 1, 2, 2, 4 ),
 ( 0.000000000000000000, 0.2499999999998344657, 0.3749999999997541411, 0.4374999999997165046, 0.4687499999996964650, 0.4843749999996863620, 0.4921874999996825317, 0.4960937499996794786, 0.4980468749996780353, 0.4999999999996767031, 0.6249999999994826361, 0.6874999999993886002, 0.7187499999993398614, 0.7343749999993155475, 0.7421874999993045563, 0.7460937499993005595, 0.7480468749993014477, 0.7499999999993022248, 1.000000000000000000 ),
 .UNSPECIFIED. ) ;
#2799 = CARTESIAN_POINT ( 'NONE',  ( 122.3263414775786373, -6.344957434206665248, -7.627207830600338134 ) ) ;
#2800 = CARTESIAN_POINT ( 'NONE',  ( 90.33554924625337890, -27.84333996136784961, -14.15691383771150136 ) ) ;
#2801 = CARTESIAN_POINT ( 'NONE',  ( 126.1270281442452870, 0.1319031606808879209, -14.10382304977623669 ) ) ;
#2802 = CARTESIAN_POINT ( 'NONE',  ( 111.9645664091100912, -0.9924539043446216624, -17.29976612834909133 ) ) ;
#2803 = ORIENTED_EDGE ( 'NONE', *, *, #25009, .T. ) ;
#2804 = CARTESIAN_POINT ( 'NONE',  ( 90.99708770779186295, -24.14644159042263993, -12.62951656296512937 ) ) ;
#2805 = CARTESIAN_POINT ( 'NONE',  ( 112.8529881442453302, -7.894159318335828068, -9.358103419637847864 ) ) ;
#2806 = CARTESIAN_POINT ( 'NONE',  ( 122.5532481442453019, 0.4262465694468514643, -12.03445270309931736 ) ) ;
#2807 = CARTESIAN_POINT ( 'NONE',  ( 107.3571765045248299, -2.791137627527939813, -8.388885654883777576 ) ) ;
#2808 = CARTESIAN_POINT ( 'NONE',  ( 113.4690515045247992, -6.936859964151250502, -18.39754474579286025 ) ) ;
#2809 = CARTESIAN_POINT ( 'NONE',  ( 118.5823814775786360, -7.643976991954077427, -18.09477374809248928 ) ) ;
#2810 = CARTESIAN_POINT ( 'NONE',  ( 114.6115148109119986, -6.222761293078241884, -8.102969835052219238 ) ) ;
#2811 = CARTESIAN_POINT ( 'NONE',  ( 124.7655881442452852, 0.5811942927096110934, -14.16772938898807510 ) ) ;
#2812 = ORIENTED_EDGE ( 'NONE', *, *, #4709, .F. ) ;
#2813 = ADVANCED_FACE ( 'NONE', ( #31081 ), #38144, .T. ) ;
#2814 = CARTESIAN_POINT ( 'NONE',  ( 122.3830681442452857, -1.833838273342659697, -17.42832698103878286 ) ) ;
#2815 = CARTESIAN_POINT ( 'NONE',  ( 118.5256548109119876, -0.4660016031367893996, -10.09054647747474043 ) ) ;
#2816 = CARTESIAN_POINT ( 'NONE',  ( 125.5030348109119558, -3.383040157471821630, -19.15922257007629170 ) ) ;
#2817 = CARTESIAN_POINT ( 'NONE',  ( 125.1626748109119802, -0.1624402480850797581, -16.17319339645315424 ) ) ;
#2818 = VERTEX_POINT ( 'NONE', #291 ) ;
#2819 = DIRECTION ( 'NONE',  ( 0.000000000000000000, 0.000000000000000000, 1.000000000000000000 ) ) ;
#2820 = CARTESIAN_POINT ( 'NONE',  ( 123.3474214775786209, -9.988377603198976828, -10.36322818467138340 ) ) ;
#2821 = CARTESIAN_POINT ( 'NONE',  ( 115.2922348109119781, 0.4262465694468514643, -12.03445270309931736 ) ) ;
#2822 = CARTESIAN_POINT ( 'NONE',  ( 125.3895814775786448, -7.893985811506177619, -18.51759400769804742 ) ) ;
#2823 = EDGE_CURVE ( 'NONE', #8410, #10961, #42247, .T. ) ;
#2824 = CYLINDRICAL_SURFACE ( 'NONE', #38413, 15.90000000000000036 ) ;
#2825 = CARTESIAN_POINT ( 'NONE',  ( 123.4939235609119663, -9.645473719204776586, -14.86997237629376656 ) ) ;
#2826 = ORIENTED_EDGE ( 'NONE', *, *, #14877, .T. ) ;
#2827 = DIRECTION ( 'NONE',  ( 0.000000000000000000, 0.9284778069183720062, 0.3713878862591650232 ) ) ;
#2828 = CARTESIAN_POINT ( 'NONE',  ( 89.70384154612264638, -12.43804770190545561, -13.24321520033830879 ) ) ;
#2829 = CARTESIAN_POINT ( 'NONE',  ( 109.7880358795247986, -8.402594152722688392, -9.854619843455216355 ) ) ;
#2830 = CARTESIAN_POINT ( 'NONE',  ( 114.9716510812576757, -0.01829820670803256055, -12.14321520033831625 ) ) ;
#2831 = CARTESIAN_POINT ( 'NONE',  ( 123.4608748109119745, 0.4262465694468514643, -12.03445270309931736 ) ) ;
#2832 = CARTESIAN_POINT ( 'NONE',  ( 114.9518748109119883, -7.643976991954077427, -18.09477374809248928 ) ) ;
#2833 = CARTESIAN_POINT ( 'NONE',  ( 126.7702028005115125, -0.1768172365690781900, -10.97118840898372660 ) ) ;
#2834 = ORIENTED_EDGE ( 'NONE', *, *, #21144, .F. ) ;
#2835 = CARTESIAN_POINT ( 'NONE',  ( 128.2184548109119930, -1.889072916127989776, -18.60376373290417362 ) ) ;
#2836 = CARTESIAN_POINT ( 'NONE',  ( 120.2841814775786276, -10.15424416112533912, -14.75197769757731336 ) ) ;
#2837 = CARTESIAN_POINT ( 'NONE',  ( 112.7962614775786676, -6.222761293078241884, -8.102969835052219238 ) ) ;
#2838 = CARTESIAN_POINT ( 'NONE',  ( 91.65862616933031859, -25.99489077589524300, -13.39321520033831447 ) ) ;
#2839 = CARTESIAN_POINT ( 'NONE',  ( 70.19189222814998175, -100.0979043305785581, -53.24182196210380624 ) ) ;
#2841 = CARTESIAN_POINT ( 'NONE',  ( 124.9357681442453014, -1.834011780172310813, -8.268836392978581529 ) ) ;
#2840 = CARTESIAN_POINT ( 'NONE',  ( 114.2334337908067710, 0.5115630086001619059, -12.14321520033831625 ) ) ;
#2842 = AXIS2_PLACEMENT_3D ( 'NONE', #25697, #1511, #1733 ) ;
#2843 = CARTESIAN_POINT ( 'NONE',  ( 112.3991748109119868, -8.166667518702817929, -8.995218007635859436 ) ) ;
#2844 = VERTEX_POINT ( 'NONE', #20387 ) ;
#2845 = CARTESIAN_POINT ( 'NONE',  ( 113.8740681442453138, 0.5811942927096154232, -14.16772938898807155 ) ) ;
#2846 = CARTESIAN_POINT ( 'NONE',  ( 128.2184548109119930, 0.6402711692277476274, -15.78131322003126868 ) ) ;
#2847 = CARTESIAN_POINT ( 'NONE',  ( 107.2182702545248105, 0.1403307496149616695, -11.32035403202665336 ) ) ;
#2848 = CARTESIAN_POINT ( 'NONE',  ( 124.3685014775786328, 0.4262465694468514643, -12.03445270309931736 ) ) ;
#2849 = CARTESIAN_POINT ( 'NONE',  ( 122.8368814775786291, -7.894159318335828068, -9.358103419637847864 ) ) ;
#2850 = DIRECTION ( 'NONE',  ( 0.3127730236694482580, -0.9498278979187074755, 0.000000000000000000 ) ) ;
#2851 = CARTESIAN_POINT ( 'NONE',  ( 114.7886608795247696, -1.325403438956436419, -16.93181055722141792 ) ) ;
#2852 = DIRECTION ( 'NONE',  ( -0.000000000000000000, -0.000000000000000000, 1.000000000000000000 ) ) ;
#2853 = CARTESIAN_POINT ( 'NONE',  ( 120.0907204359119760, -10.25716656981731489, -12.88942061488890545 ) ) ;
#2854 = FACE_OUTER_BOUND ( 'NONE', #2897, .T. ) ;
#2855 = CARTESIAN_POINT ( 'NONE',  ( 87.44708369096657918, -25.99489077589588604, -13.39321520033831447 ) ) ;
#2856 = CARTESIAN_POINT ( 'NONE',  ( 31.16203868753470019, 11.28474725185576055, -17.89321520033831447 ) ) ;
#2857 = CARTESIAN_POINT ( 'NONE',  ( 112.3578015045248861, -2.477300249445798297, -7.631215200338321125 ) ) ;
#2858 = CARTESIAN_POINT ( 'NONE',  ( 125.4463081442452932, -5.638512984488999180, -18.83840828888717311 ) ) ;
#2859 = CARTESIAN_POINT ( 'NONE',  ( 123.5176014775786228, -9.261995988541697145, -16.69588392320189030 ) ) ;
#2860 = DIRECTION ( 'NONE',  ( 1.000000000000000000, 0.000000000000000000, 0.000000000000000000 ) ) ;
#2861 =( BOUNDED_CURVE ( )  B_SPLINE_CURVE ( 3, ( #30022, #33413, #2647, #9281 ),
 .UNSPECIFIED., .F., .T. ) 
 B_SPLINE_CURVE_WITH_KNOTS ( ( 4, 4 ),
 ( 2.411864997362825225, 3.141592653589795336 ),
 .UNSPECIFIED. ) 
 CURVE ( )  GEOMETRIC_REPRESENTATION_ITEM ( )  RATIONAL_B_SPLINE_CURVE ( ( 1.000000000000000000, 0.9561149059751439250, 0.9561149059751439250, 1.000000000000000000 ) ) 
 REPRESENTATION_ITEM ( '' )  );
#2862 = CARTESIAN_POINT ( 'NONE',  ( 118.6958348109119754, -6.344957434206665248, -7.627207830600338134 ) ) ;
#2863 = CARTESIAN_POINT ( 'NONE',  ( 93.24708369096698846, -27.84333996136784961, -14.15691383771150136 ) ) ;
#2865 = VERTEX_POINT ( 'NONE', #13544 ) ;
#2864 = ADVANCED_FACE ( 'NONE', ( #7351 ), #27897, .T. ) ;
#2866 = CARTESIAN_POINT ( 'NONE',  ( 114.1009748109119784, -5.574606645277164318, -18.38911715685844683 ) ) ;
#2867 = CARTESIAN_POINT ( 'NONE',  ( 112.1155414775786454, -10.15424416112533912, -14.75197769757731336 ) ) ;
#2868 = CARTESIAN_POINT ( 'NONE',  ( 122.8368814775786291, -1.561330072975668948, -17.79121239304076951 ) ) ;
#2869 = CARTESIAN_POINT ( 'NONE',  ( 115.9729548109119861, -6.344957434206662583, -7.627207830600332805 ) ) ;
#2870 = ITEM_DEFINED_TRANSFORMATION ( 'NONE', 'NONE', #44624,  #12375 ) ;
#2871 = CARTESIAN_POINT ( 'NONE',  ( 126.0135748109119902, -8.166667518702819706, -8.995218007635861213 ) ) ;
#2872 = ORIENTED_EDGE ( 'NONE', *, *, #44296, .T. ) ;
#2873 = CARTESIAN_POINT ( 'NONE',  ( 116.4267681442453153, -6.222761293078241884, -8.102969835052219238 ) ) ;
#2874 = CARTESIAN_POINT ( 'NONE',  ( 112.7395348109119766, -5.638512984488999180, -18.83840828888717311 ) ) ;
#2875 = CARTESIAN_POINT ( 'NONE',  ( 112.4272546295247821, -4.863998795839590272, -18.39754474579285315 ) ) ;
#2876 = EDGE_CURVE ( 'NONE', #13043, #17886, #27453, .T. ) ;
#2877 = CIRCLE ( 'NONE', #26965, 1.610000000000000986 ) ;
#2878 = CARTESIAN_POINT ( 'NONE',  ( 122.3830681442452857, -1.833838273342659697, -17.42832698103878286 ) ) ;
#2879 = CARTESIAN_POINT ( 'NONE',  ( 124.0527235609119714, -0.08666061303663243065, -11.91773565553389425 ) ) ;
#2880 = CARTESIAN_POINT ( 'NONE',  ( 112.4272546295247821, -4.863998795839590272, -7.631215200338315796 ) ) ;
#2881 = ORIENTED_EDGE ( 'NONE', *, *, #1026, .T. ) ;
#2882 = CIRCLE ( 'NONE', #32701, 4.999999999999998224 ) ;
#2883 = CARTESIAN_POINT ( 'NONE',  ( 66.07656475110815109, -2.141145020708993929, -8.744744089885024607 ) ) ;
#2884 = CARTESIAN_POINT ( 'NONE',  ( 112.9327801496069696, 0.3591747506842615789, -14.64321520033830026 ) ) ;
#2885 = LINE ( 'NONE', #2198, #24754 ) ;
#2886 = DIRECTION ( 'NONE',  ( -8.728168432587710164E-16, -1.000000000000000000, 0.000000000000000000 ) ) ;
#2887 = CARTESIAN_POINT ( 'NONE',  ( 122.9382985609119743, -10.36940331770107093, -15.09355782777061350 ) ) ;
#2888 = CARTESIAN_POINT ( 'NONE',  ( 113.7722331777918896, -0.01829820670813664396, -14.64321520033831447 ) ) ;
#2889 = CARTESIAN_POINT ( 'NONE',  ( 105.8986608795248401, -1.325403438956436419, -16.93181055722141792 ) ) ;
#2890 = FACE_BOUND ( 'NONE', #40393, .T. ) ;
#2891 = CARTESIAN_POINT ( 'NONE',  ( 119.7736414775786358, -10.30919188438810075, -12.61870101168855918 ) ) ;
#2892 = CARTESIAN_POINT ( 'NONE',  ( 136.7407071004454338, -4.349533742155984761, -18.99919027275945282 ) ) ;
#2893 = DIRECTION ( 'NONE',  ( 0.000000000000000000, 0.000000000000000000, 1.000000000000000000 ) ) ;
#2894 = ADVANCED_FACE ( 'NONE', ( #41375 ), #10569, .T. ) ;
#2895 = CARTESIAN_POINT ( 'NONE',  ( 124.0495485609119726, -0.08252387247379561197, -11.91645802438259771 ) ) ;
#2896 = CARTESIAN_POINT ( 'NONE',  ( 121.1918081442452859, -10.15424416112533912, -14.75197769757731336 ) ) ;
#2897 = EDGE_LOOP ( 'NONE', ( #25166, #9378, #14886, #18310 ) ) ;
#2898 = CARTESIAN_POINT ( 'NONE',  ( 125.5597614775786326, -1.561330072975669392, -17.79121239304076951 ) ) ;
#2899 = CARTESIAN_POINT ( 'NONE',  ( 120.5110881442453206, -6.344957434206665248, -7.627207830600338134 ) ) ;
#2900 = CARTESIAN_POINT ( 'NONE',  ( 62.57015527438819191, -24.33598972801448923, -4.893215200338314474 ) ) ;
#2901 = CARTESIAN_POINT ( 'NONE',  ( 116.3700414775786527, -4.153390946401321671, -8.397313243818183892 ) ) ;
#2902 = CARTESIAN_POINT ( 'NONE',  ( 123.8012348109119642, 0.2603800115204892296, -16.42320221600525088 ) ) ;
#2903 = CARTESIAN_POINT ( 'NONE',  ( 109.7185827545247889, -2.477300249445798297, -19.15521520033831138 ) ) ;
#2904 = CARTESIAN_POINT ( 'NONE',  ( 61.85703706989207973, -38.82652229419164769, -6.037231199156998684 ) ) ;
#2905 = FACE_OUTER_BOUND ( 'NONE', #38733, .T. ) ;
#2906 = CARTESIAN_POINT ( 'NONE',  ( 116.0296814775786345, -1.833838273342658809, -17.42832698103878286 ) ) ;
#2907 = CARTESIAN_POINT ( 'NONE',  ( 117.7314814775786260, -5.574606645277164318, -18.38911715685844683 ) ) ;
#2908 = DIRECTION ( 'NONE',  ( 0.000000000000000000, -0.3818493186865927203, 0.9242245927363029745 ) ) ;
#2909 = CARTESIAN_POINT ( 'NONE',  ( 115.2053796295247849, -4.863998795839590272, -8.388885654883775800 ) ) ;
#2910 = ORIENTED_EDGE ( 'NONE', *, *, #16133, .T. ) ;
#2911 = DIRECTION ( 'NONE',  ( 0.7202110682883375858, 0.2576522076061144029, -0.6441361323747234469 ) ) ;
#2912 = CARTESIAN_POINT ( 'NONE',  ( 114.6115148109119986, -3.383040157471821630, -19.15922257007629170 ) ) ;
#2913 = DIRECTION ( 'NONE',  ( -1.000000000000000000, 0.000000000000000000, -0.000000000000000000 ) ) ;
#2914 = CARTESIAN_POINT ( 'NONE',  ( 122.7993923109119692, -0.4387604401700512802, -15.73000352943951619 ) ) ;
#2915 = CARTESIAN_POINT ( 'NONE',  ( 121.2019704359119743, -10.25716656981731489, -12.88942061488890545 ) ) ;
#2916 = VERTEX_POINT ( 'NONE', #37925 ) ;
#2917 = DIRECTION ( 'NONE',  ( -0.000000000000000000, -0.9284778069183721172, -0.3713878862591650232 ) ) ;
#2918 = CARTESIAN_POINT ( 'NONE',  ( 105.3430358795248338, -8.402594152722688392, -9.854619843455216355 ) ) ;
#2919 = ORIENTED_EDGE ( 'NONE', *, *, #17248, .F. ) ;
#2920 = CARTESIAN_POINT ( 'NONE',  ( 119.1496481442453046, -3.383040157471821630, -19.15922257007629170 ) ) ;
#2921 = CIRCLE ( 'NONE', #20410, 1.499999999999996225 ) ;
#2922 = CARTESIAN_POINT ( 'NONE',  ( 114.4413348109119823, -9.261995988541697145, -16.69588392320189030 ) ) ;
#2923 = CARTESIAN_POINT ( 'NONE',  ( 118.0151148109119816, 0.4262465694468514643, -12.03445270309931736 ) ) ;
#2924 = PRESENTATION_STYLE_ASSIGNMENT (( #2238 ) ) ;
#2925 = AXIS2_PLACEMENT_3D ( 'NONE', #18987, #8724, #11703 ) ;
#2926 = CARTESIAN_POINT ( 'NONE',  ( 61.63318325272354770, -19.46990085680238636, -15.89321520033831447 ) ) ;
#2927 = CARTESIAN_POINT ( 'NONE',  ( 120.0572748109119772, -3.383040157471821630, -19.15922257007629170 ) ) ;
#2928 = CARTESIAN_POINT ( 'NONE',  ( 116.8805814775786445, -6.344957434206662583, -7.627207830600332805 ) ) ;
#2929 = CARTESIAN_POINT ( 'NONE',  ( 106.1070202545248407, 0.1403307496149616695, -11.32035403202665336 ) ) ;
#2930 = ADVANCED_FACE ( 'NONE', ( #45008 ), #41907, .T. ) ;
#2931 = CARTESIAN_POINT ( 'NONE',  ( 112.5693548109119888, 0.4262465694468514643, -12.03445270309931736 ) ) ;
#2932 = CARTESIAN_POINT ( 'NONE',  ( 125.0849635773846842, -2.467220198597905867, -17.83387418641800437 ) ) ;
#2933 = VERTEX_POINT ( 'NONE', #21043 ) ;
#2934 = CARTESIAN_POINT ( 'NONE',  ( 117.1074881442453233, -10.63000616557722466, -14.87417383870573495 ) ) ;
#2935 = FACE_OUTER_BOUND ( 'NONE', #42752, .T. ) ;
#2936 = CARTESIAN_POINT ( 'NONE',  ( 116.3133148109119759, -7.893985811506177619, -18.51759400769804742 ) ) ;
#2937 = ORIENTED_EDGE ( 'NONE', *, *, #31128, .F. ) ;
#2938 = CARTESIAN_POINT ( 'NONE',  ( 122.4397948109119767, -9.988377603198976828, -10.36322818467138340 ) ) ;
#2939 = AXIS2_PLACEMENT_3D ( 'NONE', #32208, #7594, #14897 ) ;
#2940 = CARTESIAN_POINT ( 'NONE',  ( 96.46827370896536991, -25.18754255092518335, -13.99861390895580371 ) ) ;
#2941 = CARTESIAN_POINT ( 'NONE',  ( 113.1933481442453058, -5.574606645277164318, -18.38911715685844683 ) ) ;
#2942 =( BOUNDED_SURFACE ( )  B_SPLINE_SURFACE ( 1, 2, ( 
 ( #21336, #41213, #24103, #41660, #44858, #10860, #14053, #38643, #20458, #3116, #30935, #20900, #13612, #27522, #10196, #6771, #34557, #27969, #10636, #3341, #27745, #24540, #7197, #24325, #17260, #31149, #45070, #3770, #21108, #34984, #17694, #361, #31814, #35448, #585, #11303, #28409, #15396, #32482, #7646, #32703, #7879, #29300, #42985, #25212, #1474, #11533, #42318, #25661, #21787, #24982, #11079, #17917, #4452, #14495, #38876, #8330, #43213, #11980, #28635, #36125, #28858, #35678, #25882, #39784, #8107, #4223, #21561, #42542, #29074, #22454, #35904, #39111, #18141, #32036, #8553, #4894, #36348, #22008, #1256, #11752, #18811, #804, #25440, #14722, #39566, #42770, #18374, #15167, #32262, #39341, #1030, #14947, #4669, #22229, #18591, #12890, #33832, #19944, #2601, #1921, #33370, #29744, #2373, #43440, #23601, #19488, #19711, #12661, #2140, #12204, #26332, #9233, #15849, #37022, #26559, #26102, #5119, #44349, #16533, #9008, #30430, #5352, #19035, #29975, #32922, #40009, #13109, #30204, #33597, #8774, #1698, #15618, #22678, #29524, #16071, #36576, #40472, #9684, #6021, #19268, #33147, #43657, #5792, #27014, #22905, #36798, #12433, #40239, #40697, #5566, #43892, #23142, #16303, #44125, #26788, #40931, #9453, #23367, #37248, #44575, #3505, #7147, #10142, #14001, #10587, #10807, #13781, #6490, #20404, #3723, #27917, #41827, #41389, #24487, #38375, #21058, #42047, #309, #34936, #17642, #6717, #27693, #37486, #23833, #20628, #34505, #41610, #3283, #14223, #37719, #6260, #31314, #31540, #28138, #20180, #10365, #34065, #34289, #2831, #17205, #27469, #16760, #31098, #27244, #24273, #20843, #30657, #13340, #45023, #38161, #6937, #41158, #9919, #3061, #44800, #16989, #34722, #17422, #89, #24051, #37944, #30880, #13559, #11254, #35168, #25163, #14671, #1422, #3944, #15122, #21282, #14446, #42718, #25390, #22180, #11701, #15342, #28809, #39286, #18542, #25612, #4847, #32209, #29251, #1208, #4401, #38827, #8053, #536, #18317, #4173, #39515, #35626, #29028, #7831, #32434 ),
 ( #17867, #43160, #39060, #11484, #28585, #28353, #24702, #8278, #18091, #42266, #42939, #35847, #21509, #21959, #36076, #7595, #18766, #32655, #11031, #21737, #983, #14898, #31984, #38592, #7369, #31764, #747, #4621, #35397, #24930, #42495, #9397, #19890, #5067, #29469, #19433, #18983, #15565, #23308, #39959, #22627, #2092, #9177, #8721, #8954, #12607, #33318, #22854, #40642, #43384, #2547, #30152, #23084, #30377, #43606, #25826, #39733, #12152, #8502, #5298, #22406, #37192, #26509, #1641, #26734, #1864, #5966, #36965, #19214, #33777, #5513, #36299, #19655, #15793, #32872, #26055, #11928, #12382, #36525, #33094, #2321, #16474, #29695, #26280, #44068, #36745, #40188, #16018, #29926, #43840, #40417, #5736, #33542, #16249, #12834, #17156, #6441, #9628, #30599, #10530, #13508, #34234, #41770, #27416, #34009, #20572, #27639, #26953, #20791, #37886, #31043, #6662, #21008, #3670, #41107, #20350, #6202, #23998, #34449, #41553, #3008, #44749, #17374, #40875, #30825, #23549, #41336, #16930, #34882, #37432, #34671, #20124, #2780, #44973, #13730, #10313, #3230, #10095, #16705, #24215, #38106, #9865, #6881, #3457, #44516, #44299, #38321, #24429, #31262, #7098, #13281, #13054, #35, #17591, #27187, #23774, #13947, #27860, #37666, #28081, #254, #38537, #14163, #14613, #41989, #39001, #36639, #32985, #7312, #21231, #17811, #32155, #1759, #4110, #35338, #42212, #10754, #22516, #24876, #21455, #4339, #35566, #5412, #11428, #15685, #38768, #22737, #18031, #35110, #42657, #29587, #31928, #8619, #5181, #31484, #7771, #475, #14388, #43505, #36412, #19098, #693, #12272, #26169, #40074, #24652, #8838, #3891, #31705, #28530, #21678, #28300, #10973, #42436, #11200, #18259, #25105, #7538, #923, #14842, #25947, #28752, #39854, #33214, #9515, #16824, #33428, #1988, #44188, #37775, #26394, #30717, #44408, #33892, #40304, #15914, #29812, #9067, #43728, #2437, #12496, #26846, #23892, #20239, #22970, #36860, #5630, #20006, #34125, #37081, #23203, #30037, #19550, #9751, #12717, #9295, #37317 ) ),
 .UNSPECIFIED., .F., .F., .F. ) 
 B_SPLINE_SURFACE_WITH_KNOTS ( ( 2, 2 ),
 ( 3, 2, 2, 2, 2, 2, 2, 2, 2, 2, 2, 2, 2, 2, 2, 2, 2, 2, 2, 2, 2, 2, 2, 2, 2, 2, 2, 2, 2, 2, 2, 2, 2, 2, 2, 2, 2, 2, 2, 2, 2, 2, 2, 2, 2, 2, 2, 2, 2, 2, 2, 2, 2, 2, 2, 2, 2, 2, 2, 2, 2, 2, 2, 2, 2, 2, 2, 2, 2, 2, 2, 2, 2, 2, 2, 2, 2, 2, 2, 2, 2, 2, 2, 2, 2, 2, 2, 2, 2, 2, 2, 2, 2, 2, 2, 2, 2, 2, 2, 2, 2, 2, 2, 2, 2, 2, 2, 2, 2, 2, 2, 2, 2, 2, 2, 2, 2, 2, 2, 2, 2, 2, 2, 2, 2, 2, 2, 2, 3 ),
 ( 0.000000000000000000, 1.000000000000000000 ),
 ( 0.000000000000000000, 0.007812500000000000000, 0.01562500000000000000, 0.02343750000000000000, 0.03125000000000000000, 0.03906250000000000000, 0.04687500000000000000, 0.05468750000000000000, 0.06250000000000000000, 0.07031250000000000000, 0.07812500000000000000, 0.08593750000000000000, 0.09375000000000000000, 0.1015625000000000000, 0.1093750000000000000, 0.1171875000000000000, 0.1250000000000000000, 0.1328125000000000000, 0.1406250000000000000, 0.1484375000000000000, 0.1562500000000000000, 0.1640625000000000000, 0.1718750000000000000, 0.1796875000000000000, 0.1875000000000000000, 0.1953125000000000000, 0.2031250000000000000, 0.2109375000000000000, 0.2187500000000000000, 0.2265625000000000000, 0.2343750000000000000, 0.2421875000000000000, 0.2500000000000000000, 0.2578125000000000000, 0.2656250000000000000, 0.2734375000000000000, 0.2812500000000000000, 0.2890625000000000000, 0.2968750000000000000, 0.3046875000000000000, 0.3125000000000000000, 0.3203125000000000000, 0.3281250000000000000, 0.3359375000000000000, 0.3437500000000000000, 0.3515625000000000000, 0.3593750000000000000, 0.3671875000000000000, 0.3750000000000000000, 0.3828125000000000000, 0.3906250000000000000, 0.3984375000000000000, 0.4062500000000000000, 0.4140625000000000000, 0.4218750000000000000, 0.4296875000000000000, 0.4375000000000000000, 0.4453125000000000000, 0.4531250000000000000, 0.4609375000000000000, 0.4687500000000000000, 0.4765625000000000000, 0.4843750000000000000, 0.4921875000000000000, 0.5000000000000000000, 0.5078125000000000000, 0.5156250000000000000, 0.5234375000000000000, 0.5312500000000000000, 0.5390625000000000000, 0.5468750000000000000, 0.5546875000000000000, 0.5625000000000000000, 0.5703125000000000000, 0.5781250000000000000, 0.5859375000000000000, 0.5937500000000000000, 0.6015625000000000000, 0.6093750000000000000, 0.6171875000000000000, 0.6250000000000000000, 0.6328125000000000000, 0.6406250000000000000, 0.6484375000000000000, 0.6562500000000000000, 0.6640625000000000000, 0.6718750000000000000, 0.6796875000000000000, 0.6875000000000000000, 0.6953125000000000000, 0.7031250000000000000, 0.7109375000000000000, 0.7187500000000000000, 0.7265625000000000000, 0.7343750000000000000, 0.7421875000000000000, 0.7500000000000000000, 0.7578125000000000000, 0.7656250000000000000, 0.7734375000000000000, 0.7812500000000000000, 0.7890625000000000000, 0.7968750000000000000, 0.8046875000000000000, 0.8125000000000000000, 0.8203125000000000000, 0.8281250000000000000, 0.8359375000000000000, 0.8437500000000000000, 0.8515625000000000000, 0.8593750000000000000, 0.8671875000000000000, 0.8750000000000000000, 0.8828125000000000000, 0.8906250000000000000, 0.8984375000000000000, 0.9062500000000000000, 0.9140625000000000000, 0.9218750000000000000, 0.9296875000000000000, 0.9375000000000000000, 0.9453125000000000000, 0.9531250000000000000, 0.9609375000000000000, 0.9687500000000000000, 0.9765625000000000000, 0.9843750000000000000, 0.9921875000000000000, 1.000000000000000000 ),
 .UNSPECIFIED. ) 
 GEOMETRIC_REPRESENTATION_ITEM ( )  RATIONAL_B_SPLINE_SURFACE ( (
 ( 1.000000000000000000, 0.9238795325112869605, 1.000000000000000000, 0.9238795325112869605, 1.000000000000000000, 0.9238795325112869605, 1.000000000000000000, 0.9238795325112869605, 1.000000000000000000, 0.9238795325112869605, 1.000000000000000000, 0.9238795325112869605, 1.000000000000000000, 0.9238795325112869605, 1.000000000000000000, 0.9238795325112869605, 1.000000000000000000, 0.9238795325112869605, 1.000000000000000000, 0.9238795325112869605, 1.000000000000000000, 0.9238795325112869605, 1.000000000000000000, 0.9238795325112869605, 1.000000000000000000, 0.9238795325112869605, 1.000000000000000000, 0.9238795325112869605, 1.000000000000000000, 0.9238795325112869605, 1.000000000000000000, 0.9238795325112869605, 1.000000000000000000, 0.9238795325112869605, 1.000000000000000000, 0.9238795325112869605, 1.000000000000000000, 0.9238795325112869605, 1.000000000000000000, 0.9238795325112869605, 1.000000000000000000, 0.9238795325112869605, 1.000000000000000000, 0.9238795325112869605, 1.000000000000000000, 0.9238795325112869605, 1.000000000000000000, 0.9238795325112869605, 1.000000000000000000, 0.9238795325112869605, 1.000000000000000000, 0.9238795325112869605, 1.000000000000000000, 0.9238795325112869605, 1.000000000000000000, 0.9238795325112869605, 1.000000000000000000, 0.9238795325112869605, 1.000000000000000000, 0.9238795325112869605, 1.000000000000000000, 0.9238795325112869605, 1.000000000000000000, 0.9238795325112869605, 1.000000000000000000, 0.9238795325112869605, 1.000000000000000000, 0.9238795325112869605, 1.000000000000000000, 0.9238795325112869605, 1.000000000000000000, 0.9238795325112869605, 1.000000000000000000, 0.9238795325112869605, 1.000000000000000000, 0.9238795325112869605, 1.000000000000000000, 0.9238795325112869605, 1.000000000000000000, 0.9238795325112869605, 1.000000000000000000, 0.9238795325112869605, 1.000000000000000000, 0.9238795325112869605, 1.000000000000000000, 0.9238795325112869605, 1.000000000000000000, 0.9238795325112869605, 1.000000000000000000, 0.9238795325112869605, 1.000000000000000000, 0.9238795325112869605, 1.000000000000000000, 0.9238795325112869605, 1.000000000000000000, 0.9238795325112869605, 1.000000000000000000, 0.9238795325112869605, 1.000000000000000000, 0.9238795325112869605, 1.000000000000000000, 0.9238795325112869605, 1.000000000000000000, 0.9238795325112869605, 1.000000000000000000, 0.9238795325112869605, 1.000000000000000000, 0.9238795325112869605, 1.000000000000000000, 0.9238795325112869605, 1.000000000000000000, 0.9238795325112869605, 1.000000000000000000, 0.9238795325112869605, 1.000000000000000000, 0.9238795325112869605, 1.000000000000000000, 0.9238795325112869605, 1.000000000000000000, 0.9238795325112869605, 1.000000000000000000, 0.9238795325112869605, 1.000000000000000000, 0.9238795325112869605, 1.000000000000000000, 0.9238795325112869605, 1.000000000000000000, 0.9238795325112869605, 1.000000000000000000, 0.9238795325112869605, 1.000000000000000000, 0.9238795325112869605, 1.000000000000000000, 0.9238795325112869605, 1.000000000000000000, 0.9238795325112869605, 1.000000000000000000, 0.9238795325112869605, 1.000000000000000000, 0.9238795325112869605, 1.000000000000000000, 0.9238795325112869605, 1.000000000000000000, 0.9238795325112869605, 1.000000000000000000, 0.9238795325112869605, 1.000000000000000000, 0.9238795325112869605, 1.000000000000000000, 0.9238795325112869605, 1.000000000000000000, 0.9238795325112869605, 1.000000000000000000, 0.9238795325112869605, 1.000000000000000000, 0.9238795325112869605, 1.000000000000000000, 0.9238795325112869605, 1.000000000000000000, 0.9238795325112869605, 1.000000000000000000, 0.9238795325112869605, 1.000000000000000000, 0.9238795325112869605, 1.000000000000000000, 0.9238795325112869605, 1.000000000000000000, 0.9238795325112869605, 1.000000000000000000, 0.9238795325112869605, 1.000000000000000000, 0.9238795325112869605, 1.000000000000000000, 0.9238795325112869605, 1.000000000000000000, 0.9238795325112869605, 1.000000000000000000, 0.9238795325112869605, 1.000000000000000000, 0.9238795325112869605, 1.000000000000000000, 0.9238795325112869605, 1.000000000000000000, 0.9238795325112869605, 1.000000000000000000, 0.9238795325112869605, 1.000000000000000000, 0.9238795325112869605, 1.000000000000000000, 0.9238795325112869605, 1.000000000000000000, 0.9238795325112869605, 1.000000000000000000, 0.9238795325112869605, 1.000000000000000000, 0.9238795325112869605, 1.000000000000000000, 0.9238795325112869605, 1.000000000000000000, 0.9238795325112869605, 1.000000000000000000, 0.9238795325112869605, 1.000000000000000000, 0.9238795325112869605, 1.000000000000000000, 0.9238795325112869605, 1.000000000000000000, 0.9238795325112869605, 1.000000000000000000, 0.9238795325112869605, 1.000000000000000000, 0.9238795325112869605, 1.000000000000000000, 0.9238795325112869605, 1.000000000000000000, 0.9238795325112869605, 1.000000000000000000, 0.9238795325112869605, 1.000000000000000000, 0.9238795325112869605, 1.000000000000000000, 0.9238795325112869605, 1.000000000000000000, 0.9238795325112869605, 1.000000000000000000, 0.9238795325112869605, 1.000000000000000000, 0.9238795325112869605, 1.000000000000000000, 0.9238795325112869605, 1.000000000000000000, 0.9238795325112869605, 1.000000000000000000, 0.9238795325112869605, 1.000000000000000000, 0.9238795325112869605, 1.000000000000000000, 0.9238795325112869605, 1.000000000000000000, 0.9238795325112869605, 1.000000000000000000, 0.9238795325112869605, 1.000000000000000000, 0.9238795325112869605, 1.000000000000000000, 0.9238795325112869605, 1.000000000000000000, 0.9238795325112869605, 1.000000000000000000, 0.9238795325112869605, 1.000000000000000000, 0.9238795325112869605, 1.000000000000000000, 0.9238795325112869605, 1.000000000000000000, 0.9238795325112869605, 1.000000000000000000),
 ( 1.000000000000000000, 0.9238795325112869605, 1.000000000000000000, 0.9238795325112869605, 1.000000000000000000, 0.9238795325112869605, 1.000000000000000000, 0.9238795325112869605, 1.000000000000000000, 0.9238795325112869605, 1.000000000000000000, 0.9238795325112869605, 1.000000000000000000, 0.9238795325112869605, 1.000000000000000000, 0.9238795325112869605, 1.000000000000000000, 0.9238795325112869605, 1.000000000000000000, 0.9238795325112869605, 1.000000000000000000, 0.9238795325112869605, 1.000000000000000000, 0.9238795325112869605, 1.000000000000000000, 0.9238795325112869605, 1.000000000000000000, 0.9238795325112869605, 1.000000000000000000, 0.9238795325112869605, 1.000000000000000000, 0.9238795325112869605, 1.000000000000000000, 0.9238795325112869605, 1.000000000000000000, 0.9238795325112869605, 1.000000000000000000, 0.9238795325112869605, 1.000000000000000000, 0.9238795325112869605, 1.000000000000000000, 0.9238795325112869605, 1.000000000000000000, 0.9238795325112869605, 1.000000000000000000, 0.9238795325112869605, 1.000000000000000000, 0.9238795325112869605, 1.000000000000000000, 0.9238795325112869605, 1.000000000000000000, 0.9238795325112869605, 1.000000000000000000, 0.9238795325112869605, 1.000000000000000000, 0.9238795325112869605, 1.000000000000000000, 0.9238795325112869605, 1.000000000000000000, 0.9238795325112869605, 1.000000000000000000, 0.9238795325112869605, 1.000000000000000000, 0.9238795325112869605, 1.000000000000000000, 0.9238795325112869605, 1.000000000000000000, 0.9238795325112869605, 1.000000000000000000, 0.9238795325112869605, 1.000000000000000000, 0.9238795325112869605, 1.000000000000000000, 0.9238795325112869605, 1.000000000000000000, 0.9238795325112869605, 1.000000000000000000, 0.9238795325112869605, 1.000000000000000000, 0.9238795325112869605, 1.000000000000000000, 0.9238795325112869605, 1.000000000000000000, 0.9238795325112869605, 1.000000000000000000, 0.9238795325112869605, 1.000000000000000000, 0.9238795325112869605, 1.000000000000000000, 0.9238795325112869605, 1.000000000000000000, 0.9238795325112869605, 1.000000000000000000, 0.9238795325112869605, 1.000000000000000000, 0.9238795325112869605, 1.000000000000000000, 0.9238795325112869605, 1.000000000000000000, 0.9238795325112869605, 1.000000000000000000, 0.9238795325112869605, 1.000000000000000000, 0.9238795325112869605, 1.000000000000000000, 0.9238795325112869605, 1.000000000000000000, 0.9238795325112869605, 1.000000000000000000, 0.9238795325112869605, 1.000000000000000000, 0.9238795325112869605, 1.000000000000000000, 0.9238795325112869605, 1.000000000000000000, 0.9238795325112869605, 1.000000000000000000, 0.9238795325112869605, 1.000000000000000000, 0.9238795325112869605, 1.000000000000000000, 0.9238795325112869605, 1.000000000000000000, 0.9238795325112869605, 1.000000000000000000, 0.9238795325112869605, 1.000000000000000000, 0.9238795325112869605, 1.000000000000000000, 0.9238795325112869605, 1.000000000000000000, 0.9238795325112869605, 1.000000000000000000, 0.9238795325112869605, 1.000000000000000000, 0.9238795325112869605, 1.000000000000000000, 0.9238795325112869605, 1.000000000000000000, 0.9238795325112869605, 1.000000000000000000, 0.9238795325112869605, 1.000000000000000000, 0.9238795325112869605, 1.000000000000000000, 0.9238795325112869605, 1.000000000000000000, 0.9238795325112869605, 1.000000000000000000, 0.9238795325112869605, 1.000000000000000000, 0.9238795325112869605, 1.000000000000000000, 0.9238795325112869605, 1.000000000000000000, 0.9238795325112869605, 1.000000000000000000, 0.9238795325112869605, 1.000000000000000000, 0.9238795325112869605, 1.000000000000000000, 0.9238795325112869605, 1.000000000000000000, 0.9238795325112869605, 1.000000000000000000, 0.9238795325112869605, 1.000000000000000000, 0.9238795325112869605, 1.000000000000000000, 0.9238795325112869605, 1.000000000000000000, 0.9238795325112869605, 1.000000000000000000, 0.9238795325112869605, 1.000000000000000000, 0.9238795325112869605, 1.000000000000000000, 0.9238795325112869605, 1.000000000000000000, 0.9238795325112869605, 1.000000000000000000, 0.9238795325112869605, 1.000000000000000000, 0.9238795325112869605, 1.000000000000000000, 0.9238795325112869605, 1.000000000000000000, 0.9238795325112869605, 1.000000000000000000, 0.9238795325112869605, 1.000000000000000000, 0.9238795325112869605, 1.000000000000000000, 0.9238795325112869605, 1.000000000000000000, 0.9238795325112869605, 1.000000000000000000, 0.9238795325112869605, 1.000000000000000000, 0.9238795325112869605, 1.000000000000000000, 0.9238795325112869605, 1.000000000000000000, 0.9238795325112869605, 1.000000000000000000, 0.9238795325112869605, 1.000000000000000000, 0.9238795325112869605, 1.000000000000000000, 0.9238795325112869605, 1.000000000000000000, 0.9238795325112869605, 1.000000000000000000, 0.9238795325112869605, 1.000000000000000000, 0.9238795325112869605, 1.000000000000000000, 0.9238795325112869605, 1.000000000000000000, 0.9238795325112869605, 1.000000000000000000, 0.9238795325112869605, 1.000000000000000000, 0.9238795325112869605, 1.000000000000000000, 0.9238795325112869605, 1.000000000000000000, 0.9238795325112869605, 1.000000000000000000, 0.9238795325112869605, 1.000000000000000000, 0.9238795325112869605, 1.000000000000000000, 0.9238795325112869605, 1.000000000000000000, 0.9238795325112869605, 1.000000000000000000, 0.9238795325112869605, 1.000000000000000000, 0.9238795325112869605, 1.000000000000000000, 0.9238795325112869605, 1.000000000000000000, 0.9238795325112869605, 1.000000000000000000, 0.9238795325112869605, 1.000000000000000000, 0.9238795325112869605, 1.000000000000000000, 0.9238795325112869605, 1.000000000000000000, 0.9238795325112869605, 1.000000000000000000, 0.9238795325112869605, 1.000000000000000000, 0.9238795325112869605, 1.000000000000000000) ) ) 
 REPRESENTATION_ITEM ( '' )  SURFACE ( )  );
#2943 = DIRECTION ( 'NONE',  ( 0.000000000000000000, 0.6004852223388321697, -0.7996358532186279566 ) ) ;
#2944 = CARTESIAN_POINT ( 'NONE',  ( 115.2922348109119781, 0.4262465694468514643, -12.03445270309931736 ) ) ;
#2945 = CARTESIAN_POINT ( 'NONE',  ( 120.2905000025837126, -2.311015703046761072, -18.04188382666269774 ) ) ;
#2946 = CARTESIAN_POINT ( 'NONE',  ( 118.0718414775786442, -0.8288870151387760510, -10.36305467784173118 ) ) ;
#2947 = CIRCLE ( 'NONE', #23364, 5.000000000000004441 ) ;
#2948 = DIRECTION ( 'NONE',  ( 0.000000000000000000, 1.000000000000000000, 0.000000000000000000 ) ) ;
#2949 = CARTESIAN_POINT ( 'NONE',  ( 117.2209414775786485, -2.084020599724406786, -8.691656652584148546 ) ) ;
#2950 = CIRCLE ( 'NONE', #27705, 6.426280380454326924 ) ;
#2951 = CARTESIAN_POINT ( 'NONE',  ( 114.3846081442453197, -10.63000616557722466, -14.87417383870573495 ) ) ;
#2952 = CARTESIAN_POINT ( 'NONE',  ( 123.2855641859119942, -8.321307733199551748, -9.223433127585318303 ) ) ;
#2953 = CARTESIAN_POINT ( 'NONE',  ( 113.4202548109119846, -10.30919188438810075, -12.61870101168855918 ) ) ;
#2954 = CARTESIAN_POINT ( 'NONE',  ( 115.8027748109119841, -8.899110576539710493, -16.42337572283490132 ) ) ;
#2955 = CARTESIAN_POINT ( 'NONE',  ( 113.5337081442453240, -0.8288870151387760510, -10.36305467784173118 ) ) ;
#2956 = CARTESIAN_POINT ( 'NONE',  ( 115.9162281442453235, -5.574606645277164318, -18.38911715685844683 ) ) ;
#2957 = VERTEX_POINT ( 'NONE', #27677 ) ;
#2958 = CARTESIAN_POINT ( 'NONE',  ( 114.0442481442453300, -1.834011780172310813, -8.268836392978581529 ) ) ;
#2959 = CARTESIAN_POINT ( 'NONE',  ( 107.1488171295247867, -10.62599879583958540, -13.39321520033831447 ) ) ;
#2960 = CARTESIAN_POINT ( 'NONE',  ( 106.6626452545248611, -9.868328341294098749, -15.46607636864997204 ) ) ;
#2961 = CARTESIAN_POINT ( 'NONE',  ( 106.8710046295248759, -4.863998795839590272, -18.39754474579285315 ) ) ;
#2962 = DIRECTION ( 'NONE',  ( 1.000000000000000000, 0.000000000000000000, -0.000000000000000000 ) ) ;
#2963 = CARTESIAN_POINT ( 'NONE',  ( 117.2776681442452968, -5.638512984488999180, -18.83840828888717311 ) ) ;
#2964 = VERTEX_POINT ( 'NONE', #34918 ) ;
#2965 = DIRECTION ( 'NONE',  ( 1.000000000000000000, 0.000000000000000000, 0.000000000000000000 ) ) ;
#2966 = CARTESIAN_POINT ( 'NONE',  ( 120.7824894832010472, -2.324775150319219108, -18.02356106541841996 ) ) ;
#2967 = CARTESIAN_POINT ( 'NONE',  ( 118.8660148109119774, 0.1319031606808879209, -14.10382304977623669 ) ) ;
#2968 = CARTESIAN_POINT ( 'NONE',  ( 127.7425183523501744, 0.8652765085452543969, -12.77968882490997338 ) ) ;
#2969 = CARTESIAN_POINT ( 'NONE',  ( 124.1415948109119540, -6.344957434206665248, -7.627207830600338134 ) ) ;
#2970 = CARTESIAN_POINT ( 'NONE',  ( 106.6626452545248611, 0.8980012041604421569, -11.00651665394454071 ) ) ;
#2971 = CARTESIAN_POINT ( 'NONE',  ( 89.28655680551213436, -9.912712791071484730, -13.47323746212486562 ) ) ;
#2972 = ORIENTED_EDGE ( 'NONE', *, *, #25320, .F. ) ;
#2973 = CARTESIAN_POINT ( 'NONE',  ( 112.1155414775786454, 0.9020085738987339008, -11.91225656197089222 ) ) ;
#2974 = CARTESIAN_POINT ( 'NONE',  ( 120.9081748109119872, -4.153390946401325223, -8.397313243818185668 ) ) ;
#2975 = CARTESIAN_POINT ( 'NONE',  ( 120.7379948109119709, -10.63000616557722466, -14.87417383870573495 ) ) ;
#2976 = VECTOR ( 'NONE', #3623, 1000.000000000000000 ) ;
#2977 = CARTESIAN_POINT ( 'NONE',  ( 116.6536748109119941, -10.15424416112533912, -14.75197769757731336 ) ) ;
#2978 = CARTESIAN_POINT ( 'NONE',  ( 119.3198281442452924, 0.5811942927096110934, -14.16772938898807510 ) ) ;
#2979 = DIRECTION ( 'NONE',  ( 0.000000000000000000, 0.000000000000000000, 1.000000000000000000 ) ) ;
#2980 = CYLINDRICAL_SURFACE ( 'NONE', #7519, 1.499999999999996225 ) ;
#2981 = CARTESIAN_POINT ( 'NONE',  ( 124.8223148109119762, -10.15424416112533912, -14.75197769757731336 ) ) ;
#2982 = EDGE_LOOP ( 'NONE', ( #44977, #36661, #11961, #42449 ) ) ;
#2983 = CARTESIAN_POINT ( 'NONE',  ( 116.5945156689966922, -9.863253977036384512, -13.30267646073255250 ) ) ;
#2984 = CIRCLE ( 'NONE', #11775, 3.000000000000003997 ) ;
#2985 = CARTESIAN_POINT ( 'NONE',  ( 118.5256548109119876, -0.4660016031367893996, -10.09054647747474043 ) ) ;
#2986 = CARTESIAN_POINT ( 'NONE',  ( 125.0492214775786266, -3.505236298600246325, -18.68346056562440793 ) ) ;
#2987 = VERTEX_POINT ( 'NONE', #17847 ) ;
#2988 = AXIS2_PLACEMENT_3D ( 'NONE', #4919, #40265, #19061 ) ;
#2989 = CARTESIAN_POINT ( 'NONE',  ( 123.6328298109119714, -7.200787124940443817, -17.81845355600750835 ) ) ;
#2990 = CARTESIAN_POINT ( 'NONE',  ( 61.36049780884140148, -12.47513267055688502, -9.628222199120516578 ) ) ;
#2991 = CARTESIAN_POINT ( 'NONE',  ( 119.6601881442453106, -8.166667518702819706, -8.995218007635861213 ) ) ;
#2992 = CARTESIAN_POINT ( 'NONE',  ( 111.8716296295247901, -4.863998795839590272, -19.15521520033831493 ) ) ;
#2993 = CARTESIAN_POINT ( 'NONE',  ( 118.5256548109119876, -8.899110576539710493, -16.42337572283490132 ) ) ;
#2994 = EDGE_CURVE ( 'NONE', #9021, #11150, #41201, .T. ) ;
#2995 = ORIENTED_EDGE ( 'NONE', *, *, #8638, .T. ) ;
#2996 = EDGE_LOOP ( 'NONE', ( #25071, #25421, #35320, #36704, #2153 ) ) ;
#2997 = CARTESIAN_POINT ( 'NONE',  ( 125.2194014775786286, 0.1319031606808879209, -14.10382304977623669 ) ) ;
#2998 = CARTESIAN_POINT ( 'NONE',  ( 123.6877814775786533, -6.222761293078241884, -8.102969835052219238 ) ) ;
#2999 = DIRECTION ( 'NONE',  ( -0.000000000000000000, -0.9284778069183721172, -0.3713878862591650232 ) ) ;
#3000 = EDGE_CURVE ( 'NONE', #32925, #14305, #16142, .T. ) ;
#3001 = CARTESIAN_POINT ( 'NONE',  ( 70.36267391504962632, -5.685877709920933221, -21.89321520033831447 ) ) ;
#3002 = ADVANCED_FACE ( 'NONE', ( #31747 ), #25144, .T. ) ;
#3003 = CARTESIAN_POINT ( 'NONE',  ( 122.5532481442453019, -10.63000616557722466, -14.87417383870573495 ) ) ;
#3004 = DIRECTION ( 'NONE',  ( 0.000000000000000000, -0.4669533266896290225, -0.8842819633428516957 ) ) ;
#3005 = CIRCLE ( 'NONE', #32124, 2.999999999999999556 ) ;
#3006 = DIRECTION ( 'NONE',  ( -0.000000000000000000, -0.9284778069183718952, -0.3713878862591649677 ) ) ;
#3007 = CARTESIAN_POINT ( 'NONE',  ( 121.1918081442452859, 0.9020085738987339008, -11.91225656197089222 ) ) ;
#3009 = CARTESIAN_POINT ( 'NONE',  ( 120.9081748109119872, -4.153390946401325223, -8.397313243818185668 ) ) ;
#3008 = CARTESIAN_POINT ( 'NONE',  ( 118.5256548109119876, -0.4660016031367893996, -10.09054647747474043 ) ) ;
#3010 = DIRECTION ( 'NONE',  ( -0.9908103287288505534, 0.1352586133457950035, 0.000000000000000000 ) ) ;
#3011 = CARTESIAN_POINT ( 'NONE',  ( 116.2565881442452991, -9.261995988541697145, -16.69588392320189030 ) ) ;
#3012 = ORIENTED_EDGE ( 'NONE', *, *, #20300, .F. ) ;
#3013 = CARTESIAN_POINT ( 'NONE',  ( 124.8790414775786246, -8.899110576539710493, -16.42337572283490132 ) ) ;
#3014 = CARTESIAN_POINT ( 'NONE',  ( 125.0492214775786408, -3.505236298599212041, -18.68346056562414859 ) ) ;
#3015 = CARTESIAN_POINT ( 'NONE',  ( 106.8015515045248378, -2.477300249445798297, -7.631215200338321125 ) ) ;
#3016 = AXIS2_PLACEMENT_3D ( 'NONE', #22812, #36707, #22145 ) ;
#3017 = CARTESIAN_POINT ( 'NONE',  ( 114.0941296295247867, -4.863998795839590272, -8.388885654883775800 ) ) ;
#3018 = CARTESIAN_POINT ( 'NONE',  ( 107.2182702545248105, -10.62599879583958717, -15.77991374673208469 ) ) ;
#3019 = CARTESIAN_POINT ( 'NONE',  ( 120.8514481442452961, -7.893985811506177619, -18.51759400769804742 ) ) ;
#3020 = CARTESIAN_POINT ( 'NONE',  ( 123.2906948109119867, -1.833838273342659697, -17.42832698103878286 ) ) ;
#3021 = ORIENTED_EDGE ( 'NONE', *, *, #35385, .T. ) ;
#3022 = EDGE_CURVE ( 'NONE', #42672, #1762, #4029, .T. ) ;
#3023 = CARTESIAN_POINT ( 'NONE',  ( 122.9503348109119827, 0.5811942927096110934, -14.16772938898807510 ) ) ;
#3024 = CARTESIAN_POINT ( 'NONE',  ( 112.6828081442453282, -2.084020599724406786, -8.691656652584148546 ) ) ;
#3025 = DIRECTION ( 'NONE',  ( 1.000000000000000000, 0.000000000000000000, 0.000000000000000000 ) ) ;
#3026 = CARTESIAN_POINT ( 'NONE',  ( 123.3474214775786209, -9.988377603198976828, -10.36322818467138340 ) ) ;
#3027 = ADVANCED_FACE ( 'NONE', ( #8257 ), #28066, .T. ) ;
#3028 = EDGE_CURVE ( 'NONE', #20614, #29197, #33873, .T. ) ;
#3029 = CARTESIAN_POINT ( 'NONE',  ( 120.3976348109119812, -1.834011780172310813, -8.268836392978581529 ) ) ;
#3030 = CARTESIAN_POINT ( 'NONE',  ( 120.0180923109119675, -9.285408612553503360, -11.05844856689016886 ) ) ;
#3031 = CARTESIAN_POINT ( 'NONE',  ( 126.6942948109119840, -8.899110576539710493, -16.42337572283490132 ) ) ;
#3032 = CARTESIAN_POINT ( 'NONE',  ( 111.9254164575755226, -1.016270020561755860, -17.26805140881366896 ) ) ;
#3033 = CARTESIAN_POINT ( 'NONE',  ( 107.4266296295248821, -4.863998795839590272, -19.15521520033831493 ) ) ;
#3034 = ORIENTED_EDGE ( 'NONE', *, *, #26998, .T. ) ;
#3035 = CARTESIAN_POINT ( 'NONE',  ( 70.19189222814998175, -57.25954915413987578, -36.10662921840084749 ) ) ;
#3036 = CARTESIAN_POINT ( 'NONE',  ( 113.3635281442453504, -0.1624402480850797581, -16.17319339645315424 ) ) ;
#3037 = CARTESIAN_POINT ( 'NONE',  ( 123.5176014775786228, -0.8288870151387760510, -10.36305467784173118 ) ) ;
#3038 = CARTESIAN_POINT ( 'NONE',  ( 109.7880358795247986, -8.402594152722688392, -9.854619843455216355 ) ) ;
#3039 = CARTESIAN_POINT ( 'NONE',  ( 107.9128015045248219, -6.936859964151250502, -18.39754474579286025 ) ) ;
#3040 = CARTESIAN_POINT ( 'NONE',  ( 121.4754414775786131, -1.833838273342659697, -17.42832698103878286 ) ) ;
#3041 = CARTESIAN_POINT ( 'NONE',  ( 116.8238548109119819, -5.574606645277164318, -18.38911715685844683 ) ) ;
#3042 = CARTESIAN_POINT ( 'NONE',  ( 111.8319081442453182, -4.153390946401321671, -8.397313243818183892 ) ) ;
#3043 = ORIENTED_EDGE ( 'NONE', *, *, #16129, .T. ) ;
#3044 = CARTESIAN_POINT ( 'NONE',  ( 123.9146881442452894, -10.15424416112533912, -14.75197769757731336 ) ) ;
#3045 = CARTESIAN_POINT ( 'NONE',  ( 119.2063748109119814, -1.561330072975668504, -17.79121239304076951 ) ) ;
#3046 = CIRCLE ( 'NONE', #31438, 26.50000000000000000 ) ;
#3047 = DIRECTION ( 'NONE',  ( 0.000000000000000000, 0.000000000000000000, -1.000000000000000000 ) ) ;
#3048 = ORIENTED_EDGE ( 'NONE', *, *, #22274, .F. ) ;
#3049 = DIRECTION ( 'NONE',  ( -1.000000000000000000, 0.000000000000000000, 0.000000000000000000 ) ) ;
#3050 = ORIENTED_EDGE ( 'NONE', *, *, #25617, .T. ) ;
#3051 = CARTESIAN_POINT ( 'NONE',  ( 115.6893214775786447, -9.859900752359374465, -12.68260735090039404 ) ) ;
#3052 = CARTESIAN_POINT ( 'NONE',  ( 112.6260814775786514, -0.8288870151387760510, -10.36305467784173118 ) ) ;
#3053 = DIRECTION ( 'NONE',  ( 0.000000000000000000, -0.3818493186865936084, 0.9242245927363024194 ) ) ;
#3054 = CARTESIAN_POINT ( 'NONE',  ( 123.6328298109119714, -7.200787124940443817, -17.81845355600750835 ) ) ;
#3055 = VERTEX_POINT ( 'NONE', #962 ) ;
#3056 = CARTESIAN_POINT ( 'NONE',  ( 70.19189222814998175, -61.33395589173652951, -37.73637771078367109 ) ) ;
#3057 = CARTESIAN_POINT ( 'NONE',  ( 124.7472578386062452, 2.844596103920410179, -12.34114520301823781 ) ) ;
#3058 = EDGE_CURVE ( 'NONE', #13698, #24351, #14650, .T. ) ;
#3059 = CARTESIAN_POINT ( 'NONE',  ( 115.2053796295247849, -4.863998795839590272, -19.15521520033831493 ) ) ;
#3060 = CARTESIAN_POINT ( 'NONE',  ( 83.83554121260367253, -26.75858941326842810, -11.54476601486570964 ) ) ;
#3061 = CARTESIAN_POINT ( 'NONE',  ( 124.3117748109119844, 0.1319031606808879209, -14.10382304977623669 ) ) ;
#3062 = EDGE_CURVE ( 'NONE', #38783, #36515, #18522, .T. ) ;
#3063 = CARTESIAN_POINT ( 'NONE',  ( 112.6260814775786514, -0.8288870151387760510, -10.36305467784173118 ) ) ;
#3064 = CARTESIAN_POINT ( 'NONE',  ( 126.4082675373902873, -6.091288680381572007, -18.33809601120119481 ) ) ;
#3065 = EDGE_LOOP ( 'NONE', ( #38219, #3508, #17725 ) ) ;
#3066 = CARTESIAN_POINT ( 'NONE',  ( 116.1082702545247827, 0.1403307496149616695, -11.32035403202665336 ) ) ;
#3067 = CARTESIAN_POINT ( 'NONE',  ( 116.4114176093651878, 0.5600166689815611054, -14.64321520033831447 ) ) ;
#3068 = CARTESIAN_POINT ( 'NONE',  ( 112.3578015045248719, -2.477300249445798297, -7.631215200338321125 ) ) ;
#3069 = CARTESIAN_POINT ( 'NONE',  ( 128.2184548109119930, 0.6402711692277476274, -15.78131322003126868 ) ) ;
#3071 = DIRECTION ( 'NONE',  ( 1.000000000000000000, 0.000000000000000000, -0.000000000000000000 ) ) ;
#3070 = CARTESIAN_POINT ( 'NONE',  ( 66.38809756183205479, -36.79083284667497367, -4.893215200338314474 ) ) ;
#3072 = CARTESIAN_POINT ( 'NONE',  ( 111.9453614775786434, -1.561330072975668060, -17.79121239304076596 ) ) ;
#3073 = EDGE_LOOP ( 'NONE', ( #19466, #6837, #32313, #23665 ) ) ;
#3074 = CARTESIAN_POINT ( 'NONE',  ( 115.0086014775786509, -4.089484607189486809, -7.948022111789456723 ) ) ;
#3075 = CARTESIAN_POINT ( 'NONE',  ( 122.0046199480702569, -6.365377317481695663, -18.95617363400926081 ) ) ;
#3076 = CARTESIAN_POINT ( 'NONE',  ( 115.4831921295247952, 0.8980012041604618078, -13.39321520033831447 ) ) ;
#3077 = EDGE_CURVE ( 'NONE', #39008, #5980, #30316, .T. ) ;
#3078 = CARTESIAN_POINT ( 'NONE',  ( 125.0492214775786266, -3.505236298600246325, -18.68346056562440793 ) ) ;
#3079 = CARTESIAN_POINT ( 'NONE',  ( 124.7655881442452852, -9.859900752359378018, -12.68260735090039759 ) ) ;
#3080 = CYLINDRICAL_SURFACE ( 'NONE', #38052, 3.000000000000001776 ) ;
#3081 = CARTESIAN_POINT ( 'NONE',  ( 115.7610046295247912, -4.863998795839590272, -18.39754474579285315 ) ) ;
#3082 = CARTESIAN_POINT ( 'NONE',  ( 70.19189222814998175, -57.62004466406304459, -36.25082616574700722 ) ) ;
#3083 = CARTESIAN_POINT ( 'NONE',  ( 77.25325688895158294, -4.012910213732562070, -18.79321520033831661 ) ) ;
#3084 = CARTESIAN_POINT ( 'NONE',  ( 112.5126281442453120, 0.1319031606808879209, -14.10382304977623669 ) ) ;
#3085 = CARTESIAN_POINT ( 'NONE',  ( 107.8433483795247838, -0.7896495226426338832, -9.318865927141430916 ) ) ;
#3086 = DIRECTION ( 'NONE',  ( 0.000000000000000000, 0.6004852223388321697, -0.7996358532186279566 ) ) ;
#3087 = CARTESIAN_POINT ( 'NONE',  ( 112.8439733795247832, -8.938348069036489818, -17.46756447353520159 ) ) ;
#3088 = CARTESIAN_POINT ( 'NONE',  ( 125.2194014775786286, -10.30919188438810075, -12.61870101168855918 ) ) ;
#3089 = CARTESIAN_POINT ( 'NONE',  ( 111.8319081442453182, -4.153390946401321671, -8.397313243818183892 ) ) ;
#3090 = DIRECTION ( 'NONE',  ( 0.000000000000000000, 0.000000000000000000, 1.000000000000000000 ) ) ;
#3091 = EDGE_CURVE ( 'NONE', #10499, #36439, #12770, .T. ) ;
#3092 = CARTESIAN_POINT ( 'NONE',  ( 119.2063748109119814, -1.561330072975668504, -17.79121239304076951 ) ) ;
#3093 = CARTESIAN_POINT ( 'NONE',  ( 113.5904348109119866, -7.893985811506177619, -18.51759400769804742 ) ) ;
#3094 = ORIENTED_EDGE ( 'NONE', *, *, #6249, .F. ) ;
#3095 = CARTESIAN_POINT ( 'NONE',  ( 112.7962614775786676, -6.222761293078241884, -8.102969835052219238 ) ) ;
#3096 = CARTESIAN_POINT ( 'NONE',  ( 125.6164881442453094, 0.2603800115204892296, -16.42320221600525088 ) ) ;
#3097 = CARTESIAN_POINT ( 'NONE',  ( 124.9357681442453014, -1.834011780172310813, -8.268836392978581529 ) ) ;
#3098 = CARTESIAN_POINT ( 'NONE',  ( 115.4056881442453459, -7.893985811506177619, -18.51759400769804742 ) ) ;
#3099 = CARTESIAN_POINT ( 'NONE',  ( 113.8173414775786512, -9.565557343593413364, -10.61323700422348004 ) ) ;
#3100 = ORIENTED_EDGE ( 'NONE', *, *, #43789, .T. ) ;
#3101 = CARTESIAN_POINT ( 'NONE',  ( 116.7671281442453335, -7.643976991954077427, -18.09477374809248928 ) ) ;
#3102 = CONICAL_SURFACE ( 'NONE', #33670, 1.610000000000000986, 0.9599310885968765916 ) ;
#3103 = CARTESIAN_POINT ( 'NONE',  ( 112.3424481442453384, -6.344957434206662583, -7.627207830600332805 ) ) ;
#3104 = AXIS2_PLACEMENT_3D ( 'NONE', #28209, #4242, #14515 ) ;
#3105 = CARTESIAN_POINT ( 'NONE',  ( 123.7445081442452874, -7.894159318335828068, -9.358103419637847864 ) ) ;
#3106 = CARTESIAN_POINT ( 'NONE',  ( 116.8417075039013184, -0.9679852802911167453, -16.90817056666675811 ) ) ;
#3107 = CARTESIAN_POINT ( 'NONE',  ( 114.3719421295247827, 0.8980012041604618078, -13.39321520033831447 ) ) ;
#3108 = ORIENTED_EDGE ( 'NONE', *, *, #8673, .T. ) ;
#3109 = PRODUCT_DEFINITION_FORMATION_WITH_SPECIFIED_SOURCE ( 'ANY', '', #10664, .NOT_KNOWN. ) ;
#3110 = CARTESIAN_POINT ( 'NONE',  ( 67.28387040543748299, -1.679813135375296529, -9.537078095872010053 ) ) ;
#3111 = CARTESIAN_POINT ( 'NONE',  ( 113.0776676093651929, 0.5600166689815611054, -14.64321520033833579 ) ) ;
#3112 = CARTESIAN_POINT ( 'NONE',  ( 117.0111608795247946, -1.325403438956436419, -16.93181055722141792 ) ) ;
#3113 = AXIS2_PLACEMENT_3D ( 'NONE', #37307, #23420, #36848 ) ;
#3114 = FILL_AREA_STYLE ('',( #44179 ) ) ;
#3115 = CARTESIAN_POINT ( 'NONE',  ( 122.6604860609119640, -6.564341423271553566, -7.887810678476492754 ) ) ;
#3116 = CARTESIAN_POINT ( 'NONE',  ( 112.6828081442453282, -2.084020599724406786, -8.691656652584148546 ) ) ;
#3117 = CARTESIAN_POINT ( 'NONE',  ( 107.9128015045248219, -6.936859964151250502, -18.39754474579286025 ) ) ;
#3118 = EDGE_CURVE ( 'NONE', #31077, #16022, #33141, .T. ) ;
#3119 = CARTESIAN_POINT ( 'NONE',  ( 111.5023434012278898, 0.04929351793716424401, -14.64321520033831447 ) ) ;
#3120 = MECHANICAL_DESIGN_GEOMETRIC_PRESENTATION_REPRESENTATION (  '', ( #32202 ), #1166 ) ;
#3121 = CARTESIAN_POINT ( 'NONE',  ( 120.0005481442453146, -5.638512984488999180, -18.83840828888717311 ) ) ;
#3122 = CARTESIAN_POINT ( 'NONE',  ( 137.2844488807198502, -4.793161434092606754, -18.62470134987731640 ) ) ;
#3123 = DIRECTION ( 'NONE',  ( 0.9609149988134843001, -0.1028163501681632064, 0.2570431154366505933 ) ) ;
#3124 = CARTESIAN_POINT ( 'NONE',  ( 124.3968141859119925, -8.321307733199789780, -9.223433127585511926 ) ) ;
#3125 = CARTESIAN_POINT ( 'NONE',  ( 120.3976348109119812, -7.643976991954077427, -18.09477374809248928 ) ) ;
#3126 = VERTEX_POINT ( 'NONE', #18070 ) ;
#3127 = CARTESIAN_POINT ( 'NONE',  ( 135.9690293846493319, -9.531372520637221513, -9.741219538532039479 ) ) ;
#3128 = CARTESIAN_POINT ( 'NONE',  ( 118.9794681442453026, -9.261995988541697145, -16.69588392320189030 ) ) ;
#3129 = DIRECTION ( 'NONE',  ( -0.000000000000000000, -0.9284778069183720062, -0.3713878862591650232 ) ) ;
#3130 = CARTESIAN_POINT ( 'NONE',  ( 117.0507614775786465, 0.1319031606808879209, -14.10382304977623669 ) ) ;
#3131 =( BOUNDED_SURFACE ( )  B_SPLINE_SURFACE ( 1, 2, ( 
 ( #17394, #34902, #947, #31282, #17832, #31949, #31729, #10553, #55, #35591, #28774, #3913, #14411, #499, #18058, #31505, #42682, #28553, #714, #277, #13969, #25356, #10997, #21922, #27881, #14187, #42233, #3691, #21477, #21253, #14635, #24898, #38791, #39250, #21029, #28106, #7563, #35132, #35362, #14865, #41795, #4137, #7795, #38342, #42458, #11223, #8015, #10775, #25129, #7119, #17613, #39024, #21704, #24671, #4361, #7334, #18281, #38558, #4587, #32400, #43124, #29890, #11893, #29435, #22150, #25575, #23049, #25795, #8243, #5263, #5036, #12120, #15530, #36493, #29214, #1171, #15986, #43350, #8917, #26022, #43575, #39704, #28997, #12345, #18950, #9143, #11667, #39479, #18510, #15086, #36042, #33287, #42905, #32841, #19179, #1609, #4811, #18732, #22818, #43806, #36268, #39928, #8688, #33058, #15306, #12573, #1391, #32625, #22593, #8469, #22372, #26243, #40155, #1831, #15761, #29662, #26477, #36710, #5479, #19400, #2062, #40382, #33507, #20312, #33745, #20535, #12797, #34415, #13475, #9367, #2515, #9596, #30563, #37631, #5706, #2287, #31009, #10275, #6622, #17120, #16441, #34196, #23963, #2970, #10060, #3196, #44482, #44939, #27377, #2743, #26920, #41300, #37848, #23276, #30342, #13249, #16667, #27151, #44265, #27604, #16216 ),
 ( #16898, #23512, #41073, #44034, #9830, #23740, #30120, #13696, #6404, #41518, #30791, #44715, #36935, #19623, #13022, #26698, #40609, #37158, #5934, #37399, #19857, #40841, #6169, #20089, #33975, #14807, #3853, #20757, #28495, #3422, #17998, #25070, #31669, #38286, #32119, #14130, #28720, #34636, #14355, #41733, #17553, #7065, #24398, #20976, #31896, #21417, #10497, #42401, #662, #887, #10937, #38962, #4073, #31229, #34849, #24619, #3635, #6850, #28268, #42626, #24180, #17776, #28046, #38072, #13910, #31447, #41954, #10719, #14578, #27821, #11165, #38502, #35302, #1, #24840, #7279, #7731, #38731, #35531, #217, #21195, #35072, #21642, #438, #4303, #42177, #17339, #7502, #18225, #36217, #18458, #33238, #8640, #22540, #19124, #39874, #1557, #5433, #43525, #1782, #43070, #15937, #33007, #32570, #29609, #7957, #15480, #28942, #4757, #25521, #11610, #39424, #5205, #36437, #42851, #12293, #15707, #19351, #43298, #26193, #40100, #32348, #8189, #11838, #22098, #39191, #29385, #29836, #11388, #4982, #1336, #2012, #1114, #35986, #15251, #29157, #8859, #15031, #22761, #25746, #36660, #18678, #12067, #39652, #25299, #25969, #21868, #8415, #22320, #18894, #35763, #32786, #4534, #12975, #2918, #26419, #43755, #26870, #36884, #44664, #16619 ) ),
 .UNSPECIFIED., .F., .F., .F. ) 
 B_SPLINE_SURFACE_WITH_KNOTS ( ( 2, 2 ),
 ( 3, 2, 2, 2, 2, 2, 2, 2, 2, 2, 2, 2, 2, 2, 2, 2, 2, 2, 2, 2, 2, 2, 2, 2, 2, 2, 2, 2, 2, 2, 2, 2, 2, 2, 2, 2, 2, 2, 2, 2, 2, 2, 2, 2, 2, 2, 2, 2, 2, 2, 2, 2, 2, 2, 2, 2, 2, 2, 2, 2, 2, 2, 2, 2, 2, 2, 2, 2, 2, 2, 2, 2, 2, 2, 2, 2, 2, 2, 2, 2, 3 ),
 ( 0.000000000000000000, 1.000000000000000000 ),
 ( 0.000000000000000000, 0.01250000000000000069, 0.02500000000000000139, 0.03749999999999999861, 0.05000000000000000278, 0.06250000000000000000, 0.07499999999999999722, 0.08749999999999999445, 0.1000000000000000056, 0.1125000000000000028, 0.1250000000000000000, 0.1375000000000000111, 0.1499999999999999944, 0.1625000000000000056, 0.1749999999999999889, 0.1875000000000000000, 0.2000000000000000111, 0.2124999999999999944, 0.2250000000000000056, 0.2374999999999999889, 0.2500000000000000000, 0.2625000000000000111, 0.2750000000000000222, 0.2874999999999999778, 0.2999999999999999889, 0.3125000000000000000, 0.3250000000000000111, 0.3375000000000000222, 0.3499999999999999778, 0.3624999999999999889, 0.3750000000000000000, 0.3875000000000000111, 0.4000000000000000222, 0.4124999999999999778, 0.4249999999999999889, 0.4375000000000000000, 0.4500000000000000111, 0.4625000000000000222, 0.4749999999999999778, 0.4874999999999999889, 0.5000000000000000000, 0.5124999999999999556, 0.5250000000000000222, 0.5374999999999999778, 0.5500000000000000444, 0.5625000000000000000, 0.5749999999999999556, 0.5875000000000000222, 0.5999999999999999778, 0.6125000000000000444, 0.6250000000000000000, 0.6374999999999999556, 0.6500000000000000222, 0.6624999999999999778, 0.6750000000000000444, 0.6875000000000000000, 0.6999999999999999556, 0.7125000000000000222, 0.7249999999999999778, 0.7375000000000000444, 0.7500000000000000000, 0.7624999999999999556, 0.7750000000000000222, 0.7874999999999999778, 0.8000000000000000444, 0.8125000000000000000, 0.8249999999999999556, 0.8375000000000000222, 0.8499999999999999778, 0.8625000000000000444, 0.8750000000000000000, 0.8874999999999999556, 0.9000000000000000222, 0.9124999999999999778, 0.9250000000000000444, 0.9375000000000000000, 0.9499999999999999556, 0.9625000000000000222, 0.9749999999999999778, 0.9875000000000000444, 1.000000000000000000 ),
 .UNSPECIFIED. ) 
 GEOMETRIC_REPRESENTATION_ITEM ( )  RATIONAL_B_SPLINE_SURFACE ( (
 ( 1.000000000000000000, 0.9238795325112869605, 1.000000000000000000, 0.9238795325112869605, 1.000000000000000000, 0.9238795325112869605, 1.000000000000000000, 0.9238795325112869605, 1.000000000000000000, 0.9238795325112869605, 1.000000000000000000, 0.9238795325112869605, 1.000000000000000000, 0.9238795325112869605, 1.000000000000000000, 0.9238795325112869605, 1.000000000000000000, 0.9238795325112869605, 1.000000000000000000, 0.9238795325112869605, 1.000000000000000000, 0.9238795325112869605, 1.000000000000000000, 0.9238795325112869605, 1.000000000000000000, 0.9238795325112869605, 1.000000000000000000, 0.9238795325112869605, 1.000000000000000000, 0.9238795325112869605, 1.000000000000000000, 0.9238795325112869605, 1.000000000000000000, 0.9238795325112869605, 1.000000000000000000, 0.9238795325112869605, 1.000000000000000000, 0.9238795325112869605, 1.000000000000000000, 0.9238795325112869605, 1.000000000000000000, 0.9238795325112869605, 1.000000000000000000, 0.9238795325112869605, 1.000000000000000000, 0.9238795325112869605, 1.000000000000000000, 0.9238795325112869605, 1.000000000000000000, 0.9238795325112869605, 1.000000000000000000, 0.9238795325112869605, 1.000000000000000000, 0.9238795325112869605, 1.000000000000000000, 0.9238795325112869605, 1.000000000000000000, 0.9238795325112869605, 1.000000000000000000, 0.9238795325112869605, 1.000000000000000000, 0.9238795325112869605, 1.000000000000000000, 0.9238795325112869605, 1.000000000000000000, 0.9238795325112869605, 1.000000000000000000, 0.9238795325112869605, 1.000000000000000000, 0.9238795325112869605, 1.000000000000000000, 0.9238795325112869605, 1.000000000000000000, 0.9238795325112869605, 1.000000000000000000, 0.9238795325112869605, 1.000000000000000000, 0.9238795325112869605, 1.000000000000000000, 0.9238795325112869605, 1.000000000000000000, 0.9238795325112869605, 1.000000000000000000, 0.9238795325112869605, 1.000000000000000000, 0.9238795325112869605, 1.000000000000000000, 0.9238795325112869605, 1.000000000000000000, 0.9238795325112869605, 1.000000000000000000, 0.9238795325112869605, 1.000000000000000000, 0.9238795325112869605, 1.000000000000000000, 0.9238795325112869605, 1.000000000000000000, 0.9238795325112869605, 1.000000000000000000, 0.9238795325112869605, 1.000000000000000000, 0.9238795325112869605, 1.000000000000000000, 0.9238795325112869605, 1.000000000000000000, 0.9238795325112869605, 1.000000000000000000, 0.9238795325112869605, 1.000000000000000000, 0.9238795325112869605, 1.000000000000000000, 0.9238795325112869605, 1.000000000000000000, 0.9238795325112869605, 1.000000000000000000, 0.9238795325112869605, 1.000000000000000000, 0.9238795325112869605, 1.000000000000000000, 0.9238795325112869605, 1.000000000000000000, 0.9238795325112869605, 1.000000000000000000, 0.9238795325112869605, 1.000000000000000000, 0.9238795325112869605, 1.000000000000000000, 0.9238795325112869605, 1.000000000000000000, 0.9238795325112869605, 1.000000000000000000, 0.9238795325112869605, 1.000000000000000000, 0.9238795325112869605, 1.000000000000000000, 0.9238795325112869605, 1.000000000000000000, 0.9238795325112869605, 1.000000000000000000, 0.9238795325112869605, 1.000000000000000000, 0.9238795325112869605, 1.000000000000000000, 0.9238795325112869605, 1.000000000000000000, 0.9238795325112869605, 1.000000000000000000, 0.9238795325112869605, 1.000000000000000000, 0.9238795325112869605, 1.000000000000000000, 0.9238795325112869605, 1.000000000000000000, 0.9238795325112869605, 1.000000000000000000, 0.9238795325112869605, 1.000000000000000000, 0.9238795325112869605, 1.000000000000000000, 0.9238795325112869605, 1.000000000000000000),
 ( 1.000000000000000000, 0.9238795325112869605, 1.000000000000000000, 0.9238795325112869605, 1.000000000000000000, 0.9238795325112869605, 1.000000000000000000, 0.9238795325112869605, 1.000000000000000000, 0.9238795325112869605, 1.000000000000000000, 0.9238795325112869605, 1.000000000000000000, 0.9238795325112869605, 1.000000000000000000, 0.9238795325112869605, 1.000000000000000000, 0.9238795325112869605, 1.000000000000000000, 0.9238795325112869605, 1.000000000000000000, 0.9238795325112869605, 1.000000000000000000, 0.9238795325112869605, 1.000000000000000000, 0.9238795325112869605, 1.000000000000000000, 0.9238795325112869605, 1.000000000000000000, 0.9238795325112869605, 1.000000000000000000, 0.9238795325112869605, 1.000000000000000000, 0.9238795325112869605, 1.000000000000000000, 0.9238795325112869605, 1.000000000000000000, 0.9238795325112869605, 1.000000000000000000, 0.9238795325112869605, 1.000000000000000000, 0.9238795325112869605, 1.000000000000000000, 0.9238795325112869605, 1.000000000000000000, 0.9238795325112869605, 1.000000000000000000, 0.9238795325112869605, 1.000000000000000000, 0.9238795325112869605, 1.000000000000000000, 0.9238795325112869605, 1.000000000000000000, 0.9238795325112869605, 1.000000000000000000, 0.9238795325112869605, 1.000000000000000000, 0.9238795325112869605, 1.000000000000000000, 0.9238795325112869605, 1.000000000000000000, 0.9238795325112869605, 1.000000000000000000, 0.9238795325112869605, 1.000000000000000000, 0.9238795325112869605, 1.000000000000000000, 0.9238795325112869605, 1.000000000000000000, 0.9238795325112869605, 1.000000000000000000, 0.9238795325112869605, 1.000000000000000000, 0.9238795325112869605, 1.000000000000000000, 0.9238795325112869605, 1.000000000000000000, 0.9238795325112869605, 1.000000000000000000, 0.9238795325112869605, 1.000000000000000000, 0.9238795325112869605, 1.000000000000000000, 0.9238795325112869605, 1.000000000000000000, 0.9238795325112869605, 1.000000000000000000, 0.9238795325112869605, 1.000000000000000000, 0.9238795325112869605, 1.000000000000000000, 0.9238795325112869605, 1.000000000000000000, 0.9238795325112869605, 1.000000000000000000, 0.9238795325112869605, 1.000000000000000000, 0.9238795325112869605, 1.000000000000000000, 0.9238795325112869605, 1.000000000000000000, 0.9238795325112869605, 1.000000000000000000, 0.9238795325112869605, 1.000000000000000000, 0.9238795325112869605, 1.000000000000000000, 0.9238795325112869605, 1.000000000000000000, 0.9238795325112869605, 1.000000000000000000, 0.9238795325112869605, 1.000000000000000000, 0.9238795325112869605, 1.000000000000000000, 0.9238795325112869605, 1.000000000000000000, 0.9238795325112869605, 1.000000000000000000, 0.9238795325112869605, 1.000000000000000000, 0.9238795325112869605, 1.000000000000000000, 0.9238795325112869605, 1.000000000000000000, 0.9238795325112869605, 1.000000000000000000, 0.9238795325112869605, 1.000000000000000000, 0.9238795325112869605, 1.000000000000000000, 0.9238795325112869605, 1.000000000000000000, 0.9238795325112869605, 1.000000000000000000, 0.9238795325112869605, 1.000000000000000000, 0.9238795325112869605, 1.000000000000000000, 0.9238795325112869605, 1.000000000000000000, 0.9238795325112869605, 1.000000000000000000, 0.9238795325112869605, 1.000000000000000000, 0.9238795325112869605, 1.000000000000000000, 0.9238795325112869605, 1.000000000000000000, 0.9238795325112869605, 1.000000000000000000, 0.9238795325112869605, 1.000000000000000000, 0.9238795325112869605, 1.000000000000000000, 0.9238795325112869605, 1.000000000000000000, 0.9238795325112869605, 1.000000000000000000, 0.9238795325112869605, 1.000000000000000000) ) ) 
 REPRESENTATION_ITEM ( '' )  SURFACE ( )  );
#3133 = CARTESIAN_POINT ( 'NONE',  ( 113.8740681442453138, -9.859900752359374465, -12.68260735090039404 ) ) ;
#3132 = CONICAL_SURFACE ( 'NONE', #14782, 5.000000000000000888, 0.7853981633974419507 ) ;
#3134 = CARTESIAN_POINT ( 'NONE',  ( 112.2188952545247531, 0.8980012041604421569, -11.00651665394454071 ) ) ;
#3135 = CARTESIAN_POINT ( 'NONE',  ( 123.9584548109119737, -9.675291321254654520, -19.78473021908636298 ) ) ;
#3136 = CARTESIAN_POINT ( 'NONE',  ( 82.85213572415328542, -31.80476018815861394, -23.17883450557113179 ) ) ;
#3137 = CARTESIAN_POINT ( 'NONE',  ( 118.2420214775786320, -6.222761293078241884, -8.102969835052219238 ) ) ;
#3138 = AXIS2_PLACEMENT_3D ( 'NONE', #23330, #40897, #13907 ) ;
#3139 = CARTESIAN_POINT ( 'NONE',  ( 120.0005481442453146, -4.153390946401325223, -8.397313243818185668 ) ) ;
#3140 = EDGE_CURVE ( 'NONE', #31689, #36176, #21490, .T. ) ;
#3141 = CARTESIAN_POINT ( 'NONE',  ( 123.8411891859119862, -1.406689858478935573, -17.56299727309130887 ) ) ;
#3142 = CARTESIAN_POINT ( 'NONE',  ( 121.6881423109119709, -9.959231468620755479, -10.70263013195267199 ) ) ;
#3143 = CARTESIAN_POINT ( 'NONE',  ( 109.3018640045248304, 0.1403307496149616695, -15.46607636864997204 ) ) ;
#3144 = ORIENTED_EDGE ( 'NONE', *, *, #616, .F. ) ;
#3145 = DIRECTION ( 'NONE',  ( 0.000000000000000000, -0.9242245927363041957, -0.3818493186865896671 ) ) ;
#3146 = CARTESIAN_POINT ( 'NONE',  ( 112.8529881442453302, -1.561330072975668060, -17.79121239304076596 ) ) ;
#3147 = CARTESIAN_POINT ( 'NONE',  ( 112.1155414775786454, 0.9020085738987339008, -11.91225656197089222 ) ) ;
#3148 = CARTESIAN_POINT ( 'NONE',  ( 124.1916298109119765, -2.529232162390850913, -8.971805383624186447 ) ) ;
#3149 = CARTESIAN_POINT ( 'NONE',  ( 119.6045485609119794, -0.08252387247370887580, -11.91645802438286417 ) ) ;
#3150 = ORIENTED_EDGE ( 'NONE', *, *, #39135, .F. ) ;
#3151 = CARTESIAN_POINT ( 'NONE',  ( 123.3995567976525365, -2.659420626585511371, -15.07970544296840210 ) ) ;
#3152 = ORIENTED_EDGE ( 'NONE', *, *, #22778, .F. ) ;
#3153 = CIRCLE ( 'NONE', #30069, 2.999999999999999556 ) ;
#3154 = CARTESIAN_POINT ( 'NONE',  ( 120.2841814775786276, 0.9020085738987339008, -11.91225656197089222 ) ) ;
#3155 = CARTESIAN_POINT ( 'NONE',  ( 126.3539348109119800, -4.153390946401325223, -8.397313243818185668 ) ) ;
#3156 = CARTESIAN_POINT ( 'NONE',  ( 117.7882081442453170, -3.505236298600246325, -18.68346056562440793 ) ) ;
#3157 = CARTESIAN_POINT ( 'NONE',  ( 84.86020291624612355, -29.99489077589588959, -18.39321520033831803 ) ) ;
#3158 = CARTESIAN_POINT ( 'NONE',  ( 121.4754414775786131, -8.166667518702819706, -8.995218007635861213 ) ) ;
#3159 = CARTESIAN_POINT ( 'NONE',  ( 118.7525614775786380, -8.166667518702819706, -8.995218007635861213 ) ) ;
#3160 = CARTESIAN_POINT ( 'NONE',  ( 108.2600671295247992, 0.1403307496149613920, -13.39321520033831447 ) ) ;
#3161 = CARTESIAN_POINT ( 'NONE',  ( 111.2646414775786496, -8.899110576539710493, -16.42337572283490132 ) ) ;
#3162 = DIRECTION ( 'NONE',  ( 1.000000000000000000, 0.000000000000000000, 0.000000000000000000 ) ) ;
#3163 = ORIENTED_EDGE ( 'NONE', *, *, #17306, .F. ) ;
#3164 = CARTESIAN_POINT ( 'NONE',  ( 119.0361948109119652, -7.893985811506177619, -18.51759400769804742 ) ) ;
#3165 = MECHANICAL_DESIGN_GEOMETRIC_PRESENTATION_REPRESENTATION (  '', ( #37398 ), #22108 ) ;
#3166 = CARTESIAN_POINT ( 'NONE',  ( 121.4103298109119748, -2.173413727453600508, -8.297982527556802879 ) ) ;
#3167 = CARTESIAN_POINT ( 'NONE',  ( 114.1009748109119784, -4.089484607189486809, -7.948022111789456723 ) ) ;
#3168 = ORIENTED_EDGE ( 'NONE', *, *, #11769, .T. ) ;
#3169 = AXIS2_PLACEMENT_3D ( 'NONE', #18891, #42847, #28716 ) ;
#3170 = CARTESIAN_POINT ( 'NONE',  ( 125.1059481442452750, -8.166667518702819706, -8.995218007635861213 ) ) ;
#3171 = CARTESIAN_POINT ( 'NONE',  ( 91.11246428952674137, -25.99489077589524300, -13.39321520033831625 ) ) ;
#3172 = CARTESIAN_POINT ( 'NONE',  ( 113.5904348109119866, -2.084020599724406786, -8.691656652584148546 ) ) ;
#3173 = FACE_OUTER_BOUND ( 'NONE', #539, .T. ) ;
#3174 = CARTESIAN_POINT ( 'NONE',  ( 116.4834948109119779, -7.894159318335828068, -9.358103419637847864 ) ) ;
#3175 = CARTESIAN_POINT ( 'NONE',  ( 91.38554522942851577, -25.38011337280982715, -14.88121679464376257 ) ) ;
#3176 = CARTESIAN_POINT ( 'NONE',  ( 119.4900081442453086, -7.643976991954077427, -18.09477374809248928 ) ) ;
#3177 = CARTESIAN_POINT ( 'NONE',  ( 64.01282776924008999, -34.86145050234443943, -5.893215200338315363 ) ) ;
#3178 = CARTESIAN_POINT ( 'NONE',  ( 117.5045748109119756, -9.859900752359374465, -12.68260735090039404 ) ) ;
#3179 = CARTESIAN_POINT ( 'NONE',  ( 124.1190016859119680, -9.665098340737509730, -17.37397104707595474 ) ) ;
#3180 = CARTESIAN_POINT ( 'NONE',  ( 116.1998614775786507, -10.63000616557722466, -14.87417383870573495 ) ) ;
#3181 = CARTESIAN_POINT ( 'NONE',  ( 113.6471614775786492, -4.153390946401321671, -8.397313243818183892 ) ) ;
#3182 = CARTESIAN_POINT ( 'NONE',  ( 116.7104014775786425, -8.899110576539710493, -16.42337572283490132 ) ) ;
#3183 = VERTEX_POINT ( 'NONE', #42918 ) ;
#3184 = CARTESIAN_POINT ( 'NONE',  ( 117.2776681442452968, -5.638512984488999180, -18.83840828888717311 ) ) ;
#3185 = CARTESIAN_POINT ( 'NONE',  ( 108.5378796295247810, -4.863998795839590272, -19.15521520033831493 ) ) ;
#3186 = CARTESIAN_POINT ( 'NONE',  ( 107.0793640045248196, 0.1403307496149616695, -15.46607636864997204 ) ) ;
#3187 = CARTESIAN_POINT ( 'NONE',  ( 106.1070202545248407, 0.1403307496149616695, -11.32035403202665336 ) ) ;
#3188 = EDGE_CURVE ( 'NONE', #5920, #30137, #13528, .T. ) ;
#3189 = CARTESIAN_POINT ( 'NONE',  ( 123.0862602976252020, -8.580000213326620440, -17.71054824844518905 ) ) ;
#3190 = CARTESIAN_POINT ( 'NONE',  ( 123.5743281442453139, -7.893985811506177619, -18.51759400769804742 ) ) ;
#3191 = VERTEX_POINT ( 'NONE', #22162 ) ;
#3192 = DIRECTION ( 'NONE',  ( 0.000000000000000000, 0.6004852223388321697, -0.7996358532186279566 ) ) ;
#3193 = CARTESIAN_POINT ( 'NONE',  ( 119.0929214775786278, -4.153390946401325223, -8.397313243818185668 ) ) ;
#3194 = DIRECTION ( 'NONE',  ( 0.000000000000000000, 0.000000000000000000, 1.000000000000000000 ) ) ;
#3195 = CARTESIAN_POINT ( 'NONE',  ( 123.2339681442453241, -6.344957434206665248, -7.627207830600338134 ) ) ;
#3196 = CARTESIAN_POINT ( 'NONE',  ( 106.5237390045248418, 0.8980012041604421569, -15.77991374673208469 ) ) ;
#3197 = DIRECTION ( 'NONE',  ( 0.000000000000000000, 0.6004852223388323917, -0.7996358532186279566 ) ) ;
#3198 = ORIENTED_EDGE ( 'NONE', *, *, #522, .F. ) ;
#3199 = CYLINDRICAL_SURFACE ( 'NONE', #16531, 1.587500000000000577 ) ;
#3200 = CARTESIAN_POINT ( 'NONE',  ( 125.7299414775786346, -10.15424416112533912, -14.75197769757731336 ) ) ;
#3201 = CARTESIAN_POINT ( 'NONE',  ( 122.8936081442453059, 0.2603800115204892296, -16.42320221600525088 ) ) ;
#3202 = CARTESIAN_POINT ( 'NONE',  ( 117.4478481442453131, -9.565557343593413364, -10.61323700422348004 ) ) ;
#3203 = CARTESIAN_POINT ( 'NONE',  ( 74.69189222814998175, -41.76310523276723785, -19.39321520033831447 ) ) ;
#3204 = CARTESIAN_POINT ( 'NONE',  ( 120.4543614775786295, -4.089484607189486809, -7.948022111789456723 ) ) ;
#3205 = CARTESIAN_POINT ( 'NONE',  ( 70.19189222814998175, -50.76020450571126474, -33.50691401458669105 ) ) ;
#3206 = CARTESIAN_POINT ( 'NONE',  ( 125.6732148109119862, -9.859900752359378018, -12.68260735090039759 ) ) ;
#3207 = CARTESIAN_POINT ( 'NONE',  ( 121.3052614775786111, -7.643976991954077427, -18.09477374809248928 ) ) ;
#3208 = EDGE_LOOP ( 'NONE', ( #28421, #11225, #13823, #21479 ) ) ;
#3209 = DIRECTION ( 'NONE',  ( 0.9609149988134837450, -0.1028163501681639419, 0.2570431154366518145 ) ) ;
#3210 = CARTESIAN_POINT ( 'NONE',  ( 117.6747548109119919, -1.834011780172310813, -8.268836392978581529 ) ) ;
#3211 = CARTESIAN_POINT ( 'NONE',  ( 124.7088614775786226, -9.565557343593413364, -10.61323700422348004 ) ) ;
#3212 = ORIENTED_EDGE ( 'NONE', *, *, #14450, .T. ) ;
#3213 = CARTESIAN_POINT ( 'NONE',  ( 123.7022829359119811, -4.283928203966213211, -7.183505701512925334 ) ) ;
#3214 = CARTESIAN_POINT ( 'NONE',  ( 135.8419766445667278, -1.204973725236484716, -8.697158258016544963 ) ) ;
#3215 = CARTESIAN_POINT ( 'NONE',  ( 121.0216281442452981, -1.561330072975668948, -17.79121239304076951 ) ) ;
#3216 = CARTESIAN_POINT ( 'NONE',  ( 108.8156921295247912, 0.8980012041604618078, -13.39321520033831447 ) ) ;
#3217 = CARTESIAN_POINT ( 'NONE',  ( 119.4332814775786318, -8.899110576539710493, -16.42337572283490132 ) ) ;
#3218 = EDGE_LOOP ( 'NONE', ( #13058, #19724, #35343, #35662, #45141 ) ) ;
#3219 = ORIENTED_EDGE ( 'NONE', *, *, #4676, .F. ) ;
#3220 = CARTESIAN_POINT ( 'NONE',  ( 115.6893214775786447, 0.5811942927096154232, -14.16772938898807155 ) ) ;
#3221 = CARTESIAN_POINT ( 'NONE',  ( 123.9714148109119805, -8.899110576539710493, -16.42337572283490132 ) ) ;
#3222 = DIRECTION ( 'NONE',  ( 0.000000000000000000, 0.000000000000000000, 1.000000000000000000 ) ) ;
#3223 = CARTESIAN_POINT ( 'NONE',  ( 69.69189222814998175, -41.76310523276723785, -4.893215200338314474 ) ) ;
#3224 = AXIS2_PLACEMENT_3D ( 'NONE', #32148, #15503, #4559 ) ;
#3225 = CARTESIAN_POINT ( 'NONE',  ( 122.6667014775786413, -7.893985811506177619, -18.51759400769804742 ) ) ;
#3226 = DIRECTION ( 'NONE',  ( 0.000000000000000000, -0.4669533266896266355, -0.8842819633428529169 ) ) ;
#3227 = B_SPLINE_CURVE_WITH_KNOTS ( 'NONE', 3,
 ( #27995, #28664, #21362, #24568, #387, #22038, #35245, #41900, #7224, #42568, #32293, #14973, #39370, #11330, #4700, #1058, #11559, #25466, #10885, #4022, #42349, #8137, #21138, #35014, #3794, #17944, #17720, #612, #31618, #14300, #25010, #40035, #22931, #19517, #19739 ),
 .UNSPECIFIED., .F., .F.,
 ( 4, 2, 2, 1, 1, 2, 2, 2, 2, 1, 1, 2, 2, 2, 2, 1, 1, 1, 2, 2, 4 ),
 ( 0.000000000000000000, 0.1250000000001383060, 0.1875000000002075840, 0.2187500000002391698, 0.2343750000002570721, 0.2421875000002660372, 0.2500000000002749467, 0.3750000000004191647, 0.4375000000004898859, 0.4687500000005253020, 0.4843750000005431211, 0.4921875000005542233, 0.5000000000005653256, 0.6250000000006362688, 0.6875000000006702416, 0.7187500000006900036, 0.7343750000006985523, 0.7421875000007027712, 0.7460937500007075451, 0.7500000000007122081, 1.000000000000000000 ),
 .UNSPECIFIED. ) ;
#3228 = CARTESIAN_POINT ( 'NONE',  ( 67.30914723170953096, -57.87957791055376333, -37.24914645096997390 ) ) ;
#3229 = CARTESIAN_POINT ( 'NONE',  ( 118.5823814775786360, -1.834011780172310813, -8.268836392978581529 ) ) ;
#3231 = CARTESIAN_POINT ( 'NONE',  ( 119.0929214775786278, -4.153390946401325223, -8.397313243818185668 ) ) ;
#3230 = CARTESIAN_POINT ( 'NONE',  ( 119.4332814775786318, -0.4660016031367893996, -10.09054647747474043 ) ) ;
#3232 = CARTESIAN_POINT ( 'NONE',  ( 66.58723489636778936, -20.14619392353143112, -19.39321520033831447 ) ) ;
#3233 = CARTESIAN_POINT ( 'NONE',  ( 116.9373081442452929, -8.166667518702817929, -8.995218007635861213 ) ) ;
#3234 = ORIENTED_EDGE ( 'NONE', *, *, #35618, .T. ) ;
#3235 = CARTESIAN_POINT ( 'NONE',  ( 112.2289948109119848, -1.834011780172310813, -8.268836392978581529 ) ) ;
#3236 = CARTESIAN_POINT ( 'NONE',  ( 125.7761281442453196, -10.10582367741896093, -14.73954123521881066 ) ) ;
#3237 = CARTESIAN_POINT ( 'NONE',  ( 109.2324108795247923, -8.938348069036489818, -9.318865927141430916 ) ) ;
#3238 = CARTESIAN_POINT ( 'NONE',  ( 107.0099108795247815, -1.325403438956436419, -16.93181055722141792 ) ) ;
#3239 = CARTESIAN_POINT ( 'NONE',  ( 108.3989733795248753, -8.938348069036489818, -17.46756447353520159 ) ) ;
#3240 = CARTESIAN_POINT ( 'NONE',  ( 122.7801548109119665, -3.383040157471821630, -19.15922257007629170 ) ) ;
#3241 = CARTESIAN_POINT ( 'NONE',  ( 122.2696148109119889, -5.574606645277164318, -18.38911715685844683 ) ) ;
#3242 = ORIENTED_EDGE ( 'NONE', *, *, #6941, .F. ) ;
#3243 = CARTESIAN_POINT ( 'NONE',  ( 124.7655881442452852, 0.5811942927096110934, -14.16772938898807510 ) ) ;
#3244 = CARTESIAN_POINT ( 'NONE',  ( 112.2188952545247531, 0.8980012041604421569, -11.00651665394454071 ) ) ;
#3245 = CARTESIAN_POINT ( 'NONE',  ( 117.2294421295247844, -10.76310523276723785, -5.182735500338556456 ) ) ;
#3246 = CARTESIAN_POINT ( 'NONE',  ( 123.5176014775786228, -9.261995988541697145, -16.69588392320189030 ) ) ;
#3247 = CARTESIAN_POINT ( 'NONE',  ( 61.69189222814998175, -49.76310523276723785, -19.39321520033831447 ) ) ;
#3248 = CARTESIAN_POINT ( 'NONE',  ( 70.19189222814998175, -61.90193818873174791, -37.96356864969668266 ) ) ;
#3249 = CARTESIAN_POINT ( 'NONE',  ( 114.1009748109119784, -4.089484607189486809, -7.948022111789456723 ) ) ;
#3250 = CARTESIAN_POINT ( 'NONE',  ( 67.84197459855160162, -61.08251850740028033, -38.36497664958400122 ) ) ;
#3251 = CARTESIAN_POINT ( 'NONE',  ( 107.2182702545248105, -10.62599879583958717, -15.77991374673208469 ) ) ;
#3252 = CIRCLE ( 'NONE', #16373, 2.000000000000000444 ) ;
#3253 = ORIENTED_EDGE ( 'NONE', *, *, #13645, .F. ) ;
#3254 = CARTESIAN_POINT ( 'NONE',  ( 77.44400397045842510, -3.459648945705700473, -14.39321520033831625 ) ) ;
#3255 = CARTESIAN_POINT ( 'NONE',  ( 113.3068014775786594, -1.833838273342658809, -17.42832698103878286 ) ) ;
#3256 = CARTESIAN_POINT ( 'NONE',  ( 112.5126281442453120, -10.30919188438810075, -12.61870101168855918 ) ) ;
#3257 = CARTESIAN_POINT ( 'NONE',  ( 107.0793640045248196, 0.1403307496149616695, -15.46607636864997204 ) ) ;
#3258 = CARTESIAN_POINT ( 'NONE',  ( 105.2735827545248810, -6.936859964151250502, -8.388885654883777576 ) ) ;
#3259 = CARTESIAN_POINT ( 'NONE',  ( 121.7590748109119687, -2.084020599724406786, -8.691656652584148546 ) ) ;
#3260 = CARTESIAN_POINT ( 'NONE',  ( 115.0086014775786509, -5.574606645277164318, -18.38911715685844683 ) ) ;
#3261 = CARTESIAN_POINT ( 'NONE',  ( 113.7606148109119886, -7.894159318335828068, -9.358103419637847864 ) ) ;
#3262 = ORIENTED_EDGE ( 'NONE', *, *, #18240, .T. ) ;
#3263 = CARTESIAN_POINT ( 'NONE',  ( 124.3685014775786328, 0.4262465694468514643, -12.03445270309931736 ) ) ;
#3264 = CARTESIAN_POINT ( 'NONE',  ( 117.7882081442453170, -6.344957434206665248, -7.627207830600338134 ) ) ;
#3265 = LINE ( 'NONE', #6918, #11338 ) ;
#3266 = CARTESIAN_POINT ( 'NONE',  ( 114.8384214775786489, -10.15424416112533912, -14.75197769757731336 ) ) ;
#3267 = ORIENTED_EDGE ( 'NONE', *, *, #28125, .T. ) ;
#3268 = FACE_OUTER_BOUND ( 'NONE', #20576, .T. ) ;
#3269 = ORIENTED_EDGE ( 'NONE', *, *, #25124, .T. ) ;
#3270 = CARTESIAN_POINT ( 'NONE',  ( 116.7104014775786425, -8.899110576539710493, -16.42337572283490132 ) ) ;
#3271 = CARTESIAN_POINT ( 'NONE',  ( 115.1787814775786387, -0.1624402480850797581, -16.17319339645315424 ) ) ;
#3272 = EDGE_CURVE ( 'NONE', #34550, #30411, #21035, .T. ) ;
#3273 = DIRECTION ( 'NONE',  ( 0.000000000000000000, 0.000000000000000000, 1.000000000000000000 ) ) ;
#3274 = EDGE_CURVE ( 'NONE', #22330, #24697, #37528, .T. ) ;
#3275 = EDGE_CURVE ( 'NONE', #32855, #40329, #32189, .T. ) ;
#3276 = CARTESIAN_POINT ( 'NONE',  ( 121.3408766859119794, -9.033780868592240054, -16.85052413769862056 ) ) ;
#3277 = EDGE_LOOP ( 'NONE', ( #17579, #9420, #5051, #7378, #14820 ) ) ;
#3278 = CARTESIAN_POINT ( 'NONE',  ( 70.19189222814998175, -54.47411573338475677, -34.99246555962335492 ) ) ;
#3279 = CARTESIAN_POINT ( 'NONE',  ( 63.09505974864278244, -3.280483143683338820, -7.685112946281191348 ) ) ;
#3280 = VECTOR ( 'NONE', #28746, 1000.000000000000000 ) ;
#3281 = CARTESIAN_POINT ( 'NONE',  ( 107.1488171295247867, 0.1403307496149613920, -13.39321520033831447 ) ) ;
#3282 = CARTESIAN_POINT ( 'NONE',  ( 115.2748327545248657, -6.936859964151250502, -8.388885654883788234 ) ) ;
#3283 = CARTESIAN_POINT ( 'NONE',  ( 122.8368814775786291, -7.894159318335828068, -9.358103419637847864 ) ) ;
#3284 = CARTESIAN_POINT ( 'NONE',  ( 113.8173414775786512, -9.565557343593413364, -10.61323700422348004 ) ) ;
#3285 = CARTESIAN_POINT ( 'NONE',  ( 113.5904348109119866, -2.084020599724388578, -8.691656652584157428 ) ) ;
#3286 = ORIENTED_EDGE ( 'NONE', *, *, #42664, .F. ) ;
#3287 = LINE ( 'NONE', #6943, #24417 ) ;
#3288 = VECTOR ( 'NONE', #34511, 999.9999999999998863 ) ;
#3289 = CARTESIAN_POINT ( 'NONE',  ( 116.3700414775786527, -4.153390946401321671, -8.397313243818183892 ) ) ;
#3290 = CARTESIAN_POINT ( 'NONE',  ( 122.5977428165343781, -2.324775150319219108, -18.02356106541841996 ) ) ;
#3291 = CARTESIAN_POINT ( 'NONE',  ( -3.049772195457630897, -7.199189612102626867, -19.39321520033830737 ) ) ;
#3293 = CARTESIAN_POINT ( 'NONE',  ( 116.8797485810857069, -1.220279397241700758, -16.99638242193885063 ) ) ;
#3292 = CARTESIAN_POINT ( 'NONE',  ( 65.66749702063913219, -36.20550398600038022, -5.467054258871666406 ) ) ;
#3294 = CARTESIAN_POINT ( 'NONE',  ( 125.3895814775786448, -2.084020599724406786, -8.691656652584148546 ) ) ;
#3295 = ORIENTED_EDGE ( 'NONE', *, *, #22804, .F. ) ;
#3296 = CARTESIAN_POINT ( 'NONE',  ( 114.4413348109119823, -9.261995988541697145, -16.69588392320189030 ) ) ;
#3297 = CARTESIAN_POINT ( 'NONE',  ( 124.6894688159050872, -8.253847584685239269, -17.09290432062678278 ) ) ;
#3298 = CARTESIAN_POINT ( 'NONE',  ( 106.5931921295248372, -9.868328341294093420, -13.39321520033831447 ) ) ;
#3299 = CARTESIAN_POINT ( 'NONE',  ( 124.9357681442453014, -7.643976991954077427, -18.09477374809248928 ) ) ;
#3300 = CARTESIAN_POINT ( 'NONE',  ( 124.8790414775786246, -8.899110576539710493, -16.42337572283490132 ) ) ;
#3301 = CARTESIAN_POINT ( 'NONE',  ( 96.46827370896536991, -25.85028767034691199, -12.39451169347363546 ) ) ;
#3302 = CARTESIAN_POINT ( 'NONE',  ( 108.7462390045248242, -9.868328341294098749, -11.32035403202665869 ) ) ;
#3303 = ADVANCED_FACE ( 'NONE', ( #26260 ), #26708, .T. ) ;
#3304 = CARTESIAN_POINT ( 'NONE',  ( 111.8716296295247901, -4.863998795839590272, -19.15521520033831493 ) ) ;
#3305 = CARTESIAN_POINT ( 'NONE',  ( 119.8129079359119942, -4.360204210389833968, -8.000047426360245240 ) ) ;
#3306 = CARTESIAN_POINT ( 'NONE',  ( 114.4980614775786734, -2.084020599724406786, -8.691656652584148546 ) ) ;
#3307 = CARTESIAN_POINT ( 'NONE',  ( 107.7738952545248310, 0.8980012041604421569, -11.00651665394454071 ) ) ;
#3308 = CARTESIAN_POINT ( 'NONE',  ( 123.7184548109119788, -3.484218720211407661, -13.98160872758045770 ) ) ;
#3309 = CARTESIAN_POINT ( 'NONE',  ( 109.9963952545248134, 0.8980012041604421569, -11.00651665394454071 ) ) ;
#3310 = CARTESIAN_POINT ( 'NONE',  ( 123.5176014775786228, -9.261995988541697145, -16.69588392320189030 ) ) ;
#3311 = CARTESIAN_POINT ( 'NONE',  ( 112.1155414775786454, -10.15424416112533912, -14.75197769757731336 ) ) ;
#3312 = CARTESIAN_POINT ( 'NONE',  ( 111.7308551332721862, 0.2334052082820642360, -14.64321520033831447 ) ) ;
#3313 = EDGE_CURVE ( 'NONE', #6780, #34510, #28571, .T. ) ;
#3314 = CARTESIAN_POINT ( 'NONE',  ( 121.6456214775786293, -10.63000616557722466, -14.87417383870573495 ) ) ;
#3315 = CARTESIAN_POINT ( 'NONE',  ( 115.5758681442453053, -1.561330072975668060, -17.79121239304076951 ) ) ;
#3316 = EDGE_LOOP ( 'NONE', ( #20362, #18445, #22955, #37207, #34104 ) ) ;
#3317 = EDGE_CURVE ( 'NONE', #37700, #3191, #21724, .T. ) ;
#3318 = VECTOR ( 'NONE', #5118, 999.9999999999998863 ) ;
#3319 = CARTESIAN_POINT ( 'NONE',  ( 115.1220548109119761, -1.833838273342658809, -17.42832698103878286 ) ) ;
#3320 = CARTESIAN_POINT ( 'NONE',  ( 122.1561614775786353, -0.4660016031367893996, -10.09054647747474043 ) ) ;
#3321 = CARTESIAN_POINT ( 'NONE',  ( 114.4413348109119823, -9.261995988541697145, -16.69588392320189030 ) ) ;
#3322 = B_SPLINE_CURVE_WITH_KNOTS ( 'NONE', 3,
 ( #9850, #41320, #20332, #27841, #3214, #31247, #23982, #3440, #20992, #34866, #37868, #27398, #16688, #13265, #20775, #33994, #14149, #27622, #30581, #41536, #10297, #19, #44734, #13932, #41754, #3654, #40861, #17575, #31467, #9614, #23533, #37419, #6188, #41092, #20108, #2763, #6424, #34217, #14374, #10957, #679, #38983, #42196, #39445, #11411, #25538, #36004, #21217, #459, #35551, #35092, #31690, #3875, #41974, #11186, #11626 ),
 .UNSPECIFIED., .F., .F.,
 ( 4, 2, 2, 2, 2, 2, 2, 1, 2, 2, 2, 2, 2, 2, 2, 2, 2, 2, 2, 2, 2, 1, 2, 2, 2, 2, 2, 2, 4 ),
 ( 0.000000000000000000, 0.06250000000001902645, 0.09375000000003509693, 0.1093750000000366374, 0.1250000000000381917, 0.1875000000000199285, 0.2187500000000047462, 0.2343749999999969469, 0.2421874999999932554, 0.2499999999999895917, 0.3125000000000103251, 0.3437500000000163203, 0.3593750000000197065, 0.3750000000000230371, 0.5000000000000551781, 0.5625000000000714984, 0.5937500000000812683, 0.6093750000000863754, 0.6250000000000914824, 0.6875000000001173506, 0.7187500000001303402, 0.7343750000001322276, 0.7421875000001330047, 0.7500000000001337819, 0.8125000000000972555, 0.8437500000000790479, 0.8593750000000698330, 0.8750000000000607292, 1.000000000000000000 ),
 .UNSPECIFIED. ) ;
#3323 = CARTESIAN_POINT ( 'NONE',  ( 117.1642148109119859, -0.8288870151387760510, -10.36305467784173118 ) ) ;
#3324 = ORIENTED_EDGE ( 'NONE', *, *, #35176, .T. ) ;
#3325 = CARTESIAN_POINT ( 'NONE',  ( 117.1074881442453233, 0.4262465694468514643, -12.03445270309931736 ) ) ;
#3326 = AXIS2_PLACEMENT_3D ( 'NONE', #41163, #30884, #27248 ) ;
#3327 = CARTESIAN_POINT ( 'NONE',  ( 117.1642148109119859, -9.261995988541697145, -16.69588392320189030 ) ) ;
#3328 = CARTESIAN_POINT ( 'NONE',  ( 123.1205148109119563, -7.643976991954077427, -18.09477374809248928 ) ) ;
#3329 = FACE_OUTER_BOUND ( 'NONE', #11678, .T. ) ;
#3330 = B_SPLINE_CURVE_WITH_KNOTS ( 'NONE', 3,
 ( #18846, #19072, #30009, #39377, #8364, #12016, #43020, #29559, #29336, #26141 ),
 .UNSPECIFIED., .F., .F.,
 ( 4, 3, 3, 4 ),
 ( 0.000000000000000000, 0.0002476487219222790075, 0.0004952974148303519383, 0.0009534114850261680291 ),
 .UNSPECIFIED. ) ;
#3331 = CARTESIAN_POINT ( 'NONE',  ( 113.3301452545248083, 0.8980012041604421569, -11.00651665394454071 ) ) ;
#3332 = ORIENTED_EDGE ( 'NONE', *, *, #1737, .F. ) ;
#3333 = EDGE_CURVE ( 'NONE', #40981, #11839, #5747, .T. ) ;
#3334 = ADVANCED_FACE ( 'NONE', ( #25376 ), #6329, .T. ) ;
#3335 = EDGE_CURVE ( 'NONE', #40778, #1801, #44847, .T. ) ;
#3336 = PLANE ( 'NONE',  #14796 ) ;
#3337 = CARTESIAN_POINT ( 'NONE',  ( 113.2226630180080775, 0.7607806665038616689, -14.64321520033831447 ) ) ;
#3338 = PLANE ( 'NONE',  #32780 ) ;
#3339 = CARTESIAN_POINT ( 'NONE',  ( 115.6325948109119821, 0.2603800115204892296, -16.42320221600525088 ) ) ;
#3340 = CARTESIAN_POINT ( 'NONE',  ( 70.47992290675011873, 2.032776587329049978, -10.39321520033831625 ) ) ;
#3341 = CARTESIAN_POINT ( 'NONE',  ( 113.2500748109119968, -3.505236298600246325, -18.68346056562440793 ) ) ;
#3342 = CARTESIAN_POINT ( 'NONE',  ( 61.06105367438289733, -12.49321934622164321, -17.22529996229299343 ) ) ;
#3343 = CARTESIAN_POINT ( 'NONE',  ( 123.1938586403692000, -1.196538596002817867, -17.02799684832028504 ) ) ;
#3344 = CARTESIAN_POINT ( 'NONE',  ( 114.7192077545248594, -2.791137627527939813, -18.39754474579286025 ) ) ;
#3345 = CARTESIAN_POINT ( 'NONE',  ( 118.2987481442453088, -1.561330072975668504, -17.79121239304076951 ) ) ;
#3346 = CARTESIAN_POINT ( 'NONE',  ( 137.1428665321213884, -6.586308144700341316, -18.46356886511411943 ) ) ;
#3347 = VECTOR ( 'NONE', #35792, 1000.000000000000114 ) ;
#3348 = DIRECTION ( 'NONE',  ( 0.000000000000000000, 0.000000000000000000, 1.000000000000000000 ) ) ;
#3349 = CARTESIAN_POINT ( 'NONE',  ( 70.19189222814998175, -42.69543048370626792, -27.04993751765913501 ) ) ;
#3350 = CARTESIAN_POINT ( 'NONE',  ( 121.7023481442452777, -0.8288870151387760510, -10.36305467784173118 ) ) ;
#3351 = ORIENTED_EDGE ( 'NONE', *, *, #7188, .F. ) ;
#3352 = DIRECTION ( 'NONE',  ( -0.9609149988134838560, 0.1028163501681644970, -0.2570431154366519810 ) ) ;
#3353 = CARTESIAN_POINT ( 'NONE',  ( 118.4689281442453392, 0.9020085738987339008, -11.91225656197089222 ) ) ;
#3354 = CARTESIAN_POINT ( 'NONE',  ( 121.9272896737536911, -8.611453504372539314, -17.77011218421760574 ) ) ;
#3355 = CARTESIAN_POINT ( 'NONE',  ( 116.5402214775786405, -9.565557343593413364, -10.61323700422348004 ) ) ;
#3356 = AXIS2_PLACEMENT_3D ( 'NONE', #28804, #39055, #34931 ) ;
#3357 = CARTESIAN_POINT ( 'NONE',  ( 112.9664414775786412, -9.859900752359374465, -12.68260735090039404 ) ) ;
#3358 = CARTESIAN_POINT ( 'NONE',  ( 111.0381921295247878, 0.8980012041604618078, -13.39321520033831447 ) ) ;
#3359 = CARTESIAN_POINT ( 'NONE',  ( 105.8292077545248446, -2.791137627527939813, -18.39754474579286025 ) ) ;
#3360 = CARTESIAN_POINT ( 'NONE',  ( 114.0246765045248196, -7.250697342233347165, -19.15521520033831138 ) ) ;
#3361 = CARTESIAN_POINT ( 'NONE',  ( 116.7104014775786425, -8.899110576539710493, -16.42337572283490132 ) ) ;
#3362 = CARTESIAN_POINT ( 'NONE',  ( 118.8660148109119774, 0.1319031606808879209, -14.10382304977623669 ) ) ;
#3363 = CARTESIAN_POINT ( 'NONE',  ( 123.7263390224331516, -4.681800857092183854, -18.57451437749315559 ) ) ;
#3364 = CARTESIAN_POINT ( 'NONE',  ( 120.5074391859119913, -8.844754642576884152, -8.592115655440050404 ) ) ;
#3365 = CARTESIAN_POINT ( 'NONE',  ( 108.8156921295247912, -9.868328341294093420, -13.39321520033831447 ) ) ;
#3366 = PRODUCT ( 'Barrel Adjuster Screw', 'Barrel Adjuster Screw', '', ( #38914 ) ) ;
#3367 = DIRECTION ( 'NONE',  ( 0.9609149988134837450, -0.1028163501681639419, 0.2570431154366518145 ) ) ;
#3368 = CARTESIAN_POINT ( 'NONE',  ( 115.6893214775786447, 0.5811942927096154232, -14.16772938898807155 ) ) ;
#3369 = CARTESIAN_POINT ( 'NONE',  ( 113.5337081442453240, -9.261995988541697145, -16.69588392320189030 ) ) ;
#3370 = DIRECTION ( 'NONE',  ( -0.000000000000000000, -0.000000000000000000, 1.000000000000000000 ) ) ;
#3371 = ORIENTED_EDGE ( 'NONE', *, *, #3945, .F. ) ;
#3372 = CARTESIAN_POINT ( 'NONE',  ( 113.3995983795247895, -0.7896495226426338832, -9.318865927141425587 ) ) ;
#3373 = ORIENTED_EDGE ( 'NONE', *, *, #39824, .F. ) ;
#3374 = CARTESIAN_POINT ( 'NONE',  ( 123.1772414775786189, -4.089484607189486809, -7.948022111789456723 ) ) ;
#3375 = CARTESIAN_POINT ( 'NONE',  ( 126.1837548109119496, 0.4262465694468514643, -12.03445270309931736 ) ) ;
#3376 = CARTESIAN_POINT ( 'NONE',  ( 116.8238548109119819, -5.574606645277164318, -18.38911715685844683 ) ) ;
#3377 = TOROIDAL_SURFACE ( 'NONE', #6271, 7.132259260909269649, 2.000000000000000000 ) ;
#3378 =( NAMED_UNIT ( * ) SI_UNIT ( $, .STERADIAN. ) SOLID_ANGLE_UNIT ( ) );
#3379 = CYLINDRICAL_SURFACE ( 'NONE', #39557, 5.999999999999997335 ) ;
#3380 = CARTESIAN_POINT ( 'NONE',  ( 120.6812681442452941, -10.30919188438810075, -12.61870101168855918 ) ) ;
#3381 = CARTESIAN_POINT ( 'NONE',  ( 119.0361948109119652, -7.893985811506177619, -18.51759400769804742 ) ) ;
#3382 = EDGE_CURVE ( 'NONE', #44507, #41378, #20454, .T. ) ;
#3383 = CARTESIAN_POINT ( 'NONE',  ( 107.2877233795247776, -1.325403438956436419, -9.854619843455211026 ) ) ;
#3384 = CARTESIAN_POINT ( 'NONE',  ( 114.0442481442453300, -7.643976991954077427, -18.09477374809248928 ) ) ;
#3385 = CARTESIAN_POINT ( 'NONE',  ( 89.78938736644981589, -24.14644159042263993, -12.62951656296512937 ) ) ;
#3386 = VERTEX_POINT ( 'NONE', #34336 ) ;
#3387 = CARTESIAN_POINT ( 'NONE',  ( 118.2987481442453088, -1.561330072975668504, -17.79121239304076951 ) ) ;
#3388 = AXIS2_PLACEMENT_3D ( 'NONE', #28349, #7591, #31979 ) ;
#3389 = DIRECTION ( 'NONE',  ( 0.000000000000000000, 0.000000000000000000, 1.000000000000000000 ) ) ;
#3390 = CARTESIAN_POINT ( 'NONE',  ( 114.4413348109119823, -9.261995988541697145, -16.69588392320189030 ) ) ;
#3391 = ORIENTED_EDGE ( 'NONE', *, *, #4145, .F. ) ;
#3392 = CARTESIAN_POINT ( 'NONE',  ( 115.2748327545248657, -2.477300249445798297, -19.15521520033831138 ) ) ;
#3393 = CARTESIAN_POINT ( 'NONE',  ( -13.78505786849335379, -3.796669023459796843, -8.893215200338350002 ) ) ;
#3394 = DIRECTION ( 'NONE',  ( -0.000000000000000000, -0.9284778069183718952, -0.3713878862591649677 ) ) ;
#3395 = CARTESIAN_POINT ( 'NONE',  ( 112.6260814775786514, -0.8288870151387760510, -10.36305467784173118 ) ) ;
#3396 = CARTESIAN_POINT ( 'NONE',  ( 125.4584548109119737, -7.411001340234434132, -5.146477690568067587 ) ) ;
#3397 = EDGE_CURVE ( 'NONE', #20803, #8943, #29560, .T. ) ;
#3398 =( BOUNDED_CURVE ( )  B_SPLINE_CURVE ( 2, ( #23731, #5697, #37622, #16433, #27143, #23038, #2734, #5926, #20303, #30553, #27369, #36925, #40600 ),
 .UNSPECIFIED., .F., .F. ) 
 B_SPLINE_CURVE_WITH_KNOTS ( ( 3, 2, 2, 2, 2, 2, 3 ),
 ( 0.6035091206787219775, 0.6125000000000000444, 0.6250000000000000000, 0.6374999999999999556, 0.6500000000000000222, 0.6624999999999999778, 0.6627876305315190120 ),
 .UNSPECIFIED. ) 
 CURVE ( )  GEOMETRIC_REPRESENTATION_ITEM ( )  RATIONAL_B_SPLINE_CURVE ( ( 0.9692594319298230010, 0.9452488050343769155, 1.000000000000000000, 0.9238795325112869605, 1.000000000000000000, 0.9238795325112869605, 1.000000000000000000, 0.9238795325112869605, 1.000000000000000000, 0.9238795325112869605, 1.000000000000000000, 0.9982484343581399244, 0.9965774773173300405 ) ) 
 REPRESENTATION_ITEM ( '' )  );
#3399 = CARTESIAN_POINT ( 'NONE',  ( 117.5045748109119756, -9.859900752359374465, -12.68260735090039404 ) ) ;
#3400 = DIRECTION ( 'NONE',  ( 0.9609149988134837450, -0.1028163501681639419, 0.2570431154366518145 ) ) ;
#3401 = CARTESIAN_POINT ( 'NONE',  ( 118.6391081442452986, -5.574606645277164318, -18.38911715685844683 ) ) ;
#3402 = DIRECTION ( 'NONE',  ( 0.000000000000000000, 0.000000000000000000, -1.000000000000000000 ) ) ;
#3403 = CONICAL_SURFACE ( 'NONE', #35405, 2.000000000000000444, 0.9599310885968830309 ) ;
#3404 = CARTESIAN_POINT ( 'NONE',  ( 120.5678148109119832, -1.833838273342659253, -17.42832698103878286 ) ) ;
#3405 = CARTESIAN_POINT ( 'NONE',  ( 122.1743141859119817, -0.8832429491016019485, -18.19431474523657855 ) ) ;
#3406 = CARTESIAN_POINT ( 'NONE',  ( 117.2209414775786485, -7.893985811506177619, -18.51759400769804742 ) ) ;
#3407 = CARTESIAN_POINT ( 'NONE',  ( 117.7882081442453170, -3.505236298600246325, -18.68346056562440793 ) ) ;
#3408 = ORIENTED_EDGE ( 'NONE', *, *, #4467, .T. ) ;
#3409 = CARTESIAN_POINT ( 'NONE',  ( 116.3700414775786527, -5.638512984488999180, -18.83840828888717311 ) ) ;
#3410 = CARTESIAN_POINT ( 'NONE',  ( 107.6349890045248401, 0.8980012041604421569, -15.77991374673208469 ) ) ;
#3411 = VECTOR ( 'NONE', #44028, 1000.000000000000000 ) ;
#3412 = CARTESIAN_POINT ( 'NONE',  ( 106.5931921295248372, -9.868328341294093420, -13.39321520033831447 ) ) ;
#3413 = CARTESIAN_POINT ( 'NONE',  ( 105.7597546295248350, -4.863998795839590272, -18.39754474579285315 ) ) ;
#3414 = CARTESIAN_POINT ( 'NONE',  ( 123.1339422641554506, -8.548534124195541040, -17.65096007659765220 ) ) ;
#3415 = CARTESIAN_POINT ( 'NONE',  ( 121.5321681442453183, -9.988377603198976828, -10.36322818467138340 ) ) ;
#3416 = ORIENTED_EDGE ( 'NONE', *, *, #42304, .F. ) ;
#3417 = CARTESIAN_POINT ( 'NONE',  ( 118.3186931642484438, -2.215723800389698184, -18.16877924232191788 ) ) ;
#3418 = CARTESIAN_POINT ( 'NONE',  ( 118.5256548109119876, -8.899110576539710493, -16.42337572283490132 ) ) ;
#3419 = CYLINDRICAL_SURFACE ( 'NONE', #3138, 3.000000000000001332 ) ;
#3420 = DIRECTION ( 'NONE',  ( 0.000000000000000000, -0.3818493186865927203, 0.9242245927363029745 ) ) ;
#3421 = CARTESIAN_POINT ( 'NONE',  ( 121.7590748109119687, -7.893985811506177619, -18.51759400769804742 ) ) ;
#3422 = CARTESIAN_POINT ( 'NONE',  ( 114.0246765045248196, -2.791137627527939813, -8.388885654883777576 ) ) ;
#3423 = CARTESIAN_POINT ( 'NONE',  ( 71.57611010347959279, -98.31354337915821873, -57.70276321577036782 ) ) ;
#3424 = ORIENTED_EDGE ( 'NONE', *, *, #6923, .T. ) ;
#3425 = CYLINDRICAL_SURFACE ( 'NONE', #13603, 15.90000000000000036 ) ;
#3426 = CARTESIAN_POINT ( 'NONE',  ( 112.4559014775786494, -9.988377603198976828, -10.36322818467138340 ) ) ;
#3427 = CARTESIAN_POINT ( 'NONE',  ( 124.4819548109119722, -7.893985811506177619, -18.51759400769804742 ) ) ;
#3428 = CARTESIAN_POINT ( 'NONE',  ( 118.6958348109119754, -3.505236298600246325, -18.68346056562440793 ) ) ;
#3429 = CARTESIAN_POINT ( 'NONE',  ( 84.38170309240724976, -25.99489077589524300, -13.39321520033831447 ) ) ;
#3430 = CARTESIAN_POINT ( 'NONE',  ( 120.9081748109119872, -5.638512984488999180, -18.83840828888717311 ) ) ;
#3431 = DIRECTION ( 'NONE',  ( -0.9609149988134837450, 0.1028163501681639419, -0.2570431154366518145 ) ) ;
#3432 = CARTESIAN_POINT ( 'NONE',  ( 122.6099748109119929, -0.8288870151387760510, -10.36305467784173118 ) ) ;
#3433 = ORIENTED_EDGE ( 'NONE', *, *, #10899, .F. ) ;
#3434 = CARTESIAN_POINT ( 'NONE',  ( 151.2860562277021472, -4.683672500039348208, -14.88233656108870662 ) ) ;
#3435 = AXIS2_PLACEMENT_3D ( 'NONE', #1407, #18297, #4828 ) ;
#3436 = CARTESIAN_POINT ( 'NONE',  ( 116.4834948109119779, -1.561330072975668504, -17.79121239304076951 ) ) ;
#3437 = CARTESIAN_POINT ( 'NONE',  ( 123.4608748109119745, 0.4262465694468514643, -12.03445270309931736 ) ) ;
#3438 = ORIENTED_EDGE ( 'NONE', *, *, #4563, .T. ) ;
#3439 = CARTESIAN_POINT ( 'NONE',  ( 120.6463454359119822, -11.07370829466463569, -12.81314460846529002 ) ) ;
#3440 = CARTESIAN_POINT ( 'NONE',  ( 136.0320772899241604, -1.215848289962678130, -8.742271026892920460 ) ) ;
#3441 = CARTESIAN_POINT ( 'NONE',  ( 120.8514481442452961, -7.893985811506177619, -18.51759400769804742 ) ) ;
#3442 = CARTESIAN_POINT ( 'NONE',  ( 108.4684265045247997, -7.250697342233347165, -19.15521520033831138 ) ) ;
#3443 = CARTESIAN_POINT ( 'NONE',  ( 120.4543614775786295, -5.574606645277164318, -18.38911715685844683 ) ) ;
#3444 = CIRCLE ( 'NONE', #21632, 8.000000000000001776 ) ;
#3445 = VERTEX_POINT ( 'NONE', #20228 ) ;
#3446 = VERTEX_POINT ( 'NONE', #10631 ) ;
#3447 = CARTESIAN_POINT ( 'NONE',  ( 113.2500748109119968, -6.344957434206662583, -7.627207830600332805 ) ) ;
#3448 = EDGE_CURVE ( 'NONE', #30411, #21756, #39528, .T. ) ;
#3449 = FACE_OUTER_BOUND ( 'NONE', #19455, .T. ) ;
#3450 = CARTESIAN_POINT ( 'NONE',  ( 74.19189222814998175, -41.76310523276723785, -24.39321520033831447 ) ) ;
#3451 =( GEOMETRIC_REPRESENTATION_CONTEXT ( 3 ) GLOBAL_UNCERTAINTY_ASSIGNED_CONTEXT ( ( #12242 ) ) GLOBAL_UNIT_ASSIGNED_CONTEXT ( ( #15675, #12263, #22960 ) ) REPRESENTATION_CONTEXT ( 'NONE', 'WORKASPACE' ) );
#3452 = CARTESIAN_POINT ( 'NONE',  ( 59.44377208703740223, -12.82110557137145967, -17.39288367676203606 ) ) ;
#3453 = CARTESIAN_POINT ( 'NONE',  ( 122.0427081442452817, 0.5811942927096110934, -14.16772938898807510 ) ) ;
#3454 = DIRECTION ( 'NONE',  ( 1.000000000000000000, 0.000000000000000000, 0.000000000000000000 ) ) ;
#3455 = DIRECTION ( 'NONE',  ( 0.000000000000000000, 0.000000000000000000, -1.000000000000000000 ) ) ;
#3456 = CARTESIAN_POINT ( 'NONE',  ( 119.5467348109119712, -4.089484607189486809, -7.948022111789456723 ) ) ;
#3458 = CARTESIAN_POINT ( 'NONE',  ( 120.5110881442453206, -3.505236298600246325, -18.68346056562440793 ) ) ;
#3457 = CARTESIAN_POINT ( 'NONE',  ( 119.8303681442453126, -10.63000616557722466, -14.87417383870573495 ) ) ;
#3459 = CARTESIAN_POINT ( 'NONE',  ( 83.83554121260367253, -25.23119213852205789, -15.24166438581092109 ) ) ;
#3460 = CARTESIAN_POINT ( 'NONE',  ( 115.5191414775786569, -3.383040157471821630, -19.15922257007629170 ) ) ;
#3461 = ORIENTED_EDGE ( 'NONE', *, *, #25980, .F. ) ;
#3462 = DIRECTION ( 'NONE',  ( 0.000000000000000000, 0.000000000000000000, 1.000000000000000000 ) ) ;
#3463 = CARTESIAN_POINT ( 'NONE',  ( 107.0793640045248196, -10.62599879583958717, -11.00651665394454604 ) ) ;
#3464 = CARTESIAN_POINT ( 'NONE',  ( 110.2742077545248094, -2.791137627527939813, -18.39754474579286025 ) ) ;
#3465 = CARTESIAN_POINT ( 'NONE',  ( 108.8851452545248151, 0.8980012041604421569, -11.00651665394454071 ) ) ;
#3466 = EDGE_CURVE ( 'NONE', #12518, #26941, #44871, .T. ) ;
#3467 = AXIS2_PLACEMENT_3D ( 'NONE', #13774, #34281, #20173 ) ;
#3468 = CARTESIAN_POINT ( 'NONE',  ( 124.4252281442452812, -9.261995988541697145, -16.69588392320189030 ) ) ;
#3469 = CARTESIAN_POINT ( 'NONE',  ( 124.8223148109119762, -10.15424416112533912, -14.75197769757731336 ) ) ;
#3470 = VERTEX_POINT ( 'NONE', #6309 ) ;
#3471 = CARTESIAN_POINT ( 'NONE',  ( 123.4608748109119745, -10.63000616557722466, -14.87417383870573495 ) ) ;
#3472 = CARTESIAN_POINT ( 'NONE',  ( 112.0105358795247810, -0.7896495226426338832, -17.46756447353520159 ) ) ;
#3473 = DIRECTION ( 'NONE',  ( 1.000000000000000000, 0.000000000000000000, -0.000000000000000000 ) ) ;
#3474 = CARTESIAN_POINT ( 'NONE',  ( 124.7655881442452852, 0.5811942927096110934, -14.16772938898807510 ) ) ;
#3475 = CARTESIAN_POINT ( 'NONE',  ( 124.4252281442452812, -9.261995988541697145, -16.69588392320189030 ) ) ;
#3476 = DIRECTION ( 'NONE',  ( 0.000000000000000000, -0.3713878862591641905, 0.9284778069183722282 ) ) ;
#3477 = CARTESIAN_POINT ( 'NONE',  ( 126.4106614775786284, -6.222761293078241884, -8.102969835052219238 ) ) ;
#3478 = CARTESIAN_POINT ( 'NONE',  ( 123.6328298109119714, -7.200787124940443817, -17.81845355600750835 ) ) ;
#3479 = CARTESIAN_POINT ( 'NONE',  ( 106.4542858795248179, -0.7896495226426338832, -17.46756447353520159 ) ) ;
#3480 = ORIENTED_EDGE ( 'NONE', *, *, #31833, .F. ) ;
#3481 = CARTESIAN_POINT ( 'NONE',  ( 138.2184548109119930, -2.475900776146298110, -7.888945235271312306 ) ) ;
#3482 = CARTESIAN_POINT ( 'NONE',  ( 114.8384214775786489, -10.15424416112533912, -14.75197769757731336 ) ) ;
#3483 = CARTESIAN_POINT ( 'NONE',  ( 112.3991748109119868, -8.166667518702817929, -8.995218007635859436 ) ) ;
#3484 = CARTESIAN_POINT ( 'NONE',  ( 115.9693640045247776, -10.62599879583958717, -11.00651665394454604 ) ) ;
#3485 = CARTESIAN_POINT ( 'NONE',  ( 108.2600671295247992, 0.1403307496149613920, -13.39321520033831447 ) ) ;
#3486 = CARTESIAN_POINT ( 'NONE',  ( 119.7736414775786358, 0.1319031606808879209, -14.10382304977623669 ) ) ;
#3487 = CARTESIAN_POINT ( 'NONE',  ( 115.8595014775786609, -7.643976991954077427, -18.09477374809248928 ) ) ;
#3488 = CARTESIAN_POINT ( 'NONE',  ( 113.8173414775786512, -9.565557343593413364, -10.61323700422348004 ) ) ;
#3489 = ORIENTED_EDGE ( 'NONE', *, *, #37414, .F. ) ;
#3490 = CARTESIAN_POINT ( 'NONE',  ( 124.1983214775786166, -1.833838273342659697, -17.42832698103878286 ) ) ;
#3491 = FACE_OUTER_BOUND ( 'NONE', #28535, .T. ) ;
#3492 = CARTESIAN_POINT ( 'NONE',  ( 114.7816948109119863, -9.859900752359374465, -12.68260735090039404 ) ) ;
#3493 = ORIENTED_EDGE ( 'NONE', *, *, #37007, .T. ) ;
#3494 = DIRECTION ( 'NONE',  ( -1.224775218828351615E-16, 0.3818493186865896116, -0.9242245927363041957 ) ) ;
#3495 = VERTEX_POINT ( 'NONE', #16813 ) ;
#3496 = CARTESIAN_POINT ( 'NONE',  ( 120.0572748109119772, -6.222761293078241884, -8.102969835052219238 ) ) ;
#3497 = CARTESIAN_POINT ( 'NONE',  ( 112.7962614775786676, -6.222761293078241884, -8.102969835052219238 ) ) ;
#3498 = CARTESIAN_POINT ( 'NONE',  ( 109.2294421295247844, 0.1210096558822565393, -14.64321520034217805 ) ) ;
#3499 = CARTESIAN_POINT ( 'NONE',  ( 122.3132204359119868, -10.25716656981731489, -12.88942061488890545 ) ) ;
#3500 = ORIENTED_EDGE ( 'NONE', *, *, #35952, .F. ) ;
#3501 = FACE_OUTER_BOUND ( 'NONE', #32187, .T. ) ;
#3502 = CARTESIAN_POINT ( 'NONE',  ( 124.6574308310801058, -0.1064883412648260086, -7.172770542335224597 ) ) ;
#3503 = CARTESIAN_POINT ( 'NONE',  ( 115.7610046295247912, -4.863998795839590272, -7.631215200338315796 ) ) ;
#3504 = CARTESIAN_POINT ( 'NONE',  ( 115.6915515045247531, -6.936859964151197211, -18.39754474579287447 ) ) ;
#3505 = CARTESIAN_POINT ( 'NONE',  ( 121.3052614775786111, -7.643976991954077427, -18.09477374809248928 ) ) ;
#3506 = CARTESIAN_POINT ( 'NONE',  ( 118.7525614775786380, -1.833838273342659253, -17.42832698103878286 ) ) ;
#3507 = LINE ( 'NONE', #91, #10477 ) ;
#3508 = ORIENTED_EDGE ( 'NONE', *, *, #40922, .T. ) ;
#3509 = LINE ( 'NONE', #93, #21514 ) ;
#3510 = CARTESIAN_POINT ( 'NONE',  ( 115.9162281442453235, -5.574606645277164318, -18.38911715685844683 ) ) ;
#3511 = CARTESIAN_POINT ( 'NONE',  ( 122.6009548109119720, 2.753894863294152007, -15.83610205775420177 ) ) ;
#3512 = CARTESIAN_POINT ( 'NONE',  ( 84.51109360120413783, -29.99489077589588959, -12.39321520033831625 ) ) ;
#3513 = CARTESIAN_POINT ( 'NONE',  ( 124.8223148109119762, 0.9020085738987339008, -11.91225656197089222 ) ) ;
#3514 = CARTESIAN_POINT ( 'NONE',  ( 114.8384214775786489, 0.9020085738987339008, -11.91225656197089222 ) ) ;
#3515 = VERTEX_POINT ( 'NONE', #45066 ) ;
#3516 = CARTESIAN_POINT ( 'NONE',  ( 114.7249681442453237, 0.2603800115204892296, -16.42320221600525088 ) ) ;
#3517 = CARTESIAN_POINT ( 'NONE',  ( 74.19189222814998175, -41.76310523276723785, -20.39321520033831447 ) ) ;
#3518 = CARTESIAN_POINT ( 'NONE',  ( 115.3442858795247759, -0.7896495226426338832, -17.46756447353520159 ) ) ;
#3519 = CARTESIAN_POINT ( 'NONE',  ( 112.2289948109119848, -1.834011780172310813, -8.268836392978581529 ) ) ;
#3520 = CARTESIAN_POINT ( 'NONE',  ( 113.5337081442453240, -9.261995988541697145, -16.69588392320189030 ) ) ;
#3521 = CARTESIAN_POINT ( 'NONE',  ( 123.9146881442452894, -10.15424416112533912, -14.75197769757731336 ) ) ;
#3522 = LINE ( 'NONE', #30675, #3832 ) ;
#3523 = CARTESIAN_POINT ( 'NONE',  ( 109.9963952545248134, -9.868328341294098749, -15.46607636864997204 ) ) ;
#3524 = CARTESIAN_POINT ( 'NONE',  ( 111.3854577545248503, -7.250697342233347165, -7.631215200338321125 ) ) ;
#3525 = CARTESIAN_POINT ( 'NONE',  ( 109.2295012951870348, -4.728831740048331511, -18.57600240304503103 ) ) ;
#3526 = CARTESIAN_POINT ( 'NONE',  ( 117.2209414775786485, -2.084020599724406786, -8.691656652584148546 ) ) ;
#3527 = CARTESIAN_POINT ( 'NONE',  ( 107.9128015045248219, -2.477300249445798297, -7.631215200338321125 ) ) ;
#3528 = AXIS2_PLACEMENT_3D ( 'NONE', #44929, #10487, #31887 ) ;
#3529 = CARTESIAN_POINT ( 'NONE',  ( 83.72016463086879412, -25.99489077589524300, -13.39321520033831447 ) ) ;
#3530 = CARTESIAN_POINT ( 'NONE',  ( 108.7462390045248242, 0.8980012041604421569, -15.77991374673208469 ) ) ;
#3531 = CARTESIAN_POINT ( 'NONE',  ( 123.9714148109119805, -0.4660016031367893996, -10.09054647747474043 ) ) ;
#3532 = CARTESIAN_POINT ( 'NONE',  ( 111.4348214775786801, -3.505236298600246325, -18.68346056562440793 ) ) ;
#3533 = CARTESIAN_POINT ( 'NONE',  ( 120.0572748109119772, -6.222761293078222344, -8.102969835052219238 ) ) ;
#3534 = CARTESIAN_POINT ( 'NONE',  ( 119.0361948109119652, -7.893985811506177619, -18.51759400769804742 ) ) ;
#3535 = EDGE_CURVE ( 'NONE', #22322, #2225, #31363, .T. ) ;
#3536 = CARTESIAN_POINT ( 'NONE',  ( 115.3489614775786407, -9.261995988541697145, -16.69588392320189030 ) ) ;
#3537 = ORIENTED_EDGE ( 'NONE', *, *, #23345, .F. ) ;
#3538 = CARTESIAN_POINT ( 'NONE',  ( 114.9518748109119883, -7.643976991954077427, -18.09477374809248928 ) ) ;
#3539 = CARTESIAN_POINT ( 'NONE',  ( 123.6310548109119765, -5.638512984488999180, -18.83840828888717311 ) ) ;
#3540 = CARTESIAN_POINT ( 'NONE',  ( 119.2631014775786298, 0.2603800115204892296, -16.42320221600525088 ) ) ;
#3541 = CARTESIAN_POINT ( 'NONE',  ( 115.9162281442453093, -5.574606645277164318, -18.38911715685844683 ) ) ;
#3542 = VERTEX_POINT ( 'NONE', #20895 ) ;
#3543 = CARTESIAN_POINT ( 'NONE',  ( 121.1350814775786233, -9.859900752359378018, -12.68260735090039759 ) ) ;
#3544 = CARTESIAN_POINT ( 'NONE',  ( 116.3700414775786527, -5.638512984488999180, -18.83840828888717311 ) ) ;
#3545 = CARTESIAN_POINT ( 'NONE',  ( 136.9735043287622318, 0.6043515321839462162, -13.01395506536901436 ) ) ;
#3546 = CARTESIAN_POINT ( 'NONE',  ( 115.0664733795247798, -8.938348069036489818, -17.46756447353520159 ) ) ;
#3547 = EDGE_LOOP ( 'NONE', ( #18988, #39471, #22113, #36114 ) ) ;
#3548 = CARTESIAN_POINT ( 'NONE',  ( 65.70869026611384811, -0.1917948075113792838, -10.71553487254586656 ) ) ;
#3549 = DIRECTION ( 'NONE',  ( 0.9609149988134837450, -0.1028163501681639419, 0.2570431154366518145 ) ) ;
#3550 = EDGE_CURVE ( 'NONE', #31200, #33021, #416, .T. ) ;
#3551 = DIRECTION ( 'NONE',  ( 0.000000000000000000, -0.9554676365605411226, -0.2950959089608217178 ) ) ;
#3552 = CARTESIAN_POINT ( 'NONE',  ( 113.2500748109119968, -6.344957434206662583, -7.627207830600332805 ) ) ;
#3553 = TOROIDAL_SURFACE ( 'NONE', #29051, 3.100000000000000089, 2.899999999999999911 ) ;
#3554 = CYLINDRICAL_SURFACE ( 'NONE', #2590, 1.499999999999998002 ) ;
#3555 = DIRECTION ( 'NONE',  ( -0.000000000000000000, -0.9284778069183718952, -0.3713878862591649677 ) ) ;
#3556 = EDGE_CURVE ( 'NONE', #26284, #42482, #31021, .T. ) ;
#3557 = CARTESIAN_POINT ( 'NONE',  ( 63.16361418624702395, -12.63457483197140085, -16.47427386053546527 ) ) ;
#3558 = B_SPLINE_CURVE_WITH_KNOTS ( 'NONE', 3,
 ( #8834, #25943, #36634, #26843, #9512, #12492, #40300, #9064, #23429, #43501 ),
 .UNSPECIFIED., .F., .F.,
 ( 4, 3, 3, 4 ),
 ( 0.000000000000000000, 0.0001671877560958105107, 0.0003343755126086549959, 0.0006438490228505499516 ),
 .UNSPECIFIED. ) ;
#3559 = DIRECTION ( 'NONE',  ( 0.9609149988134843001, -0.1028163501681632064, 0.2570431154366505933 ) ) ;
#3560 = CARTESIAN_POINT ( 'NONE',  ( 113.3995983795247895, -8.402594152722688392, -16.93181055722141792 ) ) ;
#3561 = CARTESIAN_POINT ( 'NONE',  ( 118.9227414775786400, -10.63000616557722466, -14.87417383870573495 ) ) ;
#3562 = CYLINDRICAL_SURFACE ( 'NONE', #26727, 1.199999999999996625 ) ;
#3563 = ADVANCED_FACE ( 'NONE', ( #35217 ), #21555, .F. ) ;
#3564 = CARTESIAN_POINT ( 'NONE',  ( 87.02785693856107230, -27.84333996136784961, -14.15691383771150136 ) ) ;
#3565 = B_SPLINE_CURVE_WITH_KNOTS ( 'NONE', 3,
 ( #27559, #6356, #33924, #17298, #20495, #31190, #27107, #45108, #13432, #34155 ),
 .UNSPECIFIED., .F., .F.,
 ( 4, 3, 3, 4 ),
 ( 9.263427422397549112E-19, 1.415135068336276058E-06, 2.830270136674489704E-06, 5.511645061733400693E-06 ),
 .UNSPECIFIED. ) ;
#3566 = CARTESIAN_POINT ( 'NONE',  ( 125.1059481442452750, -1.833838273342660141, -17.42832698103878286 ) ) ;
#3567 = ORIENTED_EDGE ( 'NONE', *, *, #17796, .T. ) ;
#3568 = DIRECTION ( 'NONE',  ( 0.000000000000000000, 0.000000000000000000, -1.000000000000000000 ) ) ;
#3569 = CARTESIAN_POINT ( 'NONE',  ( 120.3409081442453044, -0.4660016031367893996, -10.09054647747474043 ) ) ;
#3570 = CARTESIAN_POINT ( 'NONE',  ( 76.69189222814998175, -55.76602098829192755, -2.607500914624014232 ) ) ;
#3571 = CARTESIAN_POINT ( 'NONE',  ( 114.4413348109119823, -0.8288870151387760510, -10.36305467784173118 ) ) ;
#3572 = ADVANCED_FACE ( 'NONE', ( #11749 ), #21101, .F. ) ;
#3573 = CARTESIAN_POINT ( 'NONE',  ( 112.0020881442453344, -9.565557343593413364, -10.61323700422348004 ) ) ;
#3574 = CARTESIAN_POINT ( 'NONE',  ( 105.4124890045248293, -9.868328341294098749, -11.32035403202665869 ) ) ;
#3575 = CARTESIAN_POINT ( 'NONE',  ( 113.0523327545247838, -2.477300249445798297, -19.15521520033831138 ) ) ;
#3576 = CARTESIAN_POINT ( 'NONE',  ( 119.8303681442453126, 0.4262465694468514643, -12.03445270309931736 ) ) ;
#3577 = CARTESIAN_POINT ( 'NONE',  ( 120.7379948109119709, 0.4262465694468514643, -12.03445270309931736 ) ) ;
#3578 = CARTESIAN_POINT ( 'NONE',  ( 109.2294421680114596, -0.2361213814094521024, -10.76286691213928748 ) ) ;
#3579 = CARTESIAN_POINT ( 'NONE',  ( 107.1488171295247867, 0.1403307496149613920, -13.39321520033831447 ) ) ;
#3580 = B_SPLINE_CURVE_WITH_KNOTS ( 'NONE', 3,
 ( #38872, #32031, #14718, #28629, #32257, #1025, #14943 ),
 .UNSPECIFIED., .F., .F.,
 ( 4, 3, 4 ),
 ( 0.0003705783391767355139, 0.0004952974148303549741, 0.0009534114850261810395 ),
 .UNSPECIFIED. ) ;
#3581 = EDGE_CURVE ( 'NONE', #39890, #16741, #33183, .T. ) ;
#3582 = CARTESIAN_POINT ( 'NONE',  ( 109.2292940338004286, -1.048241503082447457, -16.67292528126275641 ) ) ;
#3583 = CARTESIAN_POINT ( 'NONE',  ( 112.9097148109120070, 0.2603800115204892296, -16.42320221600525088 ) ) ;
#3584 = CARTESIAN_POINT ( 'NONE',  ( 116.2565881442452991, -9.261995988541697145, -16.69588392320189030 ) ) ;
#3585 = CARTESIAN_POINT ( 'NONE',  ( 109.1629577545248395, -7.250697342233347165, -7.631215200338321125 ) ) ;
#3586 = CARTESIAN_POINT ( 'NONE',  ( 121.8270485609119760, -0.08252387247370887580, -11.91645802438286417 ) ) ;
#3587 = ADVANCED_FACE ( 'NONE', ( #25434 ), #22003, .F. ) ;
#3588 = EDGE_CURVE ( 'NONE', #33401, #14434, #4777, .T. ) ;
#3589 = ORIENTED_EDGE ( 'NONE', *, *, #34569, .T. ) ;
#3590 = DIRECTION ( 'NONE',  ( 0.000000000000000000, 0.6004852223388321697, -0.7996358532186279566 ) ) ;
#3591 = CARTESIAN_POINT ( 'NONE',  ( 122.4397948109119767, -9.988377603198976828, -10.36322818467138340 ) ) ;
#3592 = CARTESIAN_POINT ( 'NONE',  ( 113.9875214775786532, -0.4660016031367893996, -10.09054647747474043 ) ) ;
#3593 = CARTESIAN_POINT ( 'NONE',  ( 118.3554748109119998, -9.565557343593413364, -10.61323700422348004 ) ) ;
#3594 = CARTESIAN_POINT ( 'NONE',  ( 123.6877814775786533, -3.383040157471821630, -19.15922257007629170 ) ) ;
#3595 = CARTESIAN_POINT ( 'NONE',  ( 119.2063748109119814, -1.561330072975668504, -17.79121239304076951 ) ) ;
#3596 = CARTESIAN_POINT ( 'NONE',  ( 108.3295202545248657, 0.1403307496149616695, -11.32035403202665336 ) ) ;
#3597 = CARTESIAN_POINT ( 'NONE',  ( 113.1366214775786432, -7.643976991954077427, -18.09477374809248928 ) ) ;
#3598 = DIRECTION ( 'NONE',  ( 0.000000000000000000, -1.000000000000000000, 0.000000000000000000 ) ) ;
#3599 = ORIENTED_EDGE ( 'NONE', *, *, #39791, .F. ) ;
#3600 = CARTESIAN_POINT ( 'NONE',  ( 122.8368814775786291, -1.561330072975668948, -17.79121239304076951 ) ) ;
#3601 = CARTESIAN_POINT ( 'NONE',  ( 120.5768923109119868, -9.959231468620755479, -10.70263013195267199 ) ) ;
#3602 = CARTESIAN_POINT ( 'NONE',  ( 115.9729548109119861, -6.344957434206662583, -7.627207830600332805 ) ) ;
#3603 = VERTEX_POINT ( 'NONE', #35443 ) ;
#3604 = CARTESIAN_POINT ( 'NONE',  ( 113.8857702545248003, -10.62599879583958717, -15.77991374673208469 ) ) ;
#3605 = CARTESIAN_POINT ( 'NONE',  ( 138.2184548109119930, -7.050714571525749541, -18.72418924296322729 ) ) ;
#3606 = CARTESIAN_POINT ( 'NONE',  ( 122.4397948109119767, -9.988377603198980381, -10.36322818467138518 ) ) ;
#3607 = CARTESIAN_POINT ( 'NONE',  ( 116.0861162244890892, -0.02276961308034231024, -12.14321520033833934 ) ) ;
#3608 = CARTESIAN_POINT ( 'NONE',  ( 124.4694423109119725, -9.285408612553634811, -11.05844856689041755 ) ) ;
#3609 = CARTESIAN_POINT ( 'NONE',  ( 119.1496481442453046, -6.222761293078241884, -8.102969835052219238 ) ) ;
#3610 = CARTESIAN_POINT ( 'NONE',  ( 120.5468302440515203, -2.467220198592778413, -17.83387418641524391 ) ) ;
#3611 = CARTESIAN_POINT ( 'NONE',  ( 121.4754414775786131, -1.833838273342659697, -17.42832698103878286 ) ) ;
#3612 = EDGE_CURVE ( 'NONE', #14619, #21831, #36833, .T. ) ;
#3613 = CIRCLE ( 'NONE', #9450, 3.500000000000003109 ) ;
#3614 = CARTESIAN_POINT ( 'NONE',  ( 125.1433143116076678, -11.83481241714331489, -10.81293854524298936 ) ) ;
#3615 = CARTESIAN_POINT ( 'NONE',  ( 121.0216281442452981, -7.894159318335828068, -9.358103419637847864 ) ) ;
#3616 = CARTESIAN_POINT ( 'NONE',  ( 121.4103298109119748, -2.173413727453600508, -8.297982527556802879 ) ) ;
#3617 = CARTESIAN_POINT ( 'NONE',  ( 115.3489614775786407, -9.261995988541697145, -16.69588392320189030 ) ) ;
#3618 = CARTESIAN_POINT ( 'NONE',  ( 123.1772414775786189, -4.089484607189477039, -7.948022111789462052 ) ) ;
#3619 = CARTESIAN_POINT ( 'NONE',  ( 116.9373081442452929, -1.833838273342659253, -17.42832698103878286 ) ) ;
#3620 = EDGE_LOOP ( 'NONE', ( #6263, #33817, #3948, #26256, #121 ) ) ;
#3621 = CARTESIAN_POINT ( 'NONE',  ( 116.7104014775786425, -0.4660016031367893996, -10.09054647747474043 ) ) ;
#3622 = CARTESIAN_POINT ( 'NONE',  ( 107.9128015045248219, -2.477300249445798297, -7.631215200338321125 ) ) ;
#3623 = DIRECTION ( 'NONE',  ( 1.000000000000000000, 0.000000000000000000, 0.000000000000000000 ) ) ;
#3624 = DIRECTION ( 'NONE',  ( 0.000000000000000000, 0.000000000000000000, 1.000000000000000000 ) ) ;
#3625 = AXIS2_PLACEMENT_3D ( 'NONE', #11633, #18703, #11864 ) ;
#3626 = FACE_OUTER_BOUND ( 'NONE', #182, .T. ) ;
#3627 = CARTESIAN_POINT ( 'NONE',  ( 120.7947214775786193, -9.261995988541697145, -16.69588392320189030 ) ) ;
#3628 = ORIENTED_EDGE ( 'NONE', *, *, #21656, .F. ) ;
#3629 = VECTOR ( 'NONE', #43163, 1000.000000000000000 ) ;
#3630 = CARTESIAN_POINT ( 'NONE',  ( 116.0286950891469786, 2.331313199634366118, -14.64321520033831447 ) ) ;
#3631 = CARTESIAN_POINT ( 'NONE',  ( 117.5613014775786525, -10.15424416112533912, -14.75197769757731336 ) ) ;
#3632 = CARTESIAN_POINT ( 'NONE',  ( 63.78480611294602909, -13.55202615601718463, -18.34317296867338598 ) ) ;
#3633 = EDGE_CURVE ( 'NONE', #12590, #43250, #35717, .T. ) ;
#3634 = CARTESIAN_POINT ( 'NONE',  ( 123.5176014775786228, -9.261995988541697145, -16.69588392320189030 ) ) ;
#3635 = CARTESIAN_POINT ( 'NONE',  ( 112.1494421295248003, -9.868328341294093420, -13.39321520033831447 ) ) ;
#3636 = CARTESIAN_POINT ( 'NONE',  ( 89.27431095563446206, -9.970335341274866536, -13.62791168839721578 ) ) ;
#3637 = ORIENTED_EDGE ( 'NONE', *, *, #18352, .T. ) ;
#3638 = CARTESIAN_POINT ( 'NONE',  ( 115.6893214775786447, 0.5811942927096154232, -14.16772938898807155 ) ) ;
#3639 = CARTESIAN_POINT ( 'NONE',  ( 126.4106614775786284, -6.222761293078241884, -8.102969835052219238 ) ) ;
#3640 = CARTESIAN_POINT ( 'NONE',  ( 123.9146881442452894, 0.9020085738987339008, -11.91225656197089222 ) ) ;
#3641 = CARTESIAN_POINT ( 'NONE',  ( 117.6747548109119919, -7.643976991954077427, -18.09477374809248928 ) ) ;
#3642 = CARTESIAN_POINT ( 'NONE',  ( 61.69189222814998175, -66.48243304680813992, -42.55772070205831170 ) ) ;
#3643 = CARTESIAN_POINT ( 'NONE',  ( 68.68839935636917460, -25.95913848132418522, -5.893215200338315363 ) ) ;
#3644 = CARTESIAN_POINT ( 'NONE',  ( 119.4332814775786318, -0.4660016031367893996, -10.09054647747474043 ) ) ;
#3645 = FACE_OUTER_BOUND ( 'NONE', #37899, .T. ) ;
#3646 = EDGE_CURVE ( 'NONE', #44662, #3847, #3580, .T. ) ;
#3647 = CARTESIAN_POINT ( 'NONE',  ( 124.0281414775786146, -7.643976991954077427, -18.09477374809248928 ) ) ;
#3648 = EDGE_LOOP ( 'NONE', ( #18266, #15979, #3658, #17310 ) ) ;
#3649 = CARTESIAN_POINT ( 'NONE',  ( 120.0947965460471920, -2.191907684172563986, -18.20049396185734025 ) ) ;
#3650 = CARTESIAN_POINT ( 'NONE',  ( 117.3343948109119737, -3.383040157471821630, -19.15922257007629170 ) ) ;
#3651 = CARTESIAN_POINT ( 'NONE',  ( 125.6164881442453094, -9.565557343593413364, -10.61323700422348004 ) ) ;
#3652 = ORIENTED_EDGE ( 'NONE', *, *, #782, .T. ) ;
#3653 =( BOUNDED_SURFACE ( )  B_SPLINE_SURFACE ( 1, 2, ( 
 ( #18052, #8009, #21918, #35811, #1165, #18506, #32396, #15082, #43572, #12342, #37155, #40605, #29659, #16438, #5931, #6166, #30116, #13018, #23273, #5257, #26241, #43803, #15758, #26019, #44262, #5703, #40152, #20086, #33285, #2739, #39924, #33504, #8915, #36708, #22813, #5476, #19396, #19853, #9364, #2060, #30336, #33740, #33971, #44031, #26917, #2512, #19174, #15983, #12569, #29886, #8685, #2283, #16664, #43346, #36931, #26474, #12116, #33054, #40377, #9140, #23044, #40838, #1828, #9593, #19620, #23509, #37394, #22590, #16213, #36490, #12792, #26694, #37627, #27373, #41515, #7062, #27601, #34844, #24177, #38498, #27148, #30558, #10270, #6401, #7275, #27815, #41729, #38282, #13906, #20753, #24615, #17549, #20972, #17117, #35068, #3631, #6619, #31443, #21190, #44479, #20307, #20532, #14125, #211, #38069, #34412, #28042, #41950, #16895, #23960, #6846, #34632, #3418, #41295, #3849, #41069, #9826, #17334, #2967, #31224, #34193, #10492, #3193, #24278, #30788, #24394, #10057, #10714, #13246, #31007, #23737, #44711, #13472, #37843, #44934, #13692, #11606, #25517, #4069, #39420, #35527, #39187, #31892, #43066, #11385, #28264, #8411, #42622, #14350, #22094, #42173, #8185, #31665, #35759, #434, #24835, #35981, #4752, #25065, #38958, #7726, #25293, #38726, #11160, #1109, #18673, #4530, #10933, #15027, #14574, #1332, #7498, #15246, #32565, #35296, #28491, #4299, #7953, #18454, #21414, #17993, #11834, #36211, #29154, #25742, #42396, #28937, #39648, #659, #22316, #42846, #21639, #17769, #18220, #32115, #21864, #883, #14802, #28715, #32342, #22536, #9087, #8855, #5649, #43748, #12515, #26865, #8635, #33003, #2006, #22756, #22989, #33683, #1553, #36879, #40554, #15475, #19346, #2228, #29605, #36433, #43521, #16380, #23453, #26640, #26413, #2458, #19569, #40096, #40323, #1777, #4978, #32781, #12289, #30282, #26187, #29831, #5200, #25965, #18890, #36656, #19119, #33448, #5429, #16157, #15932, #30061, #33233, #29381, #44208, #43974, #9314, #12738, #23223, #37102, #43293, #5877 ),
 ( #19798, #12969, #12063, #15703, #40780, #9538, #39870, #27549, #41901, #10666, #30959, #27325, #14078, #27095, #9771, #41242, #41683, #23910, #34799, #31178, #3146, #3583, #45098, #16843, #13855, #27770, #23683, #10444, #10001, #13640, #6342, #17494, #44883, #2682, #27996, #17067, #33911, #24348, #16613, #38235, #7015, #41461, #20257, #162, #37793, #37338, #30506, #10220, #37572, #30735, #34143, #2912, #44658, #20925, #34584, #13421, #31393, #6110, #20029, #24129, #44427, #17287, #13195, #6567, #20485, #34364, #41017, #38021, #6797, #20706, #3368, #14524, #1287, #14301, #42126, #28437, #42350, #32295, #28219, #1060, #25011, #35706, #14975, #4482, #38677, #22040, #25243, #35934, #31619, #21363, #35477, #28888, #21590, #42800, #18168, #32512, #21139, #24569, #4251, #388, #15199, #21813, #18403, #11561, #7906, #14752, #18622, #25468, #39372, #11109, #29103, #8139, #613, #4702, #43014, #38454, #10886, #38904, #7225, #35015, #32065, #7675, #3795, #17721, #24785, #17945, #833, #28665, #42569, #35246, #7443, #4023, #31844, #11332, #39141, #5380, #32731, #22933, #29553, #19297, #18839, #33175, #22484, #26587, #9036, #36826, #19519, #40269, #1952, #5821, #43919, #2170, #43470, #16329, #33396, #32950, #30003, #19741, #11783, #1505, #1727, #40500, #16100, #22707, #15649, #12688, #9261, #43244, #5149, #15878, #36605, #29775, #8584, #2401, #8358, #22262, #43686, #29330, #12461, #15425, #5595, #12236, #26362, #12010, #23171, #36378, #37050, #33625, #26133, #30231, #25690, #39597, #36156, #4925, #19066, #25912, #39817, #40037, #8803, #16789, #20431, #13138, #24300, #37746, #9482, #34749, #23860, #40725, #3310, #23395, #37970, #45049, #6516, #27042, #6964, #34092, #3531, #37281, #34315, #16561, #37513, #40959, #44376, #9714, #6746, #41416, #30456, #17233, #20655, #20871, #30906, #13809, #24077, #6048, #23627, #44604, #6286, #26814, #3088, #17447, #44153, #17015, #2858, #12918, #33859, #20207, #30685, #13367, #34532, #2628, #31124, #27272, #10170, #27720, #41635, #41186, #10391 ) ),
 .UNSPECIFIED., .F., .F., .F. ) 
 B_SPLINE_SURFACE_WITH_KNOTS ( ( 2, 2 ),
 ( 3, 2, 2, 2, 2, 2, 2, 2, 2, 2, 2, 2, 2, 2, 2, 2, 2, 2, 2, 2, 2, 2, 2, 2, 2, 2, 2, 2, 2, 2, 2, 2, 2, 2, 2, 2, 2, 2, 2, 2, 2, 2, 2, 2, 2, 2, 2, 2, 2, 2, 2, 2, 2, 2, 2, 2, 2, 2, 2, 2, 2, 2, 2, 2, 2, 2, 2, 2, 2, 2, 2, 2, 2, 2, 2, 2, 2, 2, 2, 2, 2, 2, 2, 2, 2, 2, 2, 2, 2, 2, 2, 2, 2, 2, 2, 2, 2, 2, 2, 2, 2, 2, 2, 2, 2, 2, 2, 2, 2, 2, 2, 2, 2, 2, 2, 2, 2, 2, 2, 2, 2, 2, 2, 2, 2, 2, 2, 2, 3 ),
 ( 0.000000000000000000, 1.000000000000000000 ),
 ( 0.000000000000000000, 0.007812500000000000000, 0.01562500000000000000, 0.02343750000000000000, 0.03125000000000000000, 0.03906250000000000000, 0.04687500000000000000, 0.05468750000000000000, 0.06250000000000000000, 0.07031250000000000000, 0.07812500000000000000, 0.08593750000000000000, 0.09375000000000000000, 0.1015625000000000000, 0.1093750000000000000, 0.1171875000000000000, 0.1250000000000000000, 0.1328125000000000000, 0.1406250000000000000, 0.1484375000000000000, 0.1562500000000000000, 0.1640625000000000000, 0.1718750000000000000, 0.1796875000000000000, 0.1875000000000000000, 0.1953125000000000000, 0.2031250000000000000, 0.2109375000000000000, 0.2187500000000000000, 0.2265625000000000000, 0.2343750000000000000, 0.2421875000000000000, 0.2500000000000000000, 0.2578125000000000000, 0.2656250000000000000, 0.2734375000000000000, 0.2812500000000000000, 0.2890625000000000000, 0.2968750000000000000, 0.3046875000000000000, 0.3125000000000000000, 0.3203125000000000000, 0.3281250000000000000, 0.3359375000000000000, 0.3437500000000000000, 0.3515625000000000000, 0.3593750000000000000, 0.3671875000000000000, 0.3750000000000000000, 0.3828125000000000000, 0.3906250000000000000, 0.3984375000000000000, 0.4062500000000000000, 0.4140625000000000000, 0.4218750000000000000, 0.4296875000000000000, 0.4375000000000000000, 0.4453125000000000000, 0.4531250000000000000, 0.4609375000000000000, 0.4687500000000000000, 0.4765625000000000000, 0.4843750000000000000, 0.4921875000000000000, 0.5000000000000000000, 0.5078125000000000000, 0.5156250000000000000, 0.5234375000000000000, 0.5312500000000000000, 0.5390625000000000000, 0.5468750000000000000, 0.5546875000000000000, 0.5625000000000000000, 0.5703125000000000000, 0.5781250000000000000, 0.5859375000000000000, 0.5937500000000000000, 0.6015625000000000000, 0.6093750000000000000, 0.6171875000000000000, 0.6250000000000000000, 0.6328125000000000000, 0.6406250000000000000, 0.6484375000000000000, 0.6562500000000000000, 0.6640625000000000000, 0.6718750000000000000, 0.6796875000000000000, 0.6875000000000000000, 0.6953125000000000000, 0.7031250000000000000, 0.7109375000000000000, 0.7187500000000000000, 0.7265625000000000000, 0.7343750000000000000, 0.7421875000000000000, 0.7500000000000000000, 0.7578125000000000000, 0.7656250000000000000, 0.7734375000000000000, 0.7812500000000000000, 0.7890625000000000000, 0.7968750000000000000, 0.8046875000000000000, 0.8125000000000000000, 0.8203125000000000000, 0.8281250000000000000, 0.8359375000000000000, 0.8437500000000000000, 0.8515625000000000000, 0.8593750000000000000, 0.8671875000000000000, 0.8750000000000000000, 0.8828125000000000000, 0.8906250000000000000, 0.8984375000000000000, 0.9062500000000000000, 0.9140625000000000000, 0.9218750000000000000, 0.9296875000000000000, 0.9375000000000000000, 0.9453125000000000000, 0.9531250000000000000, 0.9609375000000000000, 0.9687500000000000000, 0.9765625000000000000, 0.9843750000000000000, 0.9921875000000000000, 1.000000000000000000 ),
 .UNSPECIFIED. ) 
 GEOMETRIC_REPRESENTATION_ITEM ( )  RATIONAL_B_SPLINE_SURFACE ( (
 ( 1.000000000000000000, 0.9238795325112869605, 1.000000000000000000, 0.9238795325112869605, 1.000000000000000000, 0.9238795325112869605, 1.000000000000000000, 0.9238795325112869605, 1.000000000000000000, 0.9238795325112869605, 1.000000000000000000, 0.9238795325112869605, 1.000000000000000000, 0.9238795325112869605, 1.000000000000000000, 0.9238795325112869605, 1.000000000000000000, 0.9238795325112869605, 1.000000000000000000, 0.9238795325112869605, 1.000000000000000000, 0.9238795325112869605, 1.000000000000000000, 0.9238795325112869605, 1.000000000000000000, 0.9238795325112869605, 1.000000000000000000, 0.9238795325112869605, 1.000000000000000000, 0.9238795325112869605, 1.000000000000000000, 0.9238795325112869605, 1.000000000000000000, 0.9238795325112869605, 1.000000000000000000, 0.9238795325112869605, 1.000000000000000000, 0.9238795325112869605, 1.000000000000000000, 0.9238795325112869605, 1.000000000000000000, 0.9238795325112869605, 1.000000000000000000, 0.9238795325112869605, 1.000000000000000000, 0.9238795325112869605, 1.000000000000000000, 0.9238795325112869605, 1.000000000000000000, 0.9238795325112869605, 1.000000000000000000, 0.9238795325112869605, 1.000000000000000000, 0.9238795325112869605, 1.000000000000000000, 0.9238795325112869605, 1.000000000000000000, 0.9238795325112869605, 1.000000000000000000, 0.9238795325112869605, 1.000000000000000000, 0.9238795325112869605, 1.000000000000000000, 0.9238795325112869605, 1.000000000000000000, 0.9238795325112869605, 1.000000000000000000, 0.9238795325112869605, 1.000000000000000000, 0.9238795325112869605, 1.000000000000000000, 0.9238795325112869605, 1.000000000000000000, 0.9238795325112869605, 1.000000000000000000, 0.9238795325112869605, 1.000000000000000000, 0.9238795325112869605, 1.000000000000000000, 0.9238795325112869605, 1.000000000000000000, 0.9238795325112869605, 1.000000000000000000, 0.9238795325112869605, 1.000000000000000000, 0.9238795325112869605, 1.000000000000000000, 0.9238795325112869605, 1.000000000000000000, 0.9238795325112869605, 1.000000000000000000, 0.9238795325112869605, 1.000000000000000000, 0.9238795325112869605, 1.000000000000000000, 0.9238795325112869605, 1.000000000000000000, 0.9238795325112869605, 1.000000000000000000, 0.9238795325112869605, 1.000000000000000000, 0.9238795325112869605, 1.000000000000000000, 0.9238795325112869605, 1.000000000000000000, 0.9238795325112869605, 1.000000000000000000, 0.9238795325112869605, 1.000000000000000000, 0.9238795325112869605, 1.000000000000000000, 0.9238795325112869605, 1.000000000000000000, 0.9238795325112869605, 1.000000000000000000, 0.9238795325112869605, 1.000000000000000000, 0.9238795325112869605, 1.000000000000000000, 0.9238795325112869605, 1.000000000000000000, 0.9238795325112869605, 1.000000000000000000, 0.9238795325112869605, 1.000000000000000000, 0.9238795325112869605, 1.000000000000000000, 0.9238795325112869605, 1.000000000000000000, 0.9238795325112869605, 1.000000000000000000, 0.9238795325112869605, 1.000000000000000000, 0.9238795325112869605, 1.000000000000000000, 0.9238795325112869605, 1.000000000000000000, 0.9238795325112869605, 1.000000000000000000, 0.9238795325112869605, 1.000000000000000000, 0.9238795325112869605, 1.000000000000000000, 0.9238795325112869605, 1.000000000000000000, 0.9238795325112869605, 1.000000000000000000, 0.9238795325112869605, 1.000000000000000000, 0.9238795325112869605, 1.000000000000000000, 0.9238795325112869605, 1.000000000000000000, 0.9238795325112869605, 1.000000000000000000, 0.9238795325112869605, 1.000000000000000000, 0.9238795325112869605, 1.000000000000000000, 0.9238795325112869605, 1.000000000000000000, 0.9238795325112869605, 1.000000000000000000, 0.9238795325112869605, 1.000000000000000000, 0.9238795325112869605, 1.000000000000000000, 0.9238795325112869605, 1.000000000000000000, 0.9238795325112869605, 1.000000000000000000, 0.9238795325112869605, 1.000000000000000000, 0.9238795325112869605, 1.000000000000000000, 0.9238795325112869605, 1.000000000000000000, 0.9238795325112869605, 1.000000000000000000, 0.9238795325112869605, 1.000000000000000000, 0.9238795325112869605, 1.000000000000000000, 0.9238795325112869605, 1.000000000000000000, 0.9238795325112869605, 1.000000000000000000, 0.9238795325112869605, 1.000000000000000000, 0.9238795325112869605, 1.000000000000000000, 0.9238795325112869605, 1.000000000000000000, 0.9238795325112869605, 1.000000000000000000, 0.9238795325112869605, 1.000000000000000000, 0.9238795325112869605, 1.000000000000000000, 0.9238795325112869605, 1.000000000000000000, 0.9238795325112869605, 1.000000000000000000, 0.9238795325112869605, 1.000000000000000000, 0.9238795325112869605, 1.000000000000000000, 0.9238795325112869605, 1.000000000000000000, 0.9238795325112869605, 1.000000000000000000, 0.9238795325112869605, 1.000000000000000000, 0.9238795325112869605, 1.000000000000000000, 0.9238795325112869605, 1.000000000000000000, 0.9238795325112869605, 1.000000000000000000, 0.9238795325112869605, 1.000000000000000000, 0.9238795325112869605, 1.000000000000000000, 0.9238795325112869605, 1.000000000000000000, 0.9238795325112869605, 1.000000000000000000, 0.9238795325112869605, 1.000000000000000000, 0.9238795325112869605, 1.000000000000000000, 0.9238795325112869605, 1.000000000000000000, 0.9238795325112869605, 1.000000000000000000, 0.9238795325112869605, 1.000000000000000000, 0.9238795325112869605, 1.000000000000000000, 0.9238795325112869605, 1.000000000000000000, 0.9238795325112869605, 1.000000000000000000, 0.9238795325112869605, 1.000000000000000000, 0.9238795325112869605, 1.000000000000000000, 0.9238795325112869605, 1.000000000000000000, 0.9238795325112869605, 1.000000000000000000, 0.9238795325112869605, 1.000000000000000000, 0.9238795325112869605, 1.000000000000000000, 0.9238795325112869605, 1.000000000000000000),
 ( 1.000000000000000000, 0.9238795325112869605, 1.000000000000000000, 0.9238795325112869605, 1.000000000000000000, 0.9238795325112869605, 1.000000000000000000, 0.9238795325112869605, 1.000000000000000000, 0.9238795325112869605, 1.000000000000000000, 0.9238795325112869605, 1.000000000000000000, 0.9238795325112869605, 1.000000000000000000, 0.9238795325112869605, 1.000000000000000000, 0.9238795325112869605, 1.000000000000000000, 0.9238795325112869605, 1.000000000000000000, 0.9238795325112869605, 1.000000000000000000, 0.9238795325112869605, 1.000000000000000000, 0.9238795325112869605, 1.000000000000000000, 0.9238795325112869605, 1.000000000000000000, 0.9238795325112869605, 1.000000000000000000, 0.9238795325112869605, 1.000000000000000000, 0.9238795325112869605, 1.000000000000000000, 0.9238795325112869605, 1.000000000000000000, 0.9238795325112869605, 1.000000000000000000, 0.9238795325112869605, 1.000000000000000000, 0.9238795325112869605, 1.000000000000000000, 0.9238795325112869605, 1.000000000000000000, 0.9238795325112869605, 1.000000000000000000, 0.9238795325112869605, 1.000000000000000000, 0.9238795325112869605, 1.000000000000000000, 0.9238795325112869605, 1.000000000000000000, 0.9238795325112869605, 1.000000000000000000, 0.9238795325112869605, 1.000000000000000000, 0.9238795325112869605, 1.000000000000000000, 0.9238795325112869605, 1.000000000000000000, 0.9238795325112869605, 1.000000000000000000, 0.9238795325112869605, 1.000000000000000000, 0.9238795325112869605, 1.000000000000000000, 0.9238795325112869605, 1.000000000000000000, 0.9238795325112869605, 1.000000000000000000, 0.9238795325112869605, 1.000000000000000000, 0.9238795325112869605, 1.000000000000000000, 0.9238795325112869605, 1.000000000000000000, 0.9238795325112869605, 1.000000000000000000, 0.9238795325112869605, 1.000000000000000000, 0.9238795325112869605, 1.000000000000000000, 0.9238795325112869605, 1.000000000000000000, 0.9238795325112869605, 1.000000000000000000, 0.9238795325112869605, 1.000000000000000000, 0.9238795325112869605, 1.000000000000000000, 0.9238795325112869605, 1.000000000000000000, 0.9238795325112869605, 1.000000000000000000, 0.9238795325112869605, 1.000000000000000000, 0.9238795325112869605, 1.000000000000000000, 0.9238795325112869605, 1.000000000000000000, 0.9238795325112869605, 1.000000000000000000, 0.9238795325112869605, 1.000000000000000000, 0.9238795325112869605, 1.000000000000000000, 0.9238795325112869605, 1.000000000000000000, 0.9238795325112869605, 1.000000000000000000, 0.9238795325112869605, 1.000000000000000000, 0.9238795325112869605, 1.000000000000000000, 0.9238795325112869605, 1.000000000000000000, 0.9238795325112869605, 1.000000000000000000, 0.9238795325112869605, 1.000000000000000000, 0.9238795325112869605, 1.000000000000000000, 0.9238795325112869605, 1.000000000000000000, 0.9238795325112869605, 1.000000000000000000, 0.9238795325112869605, 1.000000000000000000, 0.9238795325112869605, 1.000000000000000000, 0.9238795325112869605, 1.000000000000000000, 0.9238795325112869605, 1.000000000000000000, 0.9238795325112869605, 1.000000000000000000, 0.9238795325112869605, 1.000000000000000000, 0.9238795325112869605, 1.000000000000000000, 0.9238795325112869605, 1.000000000000000000, 0.9238795325112869605, 1.000000000000000000, 0.9238795325112869605, 1.000000000000000000, 0.9238795325112869605, 1.000000000000000000, 0.9238795325112869605, 1.000000000000000000, 0.9238795325112869605, 1.000000000000000000, 0.9238795325112869605, 1.000000000000000000, 0.9238795325112869605, 1.000000000000000000, 0.9238795325112869605, 1.000000000000000000, 0.9238795325112869605, 1.000000000000000000, 0.9238795325112869605, 1.000000000000000000, 0.9238795325112869605, 1.000000000000000000, 0.9238795325112869605, 1.000000000000000000, 0.9238795325112869605, 1.000000000000000000, 0.9238795325112869605, 1.000000000000000000, 0.9238795325112869605, 1.000000000000000000, 0.9238795325112869605, 1.000000000000000000, 0.9238795325112869605, 1.000000000000000000, 0.9238795325112869605, 1.000000000000000000, 0.9238795325112869605, 1.000000000000000000, 0.9238795325112869605, 1.000000000000000000, 0.9238795325112869605, 1.000000000000000000, 0.9238795325112869605, 1.000000000000000000, 0.9238795325112869605, 1.000000000000000000, 0.9238795325112869605, 1.000000000000000000, 0.9238795325112869605, 1.000000000000000000, 0.9238795325112869605, 1.000000000000000000, 0.9238795325112869605, 1.000000000000000000, 0.9238795325112869605, 1.000000000000000000, 0.9238795325112869605, 1.000000000000000000, 0.9238795325112869605, 1.000000000000000000, 0.9238795325112869605, 1.000000000000000000, 0.9238795325112869605, 1.000000000000000000, 0.9238795325112869605, 1.000000000000000000, 0.9238795325112869605, 1.000000000000000000, 0.9238795325112869605, 1.000000000000000000, 0.9238795325112869605, 1.000000000000000000, 0.9238795325112869605, 1.000000000000000000, 0.9238795325112869605, 1.000000000000000000, 0.9238795325112869605, 1.000000000000000000, 0.9238795325112869605, 1.000000000000000000, 0.9238795325112869605, 1.000000000000000000, 0.9238795325112869605, 1.000000000000000000, 0.9238795325112869605, 1.000000000000000000, 0.9238795325112869605, 1.000000000000000000, 0.9238795325112869605, 1.000000000000000000, 0.9238795325112869605, 1.000000000000000000, 0.9238795325112869605, 1.000000000000000000, 0.9238795325112869605, 1.000000000000000000, 0.9238795325112869605, 1.000000000000000000, 0.9238795325112869605, 1.000000000000000000, 0.9238795325112869605, 1.000000000000000000, 0.9238795325112869605, 1.000000000000000000, 0.9238795325112869605, 1.000000000000000000, 0.9238795325112869605, 1.000000000000000000, 0.9238795325112869605, 1.000000000000000000, 0.9238795325112869605, 1.000000000000000000, 0.9238795325112869605, 1.000000000000000000) ) ) 
 REPRESENTATION_ITEM ( '' )  SURFACE ( )  );
#3654 = CARTESIAN_POINT ( 'NONE',  ( 137.3019930433552815, -1.207271142501472161, -9.674051694548802871 ) ) ;
#3655 = CARTESIAN_POINT ( 'NONE',  ( 123.0637881442452937, -0.4660016031367893996, -10.09054647747474043 ) ) ;
#3656 = CARTESIAN_POINT ( 'NONE',  ( 106.0375671295248310, -10.62599879583958540, -13.39321520033831447 ) ) ;
#3657 = CARTESIAN_POINT ( 'NONE',  ( 120.1707281442453166, -9.565557343593413364, -10.61323700422348004 ) ) ;
#3658 = ORIENTED_EDGE ( 'NONE', *, *, #36456, .F. ) ;
#3659 = ORIENTED_EDGE ( 'NONE', *, *, #18597, .F. ) ;
#3660 = AXIS2_PLACEMENT_3D ( 'NONE', #31392, #26864, #9537 ) ;
#3661 = CARTESIAN_POINT ( 'NONE',  ( 115.5191414775786569, -3.383040157471821630, -19.15922257007629170 ) ) ;
#3662 = CARTESIAN_POINT ( 'NONE',  ( 125.0492214775786266, -3.505236298600246325, -18.68346056562440793 ) ) ;
#3663 = VECTOR ( 'NONE', #42879, 1000.000000000000000 ) ;
#3664 = CARTESIAN_POINT ( 'NONE',  ( 120.7379948109119709, -10.63000616557722466, -14.87417383870573495 ) ) ;
#3665 = FACE_OUTER_BOUND ( 'NONE', #19411, .T. ) ;
#3666 = CARTESIAN_POINT ( 'NONE',  ( 123.1205148109119563, -1.834011780172310813, -8.268836392978581529 ) ) ;
#3667 = FACE_OUTER_BOUND ( 'NONE', #38630, .T. ) ;
#3668 = CARTESIAN_POINT ( 'NONE',  ( 76.56645223742121686, 1.201885453592819397, -10.89321520033831447 ) ) ;
#3669 = CARTESIAN_POINT ( 'NONE',  ( 124.1415948109119540, -6.344957434206665248, -7.627207830600338134 ) ) ;
#3671 = CARTESIAN_POINT ( 'NONE',  ( 123.0637881442452937, -8.899110576539710493, -16.42337572283490132 ) ) ;
#3670 = CARTESIAN_POINT ( 'NONE',  ( 118.1285681442453068, -7.893985811506177619, -18.51759400769804742 ) ) ;
#3672 = CARTESIAN_POINT ( 'NONE',  ( 120.2274548109119934, -9.859900752359374465, -12.68260735090039404 ) ) ;
#3673 = CARTESIAN_POINT ( 'NONE',  ( 71.36400868967236022, -24.42718413923373788, -4.893215200338314474 ) ) ;
#3674 = CARTESIAN_POINT ( 'NONE',  ( 116.8805814775786445, -6.344957434206662583, -7.627207830600332805 ) ) ;
#3675 = ORIENTED_EDGE ( 'NONE', *, *, #30870, .F. ) ;
#3676 = EDGE_CURVE ( 'NONE', #43140, #23633, #26628, .T. ) ;
#3677 = CARTESIAN_POINT ( 'NONE',  ( 125.2088614775786510, -0.2054726073298613620, -16.14774885094370660 ) ) ;
#3678 = CARTESIAN_POINT ( 'NONE',  ( 116.0388171295248014, 0.1403307496149613920, -13.39321520033831447 ) ) ;
#3679 = CARTESIAN_POINT ( 'NONE',  ( 109.3713171295247832, 0.1403307496149613920, -13.39321520033831447 ) ) ;
#3680 = CARTESIAN_POINT ( 'NONE',  ( 112.5661608795247872, -1.325403438956436419, -16.93181055722141792 ) ) ;
#3681 = CARTESIAN_POINT ( 'NONE',  ( 125.2655881442453278, 0.08617673920530924403, -14.09731900820076334 ) ) ;
#3682 = CARTESIAN_POINT ( 'NONE',  ( 125.6732148109119862, -9.859900752359378018, -12.68260735090039759 ) ) ;
#3683 = ORIENTED_EDGE ( 'NONE', *, *, #16133, .F. ) ;
#3684 = CARTESIAN_POINT ( 'NONE',  ( 114.2711548109119803, -0.1624402480850797581, -16.17319339645315424 ) ) ;
#3685 = CARTESIAN_POINT ( 'NONE',  ( 111.0381921295247878, 0.8980012041604618078, -13.39321520033831447 ) ) ;
#3686 = CARTESIAN_POINT ( 'NONE',  ( 66.82415148905926117, -40.21211973637273474, -4.893215200338314474 ) ) ;
#3687 = CARTESIAN_POINT ( 'NONE',  ( 125.1059481442452750, -8.166667518702819706, -8.995218007635861213 ) ) ;
#3688 = CARTESIAN_POINT ( 'NONE',  ( 124.8223148109119762, 0.9020085738987339008, -11.91225656197089222 ) ) ;
#3689 = CARTESIAN_POINT ( 'NONE',  ( 119.2541079359119749, -5.367357518394803684, -18.78171702160297585 ) ) ;
#3690 = CARTESIAN_POINT ( 'NONE',  ( 114.1577014775786552, -6.344957434206662583, -7.627207830600332805 ) ) ;
#3691 = CARTESIAN_POINT ( 'NONE',  ( 114.7192077545248594, -7.250697342233347165, -7.631215200338321125 ) ) ;
#3692 = CARTESIAN_POINT ( 'NONE',  ( 115.0664733795247798, -1.325403438956436419, -9.854619843455211026 ) ) ;
#3693 = VERTEX_POINT ( 'NONE', #40469 ) ;
#3694 = DIRECTION ( 'NONE',  ( 1.000000000000000000, 0.000000000000000000, -0.000000000000000000 ) ) ;
#3695 = AXIS2_PLACEMENT_3D ( 'NONE', #40723, #9712, #26812 ) ;
#3696 = CARTESIAN_POINT ( 'NONE',  ( 115.0086014775786509, -5.574606645277164318, -18.38911715685844683 ) ) ;
#3697 = CARTESIAN_POINT ( 'NONE',  ( 112.9097148109120070, 0.2603800115204892296, -16.42320221600525088 ) ) ;
#3698 = EDGE_CURVE ( 'NONE', #4879, #19315, #6339, .T. ) ;
#3699 = CARTESIAN_POINT ( 'NONE',  ( 115.0664733795247798, -8.938348069036489818, -17.46756447353520159 ) ) ;
#3700 = CARTESIAN_POINT ( 'NONE',  ( 105.7597546295248350, -4.863998795839590272, -18.39754474579285315 ) ) ;
#3701 = VECTOR ( 'NONE', #43009, 1000.000000000000227 ) ;
#3702 = CARTESIAN_POINT ( 'NONE',  ( 121.2485348109119769, -8.899110576539710493, -16.42337572283490132 ) ) ;
#3703 = CARTESIAN_POINT ( 'NONE',  ( 119.7169148109119874, -0.1624402480850797581, -16.17319339645315424 ) ) ;
#3704 = CARTESIAN_POINT ( 'NONE',  ( 113.5337081442453240, -0.8288870151387760510, -10.36305467784173118 ) ) ;
#3705 = EDGE_LOOP ( 'NONE', ( #40200, #22267, #41392, #19038, #4373 ) ) ;
#3706 = CARTESIAN_POINT ( 'NONE',  ( 125.7299414775786346, -10.15424416112533912, -14.75197769757731336 ) ) ;
#3707 = CARTESIAN_POINT ( 'NONE',  ( 114.5547881442453217, -4.153390946401321671, -8.397313243818183892 ) ) ;
#3708 = ORIENTED_EDGE ( 'NONE', *, *, #34863, .F. ) ;
#3709 = CARTESIAN_POINT ( 'NONE',  ( 88.19154317003298615, -15.02898452507898241, -18.64321520033831803 ) ) ;
#3710 = CARTESIAN_POINT ( 'NONE',  ( 112.2883483795247770, -8.402594152722688392, -16.93181055722141792 ) ) ;
#3711 = ORIENTED_EDGE ( 'NONE', *, *, #31833, .T. ) ;
#3712 = CONICAL_SURFACE ( 'NONE', #8797, 2.000000000000000444, 0.9599310885968830309 ) ;
#3713 = CARTESIAN_POINT ( 'NONE',  ( 117.3343948109119737, -6.222761293078241884, -8.102969835052219238 ) ) ;
#3714 = CARTESIAN_POINT ( 'NONE',  ( 112.5693548109119888, 0.4262465694468514643, -12.03445270309931736 ) ) ;
#3715 = CARTESIAN_POINT ( 'NONE',  ( 69.48536631248848039, -66.77523564985355620, -42.98127819198803934 ) ) ;
#3716 = CARTESIAN_POINT ( 'NONE',  ( 123.1466579359119891, -5.444069387712269226, -19.60292469916370450 ) ) ;
#3717 = ORIENTED_EDGE ( 'NONE', *, *, #12759, .T. ) ;
#3718 = DIRECTION ( 'NONE',  ( -0.9908103287288504424, 0.1352586133457951423, 0.000000000000000000 ) ) ;
#3719 = CARTESIAN_POINT ( 'NONE',  ( 125.1589444732310312, -0.6168232227114794908, -7.334077581337427709 ) ) ;
#3720 = CARTESIAN_POINT ( 'NONE',  ( 106.3153796295248412, -4.863998795839590272, -8.388885654883775800 ) ) ;
#3721 = CARTESIAN_POINT ( 'NONE',  ( 117.2014317992446024, -11.08072105495146076, -21.84774360349757316 ) ) ;
#3722 = VECTOR ( 'NONE', #11508, 1000.000000000000000 ) ;
#3723 = CARTESIAN_POINT ( 'NONE',  ( 121.8158014775786171, -4.153390946401325223, -8.397313243818185668 ) ) ;
#3724 = CARTESIAN_POINT ( 'NONE',  ( 119.0361948109119652, -2.084020599724406786, -8.691656652584148546 ) ) ;
#3725 = CYLINDRICAL_SURFACE ( 'NONE', #25045, 1.999999999999999556 ) ;
#3726 = ORIENTED_EDGE ( 'NONE', *, *, #16414, .F. ) ;
#3727 = CARTESIAN_POINT ( 'NONE',  ( 116.8238548109119819, -5.574606645277164318, -18.38911715685844683 ) ) ;
#3728 = CARTESIAN_POINT ( 'NONE',  ( 119.7434548109120129, -2.395764543994020279, -18.34942947847187611 ) ) ;
#3729 = CARTESIAN_POINT ( 'NONE',  ( 112.1260814775786514, -8.862178061932382889, -16.39564131203247399 ) ) ;
#3730 = CARTESIAN_POINT ( 'NONE',  ( 125.6732148109119862, 0.5811942927096110934, -14.16772938898807510 ) ) ;
#3731 = CARTESIAN_POINT ( 'NONE',  ( 116.1998614775786507, -10.63000616557722466, -14.87417383870573495 ) ) ;
#3732 = ORIENTED_EDGE ( 'NONE', *, *, #29013, .F. ) ;
#3733 = CARTESIAN_POINT ( 'NONE',  ( 111.8886348109120092, -3.383040157471821630, -19.15922257007629170 ) ) ;
#3734 = CARTESIAN_POINT ( 'NONE',  ( 109.4154010812577837, -0.01829820670803256055, -12.14321520033831625 ) ) ;
#3735 = CARTESIAN_POINT ( 'NONE',  ( 113.2606921295247702, 0.8980012041604618078, -13.39321520033831447 ) ) ;
#3736 = CARTESIAN_POINT ( 'NONE',  ( 113.4202548109119846, -10.30919188438810075, -12.61870101168855918 ) ) ;
#3737 = CARTESIAN_POINT ( 'NONE',  ( 115.0653281442453277, -6.344957434206662583, -7.627207830600332805 ) ) ;
#3738 = CARTESIAN_POINT ( 'NONE',  ( 122.1561614775786353, -8.899110576539710493, -16.42337572283490132 ) ) ;
#3739 = CARTESIAN_POINT ( 'NONE',  ( 63.28220228970403127, -14.74607418324612418, -17.03279905538827066 ) ) ;
#3740 = CARTESIAN_POINT ( 'NONE',  ( 112.0799890045248475, -9.868328341294098749, -11.32035403202665869 ) ) ;
#3741 = CARTESIAN_POINT ( 'NONE',  ( 111.7327233795247849, -8.938348069036441856, -17.46756447353520869 ) ) ;
#3742 = CARTESIAN_POINT ( 'NONE',  ( 109.2294312348150527, -3.835661836656289569, -18.43199761928219971 ) ) ;
#3743 = AXIS2_PLACEMENT_3D ( 'NONE', #39189, #18456, #14576 ) ;
#3744 = CARTESIAN_POINT ( 'NONE',  ( 115.4624148109119943, -4.153390946401321671, -8.397313243818183892 ) ) ;
#3745 = EDGE_CURVE ( 'NONE', #6998, #44941, #30200, .T. ) ;
#3746 = CARTESIAN_POINT ( 'NONE',  ( 106.2459265045248173, -7.250697342233347165, -19.15521520033831138 ) ) ;
#3747 = CARTESIAN_POINT ( 'NONE',  ( 114.5108483795247878, -8.402594152722688392, -16.93181055722141792 ) ) ;
#3748 = CARTESIAN_POINT ( 'NONE',  ( 111.5938171295247940, -10.62599879583958540, -13.39321520033831447 ) ) ;
#3749 = CARTESIAN_POINT ( 'NONE',  ( 127.4620922277129580, -5.372330455815395922, -7.794320933752800329 ) ) ;
#3750 = CARTESIAN_POINT ( 'NONE',  ( 124.9357681442453014, -1.834011780172310813, -8.268836392978581529 ) ) ;
#3751 = DIRECTION ( 'NONE',  ( 0.9609149988134837450, -0.1028163501681639419, 0.2570431154366518145 ) ) ;
#3752 = CARTESIAN_POINT ( 'NONE',  ( 125.0492214775786266, -6.344957434206665248, -7.627207830600338134 ) ) ;
#3753 = CARTESIAN_POINT ( 'NONE',  ( 114.7816948109119863, 0.5811942927096154232, -14.16772938898807155 ) ) ;
#3754 = VERTEX_POINT ( 'NONE', #36570 ) ;
#3755 = CARTESIAN_POINT ( 'NONE',  ( 114.6682414775786469, -7.894159318335828068, -9.358103419637847864 ) ) ;
#3756 = VECTOR ( 'NONE', #13524, 1000.000000000000000 ) ;
#3757 = DIRECTION ( 'NONE',  ( 0.000000000000000000, 1.000000000000000000, 0.000000000000000000 ) ) ;
#3758 = CARTESIAN_POINT ( 'NONE',  ( 118.5256548109119876, -0.4660016031367893996, -10.09054647747474043 ) ) ;
#3759 = CARTESIAN_POINT ( 'NONE',  ( 114.7249681442453237, -9.565557343593413364, -10.61323700422348004 ) ) ;
#3760 = ORIENTED_EDGE ( 'NONE', *, *, #13500, .T. ) ;
#3761 = CARTESIAN_POINT ( 'NONE',  ( 121.3619881442452879, -5.574606645277164318, -18.38911715685844683 ) ) ;
#3762 = CARTESIAN_POINT ( 'NONE',  ( 117.7314814775786260, -4.089484607189486809, -7.948022111789456723 ) ) ;
#3763 = CARTESIAN_POINT ( 'NONE',  ( 137.0805771145923870, 0.2345801235192398748, -15.18230913089962186 ) ) ;
#3764 = CARTESIAN_POINT ( 'NONE',  ( 107.9822546295247889, -4.863998795839590272, -7.631215200338315796 ) ) ;
#3765 = CARTESIAN_POINT ( 'NONE',  ( 114.6091521015961376, -1.040089454026971172, -17.23633227186634187 ) ) ;
#3766 = CARTESIAN_POINT ( 'NONE',  ( 143.3676850761856940, -50.16718729050181480, 3.106784799661685526 ) ) ;
#3767 = CARTESIAN_POINT ( 'NONE',  ( 116.9417077545247992, -2.791137627527939813, -18.39754474579286025 ) ) ;
#3768 = CARTESIAN_POINT ( 'NONE',  ( 113.1366214775786432, -1.834011780172310813, -8.268836392978581529 ) ) ;
#3769 = CARTESIAN_POINT ( 'NONE',  ( 86.50830818076254047, -21.65036132658698520, -20.89321520033831447 ) ) ;
#3770 = CARTESIAN_POINT ( 'NONE',  ( 113.7038881442453402, -6.222761293078241884, -8.102969835052219238 ) ) ;
#3771 = CARTESIAN_POINT ( 'NONE',  ( 135.3184548109119874, -10.44474571748257041, -15.59668151425567650 ) ) ;
#3772 = CARTESIAN_POINT ( 'NONE',  ( 76.56645223742121686, 1.201885453592819397, -16.39321520033831447 ) ) ;
#3773 = CARTESIAN_POINT ( 'NONE',  ( 114.9970202545248412, 0.1403307496149616695, -11.32035403202665336 ) ) ;
#3774 = CARTESIAN_POINT ( 'NONE',  ( 113.0231681442453180, -10.15424416112533912, -14.75197769757731336 ) ) ;
#3775 = FACE_OUTER_BOUND ( 'NONE', #42003, .T. ) ;
#3777 = CARTESIAN_POINT ( 'NONE',  ( 115.7460481442453357, 0.9020085738987339008, -11.91225656197089222 ) ) ;
#3776 = CARTESIAN_POINT ( 'NONE',  ( 118.9227414775786400, -10.63000616557722466, -14.87417383870573495 ) ) ;
#3778 = CARTESIAN_POINT ( 'NONE',  ( 123.8012348109119642, -9.565557343593413364, -10.61323700422348004 ) ) ;
#3779 = CARTESIAN_POINT ( 'NONE',  ( 118.1285681442453068, -2.084020599724406786, -8.691656652584148546 ) ) ;
#3780 = VERTEX_POINT ( 'NONE', #1467 ) ;
#3781 = CARTESIAN_POINT ( 'NONE',  ( 122.3890647965036464, -8.305800998871424312, -17.19128988610634678 ) ) ;
#3782 = CARTESIAN_POINT ( 'NONE',  ( 124.0281414775786146, -1.834011780172310813, -8.268836392978581529 ) ) ;
#3783 = CARTESIAN_POINT ( 'NONE',  ( 115.8304577545247582, -2.791137627527939813, -18.39754474579286025 ) ) ;
#3784 = CARTESIAN_POINT ( 'NONE',  ( 114.8951481442453115, -8.899110576539710493, -16.42337572283490132 ) ) ;
#3785 = CARTESIAN_POINT ( 'NONE',  ( 112.6828081442453282, -2.084020599724406786, -8.691656652584148546 ) ) ;
#3786 = CARTESIAN_POINT ( 'NONE',  ( 85.35287308025479547, -28.80162431559100611, -9.543249340220466337 ) ) ;
#3787 = CARTESIAN_POINT ( 'NONE',  ( 111.3854577545248645, -7.250697342233347165, -7.631215200338321125 ) ) ;
#3788 = CARTESIAN_POINT ( 'NONE',  ( 118.6391081442452986, -5.574606645277164318, -18.38911715685844683 ) ) ;
#3789 = CARTESIAN_POINT ( 'NONE',  ( 121.0783548109119749, -9.565557343593413364, -10.61323700422348004 ) ) ;
#3790 = CARTESIAN_POINT ( 'NONE',  ( 115.5334957829843887, 0.6362173239733635022, -14.64321520033831447 ) ) ;
#3791 = CARTESIAN_POINT ( 'NONE',  ( 70.89841814381148311, -68.89136543047671069, -37.69090763720760151 ) ) ;
#3792 = CARTESIAN_POINT ( 'NONE',  ( 120.8547048109119686, -7.554583864224885481, -18.48844787311982785 ) ) ;
#3793 = CARTESIAN_POINT ( 'NONE',  ( 108.6767858795247861, -8.402594152722688392, -9.854619843455216355 ) ) ;
#3794 = CARTESIAN_POINT ( 'NONE',  ( 116.5840207075926145, 2.158964875678295314, -20.60257148143831074 ) ) ;
#3795 = CARTESIAN_POINT ( 'NONE',  ( 118.6391081442452986, -4.089484607189486809, -7.948022111789456723 ) ) ;
#3796 = CARTESIAN_POINT ( 'NONE',  ( 115.2922348109119781, -10.63000616557722466, -14.87417383870573495 ) ) ;
#3797 = CARTESIAN_POINT ( 'NONE',  ( 111.9410827545248708, -2.477300249445798297, -19.15521520033831138 ) ) ;
#3798 = CARTESIAN_POINT ( 'NONE',  ( 85.15861813568058380, -25.99489077589524300, -13.39321520033831625 ) ) ;
#3799 = EDGE_LOOP ( 'NONE', ( #29590, #18190, #29958, #27592, #31507 ) ) ;
#3800 = LINE ( 'NONE', #393, #22498 ) ;
#3801 = VECTOR ( 'NONE', #33295, 1000.000000000000000 ) ;
#3802 = EDGE_CURVE ( 'NONE', #44494, #30068, #22226, .T. ) ;
#3803 = CARTESIAN_POINT ( 'NONE',  ( 122.7234281442452755, -5.638512984488999180, -18.83840828888717311 ) ) ;
#3804 = CIRCLE ( 'NONE', #29297, 1.499999999999996225 ) ;
#3805 = CARTESIAN_POINT ( 'NONE',  ( 112.7395348109119766, -5.638512984488999180, -18.83840828888717311 ) ) ;
#3806 = CARTESIAN_POINT ( 'NONE',  ( 121.6456214775786293, 0.4262465694468514643, -12.03445270309931736 ) ) ;
#3807 = FILL_AREA_STYLE_COLOUR ( '', #31518 ) ;
#3808 = CARTESIAN_POINT ( 'NONE',  ( 125.0492214775786266, -6.344957434206665248, -7.627207830600338134 ) ) ;
#3809 = CARTESIAN_POINT ( 'NONE',  ( 120.2274548109119934, 0.5811942927096110934, -14.16772938898807510 ) ) ;
#3810 = ADVANCED_FACE ( 'NONE', ( #12427 ), #22269, .T. ) ;
#3811 = CARTESIAN_POINT ( 'NONE',  ( 109.0935046295247872, -4.863998795839590272, -18.39754474579285315 ) ) ;
#3812 = VECTOR ( 'NONE', #10685, 1000.000000000000000 ) ;
#3813 = CARTESIAN_POINT ( 'NONE',  ( 115.3489614775786407, -0.8288870151387760510, -10.36305467784173118 ) ) ;
#3814 = CARTESIAN_POINT ( 'NONE',  ( 90.33554924625337890, -25.99489077589524300, -13.39321520033831447 ) ) ;
#3815 = ORIENTED_EDGE ( 'NONE', *, *, #9904, .T. ) ;
#3816 = CARTESIAN_POINT ( 'NONE',  ( 122.0427081442452817, 0.5811942927096110934, -14.16772938898807510 ) ) ;
#3817 = CARTESIAN_POINT ( 'NONE',  ( 110.2184548109119788, -3.104384172016180887, -16.98539509221845734 ) ) ;
#3818 = CARTESIAN_POINT ( 'NONE',  ( 116.1998614775786507, -10.63000616557722466, -14.87417383870573495 ) ) ;
#3819 = EDGE_LOOP ( 'NONE', ( #32133, #14848, #36999, #40879, #37690 ) ) ;
#3820 = CARTESIAN_POINT ( 'NONE',  ( 115.4137390045248566, 0.8980012041604421569, -15.77991374673208469 ) ) ;
#3821 = CARTESIAN_POINT ( 'NONE',  ( 124.8790414775786246, -0.4660016031367893996, -10.09054647747474043 ) ) ;
#3822 = CARTESIAN_POINT ( 'NONE',  ( 70.19189222814998175, -51.48119552555760947, -33.79530790927901052 ) ) ;
#3823 = CARTESIAN_POINT ( 'NONE',  ( 114.1009748109119784, -5.574606645277164318, -18.38911715685844683 ) ) ;
#3824 = ADVANCED_FACE ( 'NONE', ( #39562 ), #15612, .F. ) ;
#3825 = DIRECTION ( 'NONE',  ( 0.000000000000000000, 0.4669533266896289669, 0.8842819633428518067 ) ) ;
#3826 = CARTESIAN_POINT ( 'NONE',  ( 121.1350814775786233, -9.859900752359378018, -12.68260735090039759 ) ) ;
#3827 = EDGE_CURVE ( 'NONE', #12347, #30023, #27583, .T. ) ;
#3828 = B_SPLINE_CURVE_WITH_KNOTS ( 'NONE', 3,
 ( #11759, #25669, #39574, #18818, #22237, #36357, #1707, #26112, #11988, #25889, #32709, #39794, #5128, #19045, #15630, #29534, #43450, #40018, #22688, #36586, #5361, #27477, #33841, #41396, #30213, #43901, #9694, #3291, #37032 ),
 .UNSPECIFIED., .F., .F.,
 ( 4, 2, 2, 2, 1, 1, 2, 2, 2, 2, 1, 1, 1, 2, 2, 2, 4 ),
 ( 0.000000000000000000, 0.2500000000000469624, 0.3750000000000684452, 0.4375000000000791589, 0.4687500000000845435, 0.4843750000000872080, 0.4921875000000887623, 0.5000000000000902611, 0.6250000000000713873, 0.6875000000000619504, 0.7187500000000581757, 0.7343750000000563993, 0.7421875000000554001, 0.7460937500000548450, 0.7500000000000544009, 0.8750000000000272005, 1.000000000000000000 ),
 .UNSPECIFIED. ) ;
#3829 = EDGE_CURVE ( 'NONE', #19616, #19203, #30806, .T. ) ;
#3830 = CARTESIAN_POINT ( 'NONE',  ( 75.95778847736514194, -3.256761025687008537, -10.89321520033831447 ) ) ;
#3831 = CARTESIAN_POINT ( 'NONE',  ( 122.4397948109119767, -0.1624402480850797581, -16.17319339645315424 ) ) ;
#3832 = VECTOR ( 'NONE', #13358, 1000.000000000000000 ) ;
#3833 = CARTESIAN_POINT ( 'NONE',  ( 124.3741441133355892, -11.15020770235569358, -8.516513975753223775 ) ) ;
#3834 = CARTESIAN_POINT ( 'NONE',  ( 118.6391081442452986, -5.574606645277164318, -18.38911715685844683 ) ) ;
#3835 = CARTESIAN_POINT ( 'NONE',  ( 120.7852516859119731, -9.665098340737509730, -17.37397104707595474 ) ) ;
#3836 = CARTESIAN_POINT ( 'NONE',  ( 115.8595014775786609, -1.834011780172310813, -8.268836392978581529 ) ) ;
#3837 = CARTESIAN_POINT ( 'NONE',  ( 87.44708369096657918, -21.99489077589588604, -6.893215200338315363 ) ) ;
#3838 = CARTESIAN_POINT ( 'NONE',  ( 119.9438214775786378, -2.084020599724406786, -8.691656652584148546 ) ) ;
#3839 = VERTEX_POINT ( 'NONE', #44570 ) ;
#3840 = CARTESIAN_POINT ( 'NONE',  ( 118.1285681442453068, -7.893985811506177619, -18.51759400769804742 ) ) ;
#3841 = CARTESIAN_POINT ( 'NONE',  ( 105.7597546295248350, -4.863998795839590272, -7.631215200338315796 ) ) ;
#3842 = CARTESIAN_POINT ( 'NONE',  ( 119.7434548109119703, -1.575707845324203493, -20.23615509330177531 ) ) ;
#3843 = CIRCLE ( 'NONE', #32231, 2.000000000000000444 ) ;
#3844 = FACE_OUTER_BOUND ( 'NONE', #11522, .T. ) ;
#3845 = CARTESIAN_POINT ( 'NONE',  ( 121.4551560953690483, -6.001247023715324147, -18.26661038929047010 ) ) ;
#3846 = CARTESIAN_POINT ( 'NONE',  ( 122.2128881442453263, -1.834011780172310813, -8.268836392978581529 ) ) ;
#3847 = VERTEX_POINT ( 'NONE', #37482 ) ;
#3848 = CARTESIAN_POINT ( 'NONE',  ( 126.5041214912228327, -8.436341138087987801, -9.693603847840460475 ) ) ;
#3849 = CARTESIAN_POINT ( 'NONE',  ( 118.6391081442452986, -5.574606645277164318, -18.38911715685844683 ) ) ;
#3850 = CYLINDRICAL_SURFACE ( 'NONE', #2371, 20.00000000000000355 ) ;
#3851 = FACE_OUTER_BOUND ( 'NONE', #298, .T. ) ;
#3852 = DIRECTION ( 'NONE',  ( -0.9705985873829334754, -0.08939452397200675637, 0.2234882575306194330 ) ) ;
#3853 = CARTESIAN_POINT ( 'NONE',  ( 114.2330358795247776, -8.402594152722688392, -9.854619843455216355 ) ) ;
#3854 = PLANE ( 'NONE',  #8272 ) ;
#3855 = ADVANCED_FACE ( 'NONE', ( #37245 ), #36081, .T. ) ;
#3856 = ORIENTED_EDGE ( 'NONE', *, *, #4513, .T. ) ;
#3857 = CARTESIAN_POINT ( 'NONE',  ( 113.9875214775786532, -0.4660016031367893996, -10.09054647747474043 ) ) ;
#3858 = CARTESIAN_POINT ( 'NONE',  ( 112.7962614775786676, -3.383040157471821630, -19.15922257007629170 ) ) ;
#3859 = CARTESIAN_POINT ( 'NONE',  ( 124.8790414775786246, -0.4660016031367893996, -10.09054647747474043 ) ) ;
#3860 = CARTESIAN_POINT ( 'NONE',  ( 115.6325948109119821, -9.565557343593413364, -10.61323700422348004 ) ) ;
#3861 = CARTESIAN_POINT ( 'NONE',  ( 126.4915402333600696, -3.531116461040918697, -8.432618951126483964 ) ) ;
#3862 = CARTESIAN_POINT ( 'NONE',  ( 117.3343948109119737, -3.383040157471821630, -19.15922257007629170 ) ) ;
#3863 = CARTESIAN_POINT ( 'NONE',  ( 111.6155414775786596, 0.3778260857407392814, -12.04688916545883792 ) ) ;
#3864 = CARTESIAN_POINT ( 'NONE',  ( 123.2184548109119788, -4.863998795839242995, -13.39321520033831447 ) ) ;
#3865 = FACE_OUTER_BOUND ( 'NONE', #18802, .T. ) ;
#3866 = CARTESIAN_POINT ( 'NONE',  ( 123.3474214775786209, -0.1624402480850797581, -16.17319339645315424 ) ) ;
#3867 = ORIENTED_EDGE ( 'NONE', *, *, #13949, .T. ) ;
#3868 = AXIS2_PLACEMENT_3D ( 'NONE', #37031, #2608, #12668 ) ;
#3869 = EDGE_CURVE ( 'NONE', #12923, #2818, #28104, .T. ) ;
#3870 = CARTESIAN_POINT ( 'NONE',  ( 89.40092984481313465, -25.38011337280982715, -14.88121679464376257 ) ) ;
#3871 = AXIS2_PLACEMENT_3D ( 'NONE', #2838, #11209, #18039 ) ;
#3872 = CARTESIAN_POINT ( 'NONE',  ( 117.6180281442453150, -0.4660016031367893996, -10.09054647747474043 ) ) ;
#3873 = CARTESIAN_POINT ( 'NONE',  ( 136.7082020370466751, -8.466464675110531246, -17.74021297388502560 ) ) ;
#3874 = ORIENTED_EDGE ( 'NONE', *, *, #20558, .T. ) ;
#3875 = CARTESIAN_POINT ( 'NONE',  ( 136.1332990479133684, 0.5890802737549483137, -11.18462521611371940 ) ) ;
#3876 = CARTESIAN_POINT ( 'NONE',  ( 121.5888948109119809, -10.30919188438810075, -12.61870101168855918 ) ) ;
#3877 = CARTESIAN_POINT ( 'NONE',  ( 106.3848327545248651, -2.477300249445798297, -19.15521520033831138 ) ) ;
#3878 = CARTESIAN_POINT ( 'NONE',  ( 119.7736414775786358, 0.1319031606808879209, -14.10382304977623669 ) ) ;
#3879 = AXIS2_PLACEMENT_3D ( 'NONE', #40112, #8876, #29850 ) ;
#3880 = ORIENTED_EDGE ( 'NONE', *, *, #22278, .F. ) ;
#3881 = CARTESIAN_POINT ( 'NONE',  ( 116.0864081442453113, -9.988377603198976828, -10.36322818467138340 ) ) ;
#3882 = B_SPLINE_CURVE_WITH_KNOTS ( 'NONE', 3,
 ( #8003, #21912, #4801, #8909, #32614, #8460, #1159, #4575, #2054, #1380, #32390, #43341, #43113, #5026, #22363, #18941, #11656, #5470, #11883, #33279, #18500, #32831, #22584, #8233, #28987, #33049, #26014, #39919, #8680, #43566 ),
 .UNSPECIFIED., .F., .F.,
 ( 4, 2, 2, 1, 2, 2, 2, 1, 1, 2, 2, 2, 1, 1, 1, 2, 2, 4 ),
 ( 0.000000000000000000, 0.03124999999998964717, 0.06249999999997929434, 0.09374999999996894151, 0.1093749999999579364, 0.1249999999999469313, 0.1874999999999130695, 0.2187499999998872013, 0.2343749999998742672, 0.2421874999998592792, 0.2499999999998443190, 0.3749999999997088995, 0.4374999999996524447, 0.4687499999996350142, 0.4843749999996257993, 0.4921874999996208033, 0.4999999999996157518, 1.000000000000000000 ),
 .UNSPECIFIED. ) ;
#3883 = CARTESIAN_POINT ( 'NONE',  ( 116.4642898793805443, -2.191907684172563986, -18.20049396185734025 ) ) ;
#3884 = CARTESIAN_POINT ( 'NONE',  ( 112.8330431242421810, -1.016270020561755860, -17.26805140881366896 ) ) ;
#3885 = EDGE_CURVE ( 'NONE', #35058, #35857, #34500, .T. ) ;
#3886 = DIRECTION ( 'NONE',  ( -0.6049664196031392382, 0.7962509850245451659, 0.000000000000000000 ) ) ;
#3887 = CARTESIAN_POINT ( 'NONE',  ( 124.1415948109119540, -6.344957434206665248, -7.627207830600338134 ) ) ;
#3888 = CARTESIAN_POINT ( 'NONE',  ( 122.8300460087703954, -6.176492496456559955, -18.59847741292036716 ) ) ;
#3889 = CARTESIAN_POINT ( 'NONE',  ( 78.69189222814998175, -46.76310523276723785, -4.893215200338314474 ) ) ;
#3890 = CARTESIAN_POINT ( 'NONE',  ( 124.0281414775786146, -1.834011780172310813, -8.268836392978581529 ) ) ;
#3892 = CARTESIAN_POINT ( 'NONE',  ( 122.4397948109119767, -0.1624402480850797581, -16.17319339645315424 ) ) ;
#3891 = CARTESIAN_POINT ( 'NONE',  ( 123.4608748109119745, -10.63000616557722466, -14.87417383870573495 ) ) ;
#3893 = CARTESIAN_POINT ( 'NONE',  ( 119.6601881442453106, -1.833838273342659253, -17.42832698103878286 ) ) ;
#3894 = CARTESIAN_POINT ( 'NONE',  ( 96.46827370896536991, -26.99359428275991846, -13.24861209478998170 ) ) ;
#3895 = CARTESIAN_POINT ( 'NONE',  ( 115.2355081442453155, -10.30919188438810075, -12.61870101168855918 ) ) ;
#3896 = ORIENTED_EDGE ( 'NONE', *, *, #41842, .T. ) ;
#3897 = MECHANICAL_DESIGN_GEOMETRIC_PRESENTATION_REPRESENTATION (  '', ( #25756 ), #36635 ) ;
#3898 = DIRECTION ( 'NONE',  ( -0.9908103287288504424, 0.1352586133457950590, 0.000000000000000000 ) ) ;
#3899 = CARTESIAN_POINT ( 'NONE',  ( 115.6915515045247531, -6.936859964151250502, -18.39754474579286025 ) ) ;
#3900 = AXIS2_PLACEMENT_3D ( 'NONE', #13422, #23911, #30507 ) ;
#3901 = CARTESIAN_POINT ( 'NONE',  ( 108.7462390045248242, -9.868328341294098749, -11.32035403202665869 ) ) ;
#3902 = CARTESIAN_POINT ( 'NONE',  ( 113.1217858795247935, -8.402594152722688392, -9.854619843455216355 ) ) ;
#3903 = CARTESIAN_POINT ( 'NONE',  ( 70.19189222814998175, -51.12070001563444066, -33.65111096193285078 ) ) ;
#3904 = CARTESIAN_POINT ( 'NONE',  ( 126.4673881442452910, -7.894159318335828068, -9.358103419637847864 ) ) ;
#3905 = ORIENTED_EDGE ( 'NONE', *, *, #20391, .T. ) ;
#3906 = CARTESIAN_POINT ( 'NONE',  ( 114.3846081442453197, 0.4262465694468514643, -12.03445270309931736 ) ) ;
#3907 = CARTESIAN_POINT ( 'NONE',  ( 113.1912390045248031, 0.8980012041604421569, -15.77991374673208469 ) ) ;
#3908 = CARTESIAN_POINT ( 'NONE',  ( 122.3147114802850410, -3.929494816604749641, -18.62311481910883870 ) ) ;
#3909 = CARTESIAN_POINT ( 'NONE',  ( 124.5386814775786206, -5.638512984488999180, -18.83840828888717311 ) ) ;
#3910 = CARTESIAN_POINT ( 'NONE',  ( 123.6877814775786533, -3.383040157471821630, -19.15922257007629170 ) ) ;
#3911 = LINE ( 'NONE', #21701, #37404 ) ;
#3912 = CARTESIAN_POINT ( 'NONE',  ( 116.9940348109119839, -9.988377603198976828, -10.36322818467138340 ) ) ;
#3913 = CARTESIAN_POINT ( 'NONE',  ( 115.8304577545247582, -7.250697342233347165, -7.631215200338321125 ) ) ;
#3914 = CARTESIAN_POINT ( 'NONE',  ( 114.3719421295247827, -9.868328341294093420, -13.39321520033831447 ) ) ;
#3915 = ORIENTED_EDGE ( 'NONE', *, *, #36564, .F. ) ;
#3916 = CONICAL_SURFACE ( 'NONE', #29405, 2.999999999999999556, 0.9599310885968830309 ) ;
#3917 = DIRECTION ( 'NONE',  ( 0.000000000000000000, 0.000000000000000000, -1.000000000000000000 ) ) ;
#3918 = CARTESIAN_POINT ( 'NONE',  ( 117.0507614775786465, 0.1319031606808879209, -14.10382304977623669 ) ) ;
#3919 = CARTESIAN_POINT ( 'NONE',  ( 112.3424481442453384, -6.344957434206662583, -7.627207830600332805 ) ) ;
#3920 = CARTESIAN_POINT ( 'NONE',  ( 114.7886608795247696, -8.938348069036489818, -9.318865927141430916 ) ) ;
#3921 = CARTESIAN_POINT ( 'NONE',  ( 106.3848327545248651, -6.936859964151250502, -8.388885654883777576 ) ) ;
#3922 = CARTESIAN_POINT ( 'NONE',  ( 119.8870948109119752, -0.8288870151387760510, -10.36305467784173118 ) ) ;
#3923 = CARTESIAN_POINT ( 'NONE',  ( 120.9081748109119872, -4.153390946401325223, -8.397313243818185668 ) ) ;
#3924 = CARTESIAN_POINT ( 'NONE',  ( 111.4348214775786801, -3.505236298600246325, -18.68346056562440793 ) ) ;
#3925 = ORIENTED_EDGE ( 'NONE', *, *, #21962, .F. ) ;
#3926 = CARTESIAN_POINT ( 'NONE',  ( 124.7655881442452852, -9.859900752359378018, -12.68260735090039759 ) ) ;
#3927 = DIRECTION ( 'NONE',  ( 0.000000000000000000, -0.3818493186865936084, 0.9242245927363024194 ) ) ;
#3928 = CARTESIAN_POINT ( 'NONE',  ( 112.7395348109119766, -4.153390946401321671, -8.397313243818183892 ) ) ;
#3929 = ORIENTED_EDGE ( 'NONE', *, *, #28917, .F. ) ;
#3930 = LINE ( 'NONE', #294, #34696 ) ;
#3931 = EDGE_CURVE ( 'NONE', #29125, #30068, #23009, .T. ) ;
#3932 = CARTESIAN_POINT ( 'NONE',  ( 112.6260814775786514, -9.261995988541697145, -16.69588392320189030 ) ) ;
#3933 = CLOSED_SHELL ( 'NONE', ( #33804, #43683, #2704, #14896, #35491, #14168, #32857, #17653, #12249, #18716, #14159, #37025, #39249, #42653, #37086, #27839, #42869, #27517, #653, #5131, #368, #39206, #43029, #30592, #5249, #37298, #29906, #24048, #28542, #15585, #31710, #37869, #29228, #36415, #38743, #43433 ) ) ;
#3934 = CARTESIAN_POINT ( 'NONE',  ( 109.9269421295247753, -9.868328341294093420, -13.39321520033831447 ) ) ;
#3935 = ORIENTED_EDGE ( 'NONE', *, *, #28523, .F. ) ;
#3936 = CARTESIAN_POINT ( 'NONE',  ( 118.2420214775786320, -6.222761293078241884, -8.102969835052219238 ) ) ;
#3937 = CARTESIAN_POINT ( 'NONE',  ( 114.8951481442453115, -8.899110576539710493, -16.42337572283490132 ) ) ;
#3938 = CARTESIAN_POINT ( 'NONE',  ( 124.5665232958111091, -9.854882086978124178, -13.73083157374175300 ) ) ;
#3939 = ORIENTED_EDGE ( 'NONE', *, *, #36160, .T. ) ;
#3940 = FACE_OUTER_BOUND ( 'NONE', #7724, .T. ) ;
#3941 = CARTESIAN_POINT ( 'NONE',  ( 125.0660727672592856, -0.4645083225204098554, -7.304893862189946852 ) ) ;
#3942 = CARTESIAN_POINT ( 'NONE',  ( 116.4555358795247884, -0.7896495226426338832, -17.46756447353520159 ) ) ;
#3943 = CARTESIAN_POINT ( 'NONE',  ( 112.8529881442453302, -1.561330072975668060, -17.79121239304076596 ) ) ;
#3944 = CARTESIAN_POINT ( 'NONE',  ( 125.1626748109119802, -0.1624402480850797581, -16.17319339645315424 ) ) ;
#3945 = EDGE_CURVE ( 'NONE', #40078, #35613, #9915, .T. ) ;
#3946 = CARTESIAN_POINT ( 'NONE',  ( 117.0507614775786465, 0.1319031606808879209, -14.10382304977623669 ) ) ;
#3947 = CARTESIAN_POINT ( 'NONE',  ( 113.5337081442453240, -0.8288870151387690566, -10.36305467784174006 ) ) ;
#3948 = ORIENTED_EDGE ( 'NONE', *, *, #26611, .T. ) ;
#3949 = CARTESIAN_POINT ( 'NONE',  ( 116.4267681442453153, -6.222761293078241884, -8.102969835052219238 ) ) ;
#3950 = CIRCLE ( 'NONE', #25093, 0.8999999999999980238 ) ;
#3951 = DIRECTION ( 'NONE',  ( -0.9908103287288505534, 0.1352586133457944206, 0.000000000000000000 ) ) ;
#3952 = CARTESIAN_POINT ( 'NONE',  ( 86.29547825138352835, -26.51858395224443754, -8.393215200338314474 ) ) ;
#3953 = CARTESIAN_POINT ( 'NONE',  ( 115.9693640045247776, -10.62599879583958717, -11.00651665394454604 ) ) ;
#3954 = CARTESIAN_POINT ( 'NONE',  ( 113.5904348109119866, -7.893985811506177619, -18.51759400769804742 ) ) ;
#3955 = ORIENTED_EDGE ( 'NONE', *, *, #34508, .T. ) ;
#3956 = CARTESIAN_POINT ( 'NONE',  ( 117.3911214775786505, -1.561330072975668504, -17.79121239304076951 ) ) ;
#3957 = CARTESIAN_POINT ( 'NONE',  ( 109.7003860982116805, 0.3867979994853637526, -12.14321520033828072 ) ) ;
#3958 = CARTESIAN_POINT ( 'NONE',  ( 109.5796765045248122, -7.250697342233347165, -19.15521520033831138 ) ) ;
#3959 = CARTESIAN_POINT ( 'NONE',  ( 113.3635281442453504, -9.988377603198976828, -10.36322818467138340 ) ) ;
#3960 = CARTESIAN_POINT ( 'NONE',  ( 113.7606148109119886, -1.561330072975668060, -17.79121239304076596 ) ) ;
#3962 = CIRCLE ( 'NONE', #17081, 3.249999999999996003 ) ;
#3961 = CARTESIAN_POINT ( 'NONE',  ( 85.43169907558235820, -25.99489077589524300, -13.39321520033831625 ) ) ;
#3963 = CARTESIAN_POINT ( 'NONE',  ( 111.8716296295247901, -4.863998795839638234, -8.388885654883775800 ) ) ;
#3964 = CARTESIAN_POINT ( 'NONE',  ( 111.3160046295247838, -4.863998795839590272, -18.39754474579285315 ) ) ;
#3965 = ORIENTED_EDGE ( 'NONE', *, *, #19438, .T. ) ;
#3966 = DIRECTION ( 'NONE',  ( -0.8949343913984424415, 0.4123869368673878100, 0.1703803081152053811 ) ) ;
#3967 = CARTESIAN_POINT ( 'NONE',  ( 109.2294391953206798, -4.004300405888451486, -18.47138478117985372 ) ) ;
#3968 = CARTESIAN_POINT ( 'NONE',  ( 115.6893214775786447, -9.859900752359374465, -12.68260735090039404 ) ) ;
#3969 = CARTESIAN_POINT ( 'NONE',  ( 65.03532339491583514, -13.35226529162342501, -11.76448087493823280 ) ) ;
#3970 = FACE_OUTER_BOUND ( 'NONE', #24951, .T. ) ;
#3971 = CARTESIAN_POINT ( 'NONE',  ( 108.9545983795247821, -0.7896495226426338832, -9.318865927141430916 ) ) ;
#3972 = CARTESIAN_POINT ( 'NONE',  ( 126.8137406967953211, -5.033017579089364979, -8.097877628942260486 ) ) ;
#3973 = CARTESIAN_POINT ( 'NONE',  ( 123.9146881442452894, 0.9020085738987339008, -11.91225656197089222 ) ) ;
#3974 = DIRECTION ( 'NONE',  ( 0.9609149988134837450, -0.1028163501681639419, 0.2570431154366518145 ) ) ;
#3975 = CARTESIAN_POINT ( 'NONE',  ( 123.0637881442452937, -0.4660016031367893996, -10.09054647747474043 ) ) ;
#3976 = CARTESIAN_POINT ( 'NONE',  ( 115.8027748109119841, -0.4660016031367893996, -10.09054647747474043 ) ) ;
#3977 = ORIENTED_EDGE ( 'NONE', *, *, #37659, .F. ) ;
#3978 = CARTESIAN_POINT ( 'NONE',  ( 114.8951481442453115, -8.899110576539710493, -16.42337572283490132 ) ) ;
#3979 = CARTESIAN_POINT ( 'NONE',  ( 54.86886719809545809, -45.79521720516596872, -9.393215200338314474 ) ) ;
#3980 = CARTESIAN_POINT ( 'NONE',  ( 118.0718414775786300, -9.261995988541697145, -16.69588392320189030 ) ) ;
#3981 = CARTESIAN_POINT ( 'NONE',  ( 116.7671281442453335, -7.643976991954077427, -18.09477374809248928 ) ) ;
#3982 = VERTEX_POINT ( 'NONE', #6256 ) ;
#3983 = CARTESIAN_POINT ( 'NONE',  ( 121.7590748109119687, -2.084020599724406786, -8.691656652584148546 ) ) ;
#3984 = AXIS2_PLACEMENT_3D ( 'NONE', #3396, #13447, #40811 ) ;
#3985 = CARTESIAN_POINT ( 'NONE',  ( 117.1074881442453233, -10.63000616557722466, -14.87417383870573495 ) ) ;
#3986 = CARTESIAN_POINT ( 'NONE',  ( 137.1434659109582128, 0.4862668849895840917, -13.14961857006992219 ) ) ;
#3987 = CARTESIAN_POINT ( 'NONE',  ( 111.2465515045248168, -2.477300249445798297, -7.631215200338321125 ) ) ;
#3988 = AXIS2_PLACEMENT_3D ( 'NONE', #13113, #37490, #9459 ) ;
#3989 = CARTESIAN_POINT ( 'NONE',  ( 60.45894907855897316, -4.846173528048923096, -17.39321520033831447 ) ) ;
#3990 = DIRECTION ( 'NONE',  ( -1.000000000000000000, 0.000000000000000000, 0.000000000000000000 ) ) ;
#3991 = CARTESIAN_POINT ( 'NONE',  ( 116.5249890045247980, -9.868328341294098749, -11.32035403202665869 ) ) ;
#3992 = CARTESIAN_POINT ( 'NONE',  ( 114.8384214775786489, 0.9020085738987339008, -11.91225656197089222 ) ) ;
#3993 = ADVANCED_FACE ( 'NONE', ( #37715 ), #20176, .F. ) ;
#3994 = DIRECTION ( 'NONE',  ( -0.3445294493088599252, -0.9387755102040817867, 0.000000000000000000 ) ) ;
#3995 = CARTESIAN_POINT ( 'NONE',  ( 121.5582890828414122, -8.372502050422333753, -17.31760344562334808 ) ) ;
#3996 = CARTESIAN_POINT ( 'NONE',  ( 62.56397285973651634, -12.53174821361586488, -16.75792485075395533 ) ) ;
#3997 = CARTESIAN_POINT ( 'NONE',  ( 117.7765781469516924, -3.929494816604741203, -18.62311481910882804 ) ) ;
#3998 = CARTESIAN_POINT ( 'NONE',  ( 116.4555358795247884, -8.402594152722688392, -9.854619843455216355 ) ) ;
#3999 = CARTESIAN_POINT ( 'NONE',  ( 122.1448793335884204, -2.334846009198419559, -18.01015021110789505 ) ) ;
#4000 = CARTESIAN_POINT ( 'NONE',  ( 70.19189222814998175, -52.40967333247598248, -34.16669579553818181 ) ) ;
#4001 = CARTESIAN_POINT ( 'NONE',  ( 67.30914723170953096, -61.38600235115519865, -38.65170400443977883 ) ) ;
#4003 = CARTESIAN_POINT ( 'NONE',  ( 118.4122014775786340, 0.5811942927096110934, -14.16772938898807510 ) ) ;
#4002 = CARTESIAN_POINT ( 'NONE',  ( 89.01247232317646763, -25.99489077589524300, -13.39321520033831447 ) ) ;
#4004 = CARTESIAN_POINT ( 'NONE',  ( 123.2339681442453241, -3.505236298600246325, -18.68346056562440793 ) ) ;
#4005 = CARTESIAN_POINT ( 'NONE',  ( 120.4543614775786295, -5.574606645277164318, -18.38911715685844683 ) ) ;
#4006 = CARTESIAN_POINT ( 'NONE',  ( 125.2194014775786286, -10.30919188438810075, -12.61870101168855918 ) ) ;
#4007 = ORIENTED_EDGE ( 'NONE', *, *, #45112, .T. ) ;
#4008 = CARTESIAN_POINT ( 'NONE',  ( 137.2528433483957713, -8.663841125622667505, -9.754824023745433337 ) ) ;
#4009 = CARTESIAN_POINT ( 'NONE',  ( 124.3685014775786328, -10.63000616557722466, -14.87417383870573495 ) ) ;
#4010 = CARTESIAN_POINT ( 'NONE',  ( 113.7468640045248236, 0.1403307496149616695, -15.46607636864997204 ) ) ;
#4011 = CARTESIAN_POINT ( 'NONE',  ( 117.9016614775786280, -0.1624402480850797581, -16.17319339645315424 ) ) ;
#4012 = CARTESIAN_POINT ( 'NONE',  ( 113.5337081442453240, -0.8288870151387760510, -10.36305467784173118 ) ) ;
#4013 = CARTESIAN_POINT ( 'NONE',  ( 85.18868397526492231, -29.19971465527826737, -9.984222205337539791 ) ) ;
#4014 = CARTESIAN_POINT ( 'NONE',  ( 111.2465515045248168, -2.477300249445798297, -7.631215200338321125 ) ) ;
#4015 = VECTOR ( 'NONE', #28408, 1000.000000000000114 ) ;
#4016 = CARTESIAN_POINT ( 'NONE',  ( 119.4900081442453086, -7.643976991954077427, -18.09477374809248928 ) ) ;
#4017 = CARTESIAN_POINT ( 'NONE',  ( 119.8870948109119752, -0.8288870151387760510, -10.36305467784173118 ) ) ;
#4018 = CARTESIAN_POINT ( 'NONE',  ( 115.6217004682427785, 0.5115630086001619059, -14.64321520033831447 ) ) ;
#4019 = DIRECTION ( 'NONE',  ( 0.9609149988134834119, -0.1028163501681649411, 0.2570431154366530913 ) ) ;
#4020 = CARTESIAN_POINT ( 'NONE',  ( 121.7575954359119805, -11.07370829466463569, -12.81314460846529002 ) ) ;
#4021 = CARTESIAN_POINT ( 'NONE',  ( 110.6909265045248247, -2.791137627527939813, -8.388885654883777576 ) ) ;
#4022 = CARTESIAN_POINT ( 'NONE',  ( 116.8216831185638398, 1.980589080847753092, -20.92910018805106276 ) ) ;
#4023 = CARTESIAN_POINT ( 'NONE',  ( 119.1496481442453046, -3.383040157471821630, -19.15922257007629170 ) ) ;
#4024 = CARTESIAN_POINT ( 'NONE',  ( 116.4834948109119779, -1.561330072975668504, -17.79121239304076951 ) ) ;
#4025 = CARTESIAN_POINT ( 'NONE',  ( 111.6632702545248605, -10.62599879583958717, -15.77991374673208469 ) ) ;
#4026 = CARTESIAN_POINT ( 'NONE',  ( 114.6682414775786469, -1.561330072975668060, -17.79121239304076596 ) ) ;
#4027 = VERTEX_POINT ( 'NONE', #6017 ) ;
#4028 = CARTESIAN_POINT ( 'NONE',  ( 113.0921268052895527, -1.125321370491273454, -17.12283323191015683 ) ) ;
#4029 = CIRCLE ( 'NONE', #25876, 2.999999999999999556 ) ;
#4030 = CARTESIAN_POINT ( 'NONE',  ( 122.8368814775786291, -1.561330072975668948, -17.79121239304076951 ) ) ;
#4031 = CARTESIAN_POINT ( 'NONE',  ( 115.4624148109119943, -5.638512984488999180, -18.83840828888717311 ) ) ;
#4032 = CARTESIAN_POINT ( 'NONE',  ( 120.8514481442452961, -2.084020599724406786, -8.691656652584148546 ) ) ;
#4033 = CARTESIAN_POINT ( 'NONE',  ( 124.7655881442452852, 0.5811942927096110934, -14.16772938898807510 ) ) ;
#4034 = CARTESIAN_POINT ( 'NONE',  ( 123.4041481442452834, -10.30919188438810075, -12.61870101168855918 ) ) ;
#4035 = CARTESIAN_POINT ( 'NONE',  ( 113.8857702545248003, -10.62599879583958717, -15.77991374673208469 ) ) ;
#4036 = CARTESIAN_POINT ( 'NONE',  ( 117.5045748109119756, -9.859900752359374465, -12.68260735090039404 ) ) ;
#4037 = VECTOR ( 'NONE', #12912, 1000.000000000000114 ) ;
#4038 = CARTESIAN_POINT ( 'NONE',  ( 86.09323753712084226, -25.99489077589524300, -13.39321520033831625 ) ) ;
#4039 = ORIENTED_EDGE ( 'NONE', *, *, #43948, .F. ) ;
#4040 =( BOUNDED_CURVE ( )  B_SPLINE_CURVE ( 3, ( #38249, #20941, #10681, #14990 ),
 .UNSPECIFIED., .F., .T. ) 
 B_SPLINE_CURVE_WITH_KNOTS ( ( 4, 4 ),
 ( 4.712388980384689674, 7.853981633974479237 ),
 .UNSPECIFIED. ) 
 CURVE ( )  GEOMETRIC_REPRESENTATION_ITEM ( )  RATIONAL_B_SPLINE_CURVE ( ( 1.000000000000000000, 0.3333333333333335369, 0.3333333333333335369, 1.000000000000000000 ) ) 
 REPRESENTATION_ITEM ( '' )  );
#4041 = CARTESIAN_POINT ( 'NONE',  ( 122.2696148109119889, -4.089484607189486809, -7.948022111789456723 ) ) ;
#4042 = CARTESIAN_POINT ( 'NONE',  ( 119.3267360609119692, -3.387241619883791355, -18.17469012370385073 ) ) ;
#4043 = CARTESIAN_POINT ( 'NONE',  ( 118.0718414775786300, -9.261995988541697145, -16.69588392320189030 ) ) ;
#4044 = VERTEX_POINT ( 'NONE', #6713 ) ;
#4045 = CARTESIAN_POINT ( 'NONE',  ( 115.0664733795247798, -8.938348069036489818, -17.46756447353520159 ) ) ;
#4046 = CARTESIAN_POINT ( 'NONE',  ( 124.8223148109119762, 0.9020085738987339008, -11.91225656197089222 ) ) ;
#4047 = CARTESIAN_POINT ( 'NONE',  ( 93.44708369096697709, -25.99489077589524300, -13.39321520033831447 ) ) ;
#4048 = CARTESIAN_POINT ( 'NONE',  ( 114.7816948109119863, -9.859900752359374465, -12.68260735090039404 ) ) ;
#4049 = CARTESIAN_POINT ( 'NONE',  ( 118.5256548109119876, -8.899110576539710493, -16.42337572283490132 ) ) ;
#4050 = LINE ( 'NONE', #14552, #35258 ) ;
#4051 = CARTESIAN_POINT ( 'NONE',  ( 120.3409081442453044, -8.899110576539710493, -16.42337572283490132 ) ) ;
#4052 = CARTESIAN_POINT ( 'NONE',  ( 124.9801526047702680, -12.03596826789013363, -10.88240524119288288 ) ) ;
#4053 = CARTESIAN_POINT ( 'NONE',  ( 118.8660148109119774, 0.1319031606808879209, -14.10382304977623669 ) ) ;
#4054 = CARTESIAN_POINT ( 'NONE',  ( 112.1155414775786454, 0.9020085738987339008, -11.91225656197089222 ) ) ;
#4055 = CARTESIAN_POINT ( 'NONE',  ( 119.4900081442453086, -1.834011780172310813, -8.268836392978581529 ) ) ;
#4056 = CARTESIAN_POINT ( 'NONE',  ( 112.0588148109119828, 0.5811942927096154232, -14.16772938898807155 ) ) ;
#4057 = DIRECTION ( 'NONE',  ( 1.000000000000000000, 0.000000000000000000, -0.000000000000000000 ) ) ;
#4058 = CARTESIAN_POINT ( 'NONE',  ( 120.6245414775786458, -0.1624402480850797581, -16.17319339645315424 ) ) ;
#4059 = ORIENTED_EDGE ( 'NONE', *, *, #43434, .F. ) ;
#4060 = CARTESIAN_POINT ( 'NONE',  ( 116.9373081442452929, -8.166667518702817929, -8.995218007635861213 ) ) ;
#4061 = CARTESIAN_POINT ( 'NONE',  ( 115.6915515045247531, -6.936859964151250502, -18.39754474579286025 ) ) ;
#4062 = CARTESIAN_POINT ( 'NONE',  ( 115.2355081442453155, 0.1319031606808870605, -14.10382304977625090 ) ) ;
#4063 = DIRECTION ( 'NONE',  ( 0.9609149988134837450, -0.1028163501681639419, 0.2570431154366518145 ) ) ;
#4064 = CARTESIAN_POINT ( 'NONE',  ( 121.8965016859119856, -0.6942167230862464899, -9.935906262978006609 ) ) ;
#4065 = CIRCLE ( 'NONE', #7023, 8.000000000000001776 ) ;
#4066 = CARTESIAN_POINT ( 'NONE',  ( 120.6812681442452941, -10.30919188438810075, -12.61870101168855918 ) ) ;
#4067 = ORIENTED_EDGE ( 'NONE', *, *, #25596, .F. ) ;
#4068 = DIRECTION ( 'NONE',  ( -0.5735764363510446051, 0.3127926500124816878, -0.7570804645221042017 ) ) ;
#4069 = CARTESIAN_POINT ( 'NONE',  ( 120.0005481442453146, -4.153390946401325223, -8.397313243818185668 ) ) ;
#4070 = CARTESIAN_POINT ( 'NONE',  ( 91.11246428952674137, -25.23119213852205789, -15.24166438581092109 ) ) ;
#4071 = DIRECTION ( 'NONE',  ( 0.000000000000000000, 0.8842819633428519177, -0.4669533266896288004 ) ) ;
#4072 = CARTESIAN_POINT ( 'NONE',  ( 120.6343014173871211, -8.493878760966627084, -17.54745775818410536 ) ) ;
#4073 = CARTESIAN_POINT ( 'NONE',  ( 112.4272546295247821, -4.863998795839590272, -18.39754474579285315 ) ) ;
#4074 = CIRCLE ( 'NONE', #2651, 2.000000000000000444 ) ;
#4075 = ORIENTED_EDGE ( 'NONE', *, *, #42977, .F. ) ;
#4076 = CARTESIAN_POINT ( 'NONE',  ( 114.9518748109119883, -1.834011780172310813, -8.268836392978581529 ) ) ;
#4077 = CARTESIAN_POINT ( 'NONE',  ( 126.0703014775786102, -0.1624402480850797581, -16.17319339645315424 ) ) ;
#4078 = CARTESIAN_POINT ( 'NONE',  ( 124.9924948109119924, -4.089484607189486809, -7.948022111789456723 ) ) ;
#4079 = CARTESIAN_POINT ( 'NONE',  ( 120.4543614775786295, -5.574606645277164318, -18.38911715685844683 ) ) ;
#4080 = CARTESIAN_POINT ( 'NONE',  ( 126.4262034846925786, -3.611341894066276481, -8.445358815182457235 ) ) ;
#4081 = CARTESIAN_POINT ( 'NONE',  ( 121.8725281442453223, -3.383040157471821630, -19.15922257007629170 ) ) ;
#4082 = CARTESIAN_POINT ( 'NONE',  ( 112.1155414775786454, -10.15424416112533912, -14.75197769757731336 ) ) ;
#4083 = DIRECTION ( 'NONE',  ( -0.000000000000000000, -0.9284778069183718952, -0.3713878862591649677 ) ) ;
#4084 = CARTESIAN_POINT ( 'NONE',  ( 110.3455291257774888, 0.2334052082820642360, -12.14321520033831625 ) ) ;
#4085 = CARTESIAN_POINT ( 'NONE',  ( 112.1155414775786454, 0.9020085738987339008, -11.91225656197089222 ) ) ;
#4086 = ORIENTED_EDGE ( 'NONE', *, *, #30471, .F. ) ;
#4087 = ADVANCED_FACE ( 'NONE', ( #6931 ), #38263, .T. ) ;
#4088 = AXIS2_PLACEMENT_3D ( 'NONE', #23483, #22400, #18978 ) ;
#4089 = CARTESIAN_POINT ( 'NONE',  ( 115.6915515045247531, -6.936859964151250502, -18.39754474579286025 ) ) ;
#4090 = CARTESIAN_POINT ( 'NONE',  ( 121.5888948109119809, -10.30919188438810075, -12.61870101168855918 ) ) ;
#4091 = ADVANCED_FACE ( 'NONE', ( #17201 ), #10993, .T. ) ;
#4092 = DIRECTION ( 'NONE',  ( -0.9908103287288503314, 0.1352586133457958362, 0.000000000000000000 ) ) ;
#4093 = ORIENTED_EDGE ( 'NONE', *, *, #21558, .F. ) ;
#4094 = CARTESIAN_POINT ( 'NONE',  ( 111.7184548109119788, -9.261995988541697145, -16.69588392320189030 ) ) ;
#4095 = CARTESIAN_POINT ( 'NONE',  ( 122.8936081442453059, 0.2603800115204892296, -16.42320221600525088 ) ) ;
#4096 = CARTESIAN_POINT ( 'NONE',  ( 111.5497331777918788, -0.01829820670803256055, -14.64321520033831447 ) ) ;
#4097 = CARTESIAN_POINT ( 'NONE',  ( 123.4041481442452834, 0.1319031606808879209, -14.10382304977623669 ) ) ;
#4098 = ORIENTED_EDGE ( 'NONE', *, *, #11680, .T. ) ;
#4099 = CARTESIAN_POINT ( 'NONE',  ( 113.7038881442453402, -3.383040157471821630, -19.15922257007629170 ) ) ;
#4100 = AXIS2_PLACEMENT_3D ( 'NONE', #5709, #43809, #32628 ) ;
#4101 = CARTESIAN_POINT ( 'NONE',  ( 117.2294421295248270, 0.5103437856549055684, -4.893215200338311810 ) ) ;
#4102 = CARTESIAN_POINT ( 'NONE',  ( 120.9081748109119872, -5.638512984489026714, -18.83840828888716956 ) ) ;
#4103 = CARTESIAN_POINT ( 'NONE',  ( 136.6675107540880845, -5.407613336693704476, -7.751903229841559551 ) ) ;
#4104 = CARTESIAN_POINT ( 'NONE',  ( 124.7088614775786226, 0.2603800115204892296, -16.42320221600525088 ) ) ;
#4105 = ADVANCED_FACE ( 'NONE', ( #20838 ), #14981, .T. ) ;
#4106 = AXIS2_PLACEMENT_3D ( 'NONE', #9030, #4695, #18615 ) ;
#4107 = CARTESIAN_POINT ( 'NONE',  ( 69.69189222815028018, -41.76310523276638520, -10.39321520033831625 ) ) ;
#4108 = DIRECTION ( 'NONE',  ( -0.000000000000000000, -0.9284778069183721172, -0.3713878862591650232 ) ) ;
#4109 = CARTESIAN_POINT ( 'NONE',  ( 123.2339681442453241, -6.344957434206665248, -7.627207830600338134 ) ) ;
#4111 = CARTESIAN_POINT ( 'NONE',  ( 124.0848681442452772, -5.574606645277164318, -18.38911715685844683 ) ) ;
#4110 = CARTESIAN_POINT ( 'NONE',  ( 121.5321681442453183, -9.988377603198976828, -10.36322818467138340 ) ) ;
#4112 = CARTESIAN_POINT ( 'NONE',  ( 118.7525614775786380, -1.833838273342659253, -17.42832698103878286 ) ) ;
#4113 = CARTESIAN_POINT ( 'NONE',  ( 94.99177781699742695, -22.29799240495002977, -11.86581792559194426 ) ) ;
#4114 = CARTESIAN_POINT ( 'NONE',  ( 118.8660148109119774, -10.30919188438810075, -12.61870101168855918 ) ) ;
#4115 = ADVANCED_FACE ( 'NONE', ( #3501 ), #13551, .T. ) ;
#4116 = ORIENTED_EDGE ( 'NONE', *, *, #27250, .T. ) ;
#4117 = CIRCLE ( 'NONE', #23078, 1.587500000000000355 ) ;
#4118 = ORIENTED_EDGE ( 'NONE', *, *, #37835, .T. ) ;
#4119 = CYLINDRICAL_SURFACE ( 'NONE', #16259, 3.000000000000001776 ) ;
#4120 = EDGE_CURVE ( 'NONE', #19817, #22660, #18631, .T. ) ;
#4121 = DIRECTION ( 'NONE',  ( 0.000000000000000000, 0.9242245927363028635, 0.3818493186865930533 ) ) ;
#4122 = CARTESIAN_POINT ( 'NONE',  ( 112.4272546295247821, -4.863998795839590272, -18.39754474579285315 ) ) ;
#4123 = CARTESIAN_POINT ( 'NONE',  ( 108.1906140045248037, 0.1403307496149616695, -15.46607636864997204 ) ) ;
#4124 = CARTESIAN_POINT ( 'NONE',  ( 114.2330358795247776, -8.402594152722688392, -9.854619843455216355 ) ) ;
#4125 = CARTESIAN_POINT ( 'NONE',  ( 124.1415948109119540, -6.344957434206665248, -7.627207830600338134 ) ) ;
#4126 = CARTESIAN_POINT ( 'NONE',  ( 112.9664414775786412, 0.5811942927096154232, -14.16772938898807155 ) ) ;
#4127 =( BOUNDED_CURVE ( )  B_SPLINE_CURVE ( 2, ( #4096, #32587, #25322, #42424, #35553, #1575, #36234, #39894, #1357, #15269, #43090, #18913, #29403, #11628, #31916, #25764, #28964 ),
 .UNSPECIFIED., .F., .T. ) 
 B_SPLINE_CURVE_WITH_KNOTS ( ( 3, 2, 2, 2, 2, 2, 2, 2, 3 ),
 ( 0.4040431156034944848, 0.4124999999999999778, 0.4249999999999999889, 0.4375000000000000000, 0.4500000000000000111, 0.4625000000000000222, 0.4749999999999999778, 0.4874999999999999889, 0.4959568843965059814 ),
 .UNSPECIFIED. ) 
 CURVE ( )  GEOMETRIC_REPRESENTATION_ITEM ( )  RATIONAL_B_SPLINE_CURVE ( ( 0.9666851417651740608, 0.9485006404992000206, 1.000000000000000000, 0.9238795325112869605, 1.000000000000000000, 0.9238795325112869605, 1.000000000000000000, 0.9238795325112869605, 1.000000000000000000, 0.9238795325112869605, 1.000000000000000000, 0.9238795325112869605, 1.000000000000000000, 0.9238795325112869605, 1.000000000000000000, 0.9485006404991980222, 0.9666851417651760592 ) ) 
 REPRESENTATION_ITEM ( '' )  );
#4128 = ORIENTED_EDGE ( 'NONE', *, *, #1924, .T. ) ;
#4129 = CARTESIAN_POINT ( 'NONE',  ( 113.5904348109119866, -2.084020599724406786, -8.691656652584148546 ) ) ;
#4130 = CARTESIAN_POINT ( 'NONE',  ( 107.8433483795247838, -0.7896495226426338832, -9.318865927141430916 ) ) ;
#4131 = CARTESIAN_POINT ( 'NONE',  ( 119.2063748109119814, -7.894159318335806752, -9.358103419637831877 ) ) ;
#4132 = FACE_OUTER_BOUND ( 'NONE', #40700, .T. ) ;
#4133 = CARTESIAN_POINT ( 'NONE',  ( 124.6521348109119884, -1.561330072975668948, -17.79121239304076951 ) ) ;
#4134 = FACE_OUTER_BOUND ( 'NONE', #28235, .T. ) ;
#4135 = CARTESIAN_POINT ( 'NONE',  ( 117.9016614775786280, -9.988377603198976828, -10.36322818467138340 ) ) ;
#4136 = EDGE_CURVE ( 'NONE', #33593, #9155, #44117, .T. ) ;
#4137 = CARTESIAN_POINT ( 'NONE',  ( 113.7468640045248236, -10.62599879583958717, -11.00651665394454604 ) ) ;
#4138 = CARTESIAN_POINT ( 'NONE',  ( 113.6079577545248043, -2.791137627527939813, -18.39754474579286025 ) ) ;
#4139 = ORIENTED_EDGE ( 'NONE', *, *, #44843, .F. ) ;
#4140 = CARTESIAN_POINT ( 'NONE',  ( 116.2659068881580708, -12.01880880694303855, -6.893215200338315363 ) ) ;
#4141 = CARTESIAN_POINT ( 'NONE',  ( 116.3133148109120043, -2.084020599724406786, -8.691656652584148546 ) ) ;
#4142 = CARTESIAN_POINT ( 'NONE',  ( 125.9568481442452850, -3.505236298600246325, -18.68346056562440793 ) ) ;
#4143 = VECTOR ( 'NONE', #793, 999.9999999999998863 ) ;
#4144 = CARTESIAN_POINT ( 'NONE',  ( 113.2500748109119968, -6.344957434206662583, -7.627207830600332805 ) ) ;
#4145 = EDGE_CURVE ( 'NONE', #13251, #31200, #37560, .T. ) ;
#4146 = CARTESIAN_POINT ( 'NONE',  ( 123.9146881442452894, -10.15424416112533912, -14.75197769757731336 ) ) ;
#4147 = UNCERTAINTY_MEASURE_WITH_UNIT (LENGTH_MEASURE( 1.000000000000000082E-05 ), #7073, 'distance_accuracy_value', 'NONE');
#4148 = CARTESIAN_POINT ( 'NONE',  ( 121.3619881442452879, -5.574606645277164318, -18.38911715685844683 ) ) ;
#4149 = CARTESIAN_POINT ( 'NONE',  ( 117.0507614775786465, 0.1319031606808879209, -14.10382304977623669 ) ) ;
#4150 = ORIENTED_EDGE ( 'NONE', *, *, #29223, .F. ) ;
#4151 = ADVANCED_FACE ( 'NONE', ( #40928 ), #23597, .F. ) ;
#4152 = ADVANCED_FACE ( 'NONE', ( #31760 ), #17638, .F. ) ;
#4153 = CARTESIAN_POINT ( 'NONE',  ( 31.16203868753470019, 11.28474725185576055, -7.393215200338315363 ) ) ;
#4154 = CARTESIAN_POINT ( 'NONE',  ( 121.8367297606643262, -2.236191541394346061, -18.14152338500401029 ) ) ;
#4155 = CARTESIAN_POINT ( 'NONE',  ( 115.1220548109119761, -1.833838273342658809, -17.42832698103878286 ) ) ;
#4156 = ORIENTED_EDGE ( 'NONE', *, *, #3556, .T. ) ;
#4157 = CARTESIAN_POINT ( 'NONE',  ( 126.8396850857591289, -9.603614909541551725, -15.78910935443854768 ) ) ;
#4158 = CARTESIAN_POINT ( 'NONE',  ( 117.2294421295247844, -4.863998795839590272, -19.02821520033831604 ) ) ;
#4159 =( GEOMETRIC_REPRESENTATION_CONTEXT ( 3 ) GLOBAL_UNCERTAINTY_ASSIGNED_CONTEXT ( ( #15884 ) ) GLOBAL_UNIT_ASSIGNED_CONTEXT ( ( #23883, #27067, #41211 ) ) REPRESENTATION_CONTEXT ( 'NONE', 'WORKASPACE' ) );
#4160 = CARTESIAN_POINT ( 'NONE',  ( 111.7327233795247849, -1.325403438956436419, -9.854619843455211026 ) ) ;
#4161 = CARTESIAN_POINT ( 'NONE',  ( 124.9924948109119924, -5.574606645277164318, -18.38911715685844683 ) ) ;
#4162 = VERTEX_POINT ( 'NONE', #4168 ) ;
#4163 = CARTESIAN_POINT ( 'NONE',  ( 117.2209414775786485, -2.084020599724406786, -8.691656652584148546 ) ) ;
#4164 = CARTESIAN_POINT ( 'NONE',  ( 115.6325948109119821, -9.565557343593413364, -10.61323700422348004 ) ) ;
#4165 = CARTESIAN_POINT ( 'NONE',  ( 124.5696098453081788, -9.847885663951533530, -13.82108784073833085 ) ) ;
#4166 = CARTESIAN_POINT ( 'NONE',  ( 122.3132204359119868, 1.345710702986147034, -13.97328579221134426 ) ) ;
#4167 = ORIENTED_EDGE ( 'NONE', *, *, #42868, .F. ) ;
#4168 = CARTESIAN_POINT ( 'NONE',  ( 94.20708369096698220, -25.20837564747665027, -13.06826143013602604 ) ) ;
#4169 = DIRECTION ( 'NONE',  ( 0.8636456077245092677, -0.5040994586965584778, 0.000000000000000000 ) ) ;
#4170 = CARTESIAN_POINT ( 'NONE',  ( 111.6632702545248605, -10.62599879583958717, -15.77991374673208469 ) ) ;
#4171 = CIRCLE ( 'NONE', #18012, 2.999999999999999556 ) ;
#4172 = CARTESIAN_POINT ( 'NONE',  ( 113.4202548109119846, -10.30919188438810075, -12.61870101168855918 ) ) ;
#4173 = CARTESIAN_POINT ( 'NONE',  ( 126.4106614775786284, -6.222761293078241884, -8.102969835052219238 ) ) ;
#4174 = CARTESIAN_POINT ( 'NONE',  ( 116.8238548109119819, -5.574606645277164318, -18.38911715685844683 ) ) ;
#4175 = CARTESIAN_POINT ( 'NONE',  ( 113.4769814775786614, 0.4262465694468579591, -12.03445270309932802 ) ) ;
#4176 = ORIENTED_EDGE ( 'NONE', *, *, #4713, .F. ) ;
#4177 = CARTESIAN_POINT ( 'NONE',  ( 117.7882081442453170, -3.505236298600246325, -18.68346056562440793 ) ) ;
#4178 = CARTESIAN_POINT ( 'NONE',  ( 119.7434548109119845, -1.419520476163944167, -9.663672953983557079 ) ) ;
#4179 = CARTESIAN_POINT ( 'NONE',  ( 85.67997340455728761, -28.00936669380753585, -8.898069645441740505 ) ) ;
#4180 = CARTESIAN_POINT ( 'NONE',  ( 72.54180985774836188, -59.72843766223603268, -36.36500299946500547 ) ) ;
#4181 = CARTESIAN_POINT ( 'NONE',  ( 115.2355081442453155, -10.30919188438810075, -12.61870101168855918 ) ) ;
#4182 = ORIENTED_EDGE ( 'NONE', *, *, #40198, .F. ) ;
#4183 = CARTESIAN_POINT ( 'NONE',  ( 116.1998614775786507, -10.63000616557722466, -14.87417383870573495 ) ) ;
#4184 = DIRECTION ( 'NONE',  ( 0.5735764363510498232, -0.3127926500124802445, 0.7570804645221007600 ) ) ;
#4185 = CARTESIAN_POINT ( 'NONE',  ( 111.4549108795247747, -8.938348069036489818, -9.318865927141430916 ) ) ;
#4186 = CARTESIAN_POINT ( 'NONE',  ( 115.1787814775786387, -9.988377603198976828, -10.36322818467138340 ) ) ;
#4187 = CARTESIAN_POINT ( 'NONE',  ( 113.8173414775786512, 0.2603800115204892296, -16.42320221600525088 ) ) ;
#4188 = AXIS2_PLACEMENT_3D ( 'NONE', #32929, #4675, #43219 ) ;
#4189 = CARTESIAN_POINT ( 'NONE',  ( 61.41189896420279837, -3.923951091603942398, -19.36498282264282977 ) ) ;
#4190 = CARTESIAN_POINT ( 'NONE',  ( 88.28425963449632263, -11.60945497031996787, -8.143215200338314474 ) ) ;
#4191 = CARTESIAN_POINT ( 'NONE',  ( 110.6909265045248247, -2.791137627527939813, -8.388885654883777576 ) ) ;
#4192 = ADVANCED_FACE ( 'NONE', ( #3940 ), #743, .T. ) ;
#4193 = EDGE_LOOP ( 'NONE', ( #148, #21367, #47, #26700 ) ) ;
#4194 = DIRECTION ( 'NONE',  ( -0.000000000000000000, -0.9284778069183721172, -0.3713878862591650232 ) ) ;
#4195 = CARTESIAN_POINT ( 'NONE',  ( 109.2296420770869645, -6.046829405984460948, -18.50501756593391178 ) ) ;
#4196 = CARTESIAN_POINT ( 'NONE',  ( 115.6325948109119821, -9.565557343593413364, -10.61323700422348004 ) ) ;
#4197 = CARTESIAN_POINT ( 'NONE',  ( 122.6009548109119720, -5.853704621469987934, -5.454671103420249523 ) ) ;
#4198 = CARTESIAN_POINT ( 'NONE',  ( 117.9583881442453048, -10.30919188438809719, -12.61870101168856273 ) ) ;
#4199 = CARTESIAN_POINT ( 'NONE',  ( 110.9687390045248350, 0.8980012041604421569, -15.77991374673208469 ) ) ;
#4200 = CARTESIAN_POINT ( 'NONE',  ( 126.6827570900409796, -4.935151780043032232, -8.161448820960071515 ) ) ;
#4201 = CARTESIAN_POINT ( 'NONE',  ( 113.5337081442453240, -0.8288870151387760510, -10.36305467784173118 ) ) ;
#4202 = CARTESIAN_POINT ( 'NONE',  ( 69.36136150295220659, -63.69354577943025930, -35.57539779218904386 ) ) ;
#4203 = CARTESIAN_POINT ( 'NONE',  ( 123.3474214775786209, -9.988377603198976828, -10.36322818467138340 ) ) ;
#4204 = CARTESIAN_POINT ( 'NONE',  ( 116.9940348109119839, -9.988377603198976828, -10.36322818467138340 ) ) ;
#4205 = EDGE_LOOP ( 'NONE', ( #36138, #2910, #18407, #16763 ) ) ;
#4206 = CARTESIAN_POINT ( 'NONE',  ( 116.0296814775786345, -1.833838273342658809, -17.42832698103878286 ) ) ;
#4207 = CARTESIAN_POINT ( 'NONE',  ( 112.5126281442453120, -10.30919188438810075, -12.61870101168855918 ) ) ;
#4208 = EDGE_CURVE ( 'NONE', #42235, #1359, #8513, .T. ) ;
#4209 = CARTESIAN_POINT ( 'NONE',  ( 117.7314814775786260, -4.089484607189486809, -7.948022111789456723 ) ) ;
#4210 = CIRCLE ( 'NONE', #13702, 0.5000000000000004441 ) ;
#4211 = CARTESIAN_POINT ( 'NONE',  ( 118.6958348109119754, -3.505236298600246325, -18.68346056562440793 ) ) ;
#4212 = ORIENTED_EDGE ( 'NONE', *, *, #41209, .F. ) ;
#4213 = EDGE_CURVE ( 'NONE', #42171, #40139, #32205, .T. ) ;
#4214 = CARTESIAN_POINT ( 'NONE',  ( 122.4965214775786251, 0.1319031606808879209, -14.10382304977623669 ) ) ;
#4215 = CARTESIAN_POINT ( 'NONE',  ( 115.3489614775786407, -9.261995988541697145, -16.69588392320189030 ) ) ;
#4216 = CARTESIAN_POINT ( 'NONE',  ( 137.3409837554746105, 0.3147047579545037554, -13.41223745296854730 ) ) ;
#4217 = CARTESIAN_POINT ( 'NONE',  ( 109.0240515045248202, -2.477300249445798297, -7.631215200338321125 ) ) ;
#4218 = FACE_OUTER_BOUND ( 'NONE', #37197, .T. ) ;
#4219 = CARTESIAN_POINT ( 'NONE',  ( 70.19189222814998175, -52.40967333247598248, -34.16669579553818181 ) ) ;
#4220 = CARTESIAN_POINT ( 'NONE',  ( 115.5526452545247622, -9.868328341294098749, -15.46607636864997204 ) ) ;
#4221 = CARTESIAN_POINT ( 'NONE',  ( 114.3846081442453197, -10.63000616557722466, -14.87417383870573495 ) ) ;
#4222 = CARTESIAN_POINT ( 'NONE',  ( 136.6675107540953604, -10.50531076633295768, -13.93682974119022866 ) ) ;
#4223 = CARTESIAN_POINT ( 'NONE',  ( 115.9162281442453235, -5.574606645277164318, -18.38911715685844683 ) ) ;
#4224 = LINE ( 'NONE', #25213, #41087 ) ;
#4225 = CARTESIAN_POINT ( 'NONE',  ( 117.2209414775786485, -2.084020599724404121, -8.691656652584155651 ) ) ;
#4226 = CARTESIAN_POINT ( 'NONE',  ( 113.9552233795247815, -1.325403438956436419, -9.854619843455211026 ) ) ;
#4227 = CARTESIAN_POINT ( 'NONE',  ( 115.4624148109119943, -5.638512984488999180, -18.83840828888717311 ) ) ;
#4228 = FACE_OUTER_BOUND ( 'NONE', #43371, .T. ) ;
#4229 = LINE ( 'NONE', #41881, #14315 ) ;
#4231 = CARTESIAN_POINT ( 'NONE',  ( 119.8303681442453126, -10.63000616557722466, -14.87417383870573495 ) ) ;
#4230 = CARTESIAN_POINT ( 'NONE',  ( 62.22094884293999684, -14.48605613577975681, -7.865232863873874436 ) ) ;
#4232 = CONICAL_SURFACE ( 'NONE', #26839, 2.000000000000000444, 0.9599310885968830309 ) ;
#4233 = CARTESIAN_POINT ( 'NONE',  ( 117.5613014775786525, -10.15424416112533912, -14.75197769757731336 ) ) ;
#4234 = CARTESIAN_POINT ( 'NONE',  ( 125.9568481442452850, -6.344957434206665248, -7.627207830600338134 ) ) ;
#4235 = ORIENTED_EDGE ( 'NONE', *, *, #35056, .T. ) ;
#4236 = CYLINDRICAL_SURFACE ( 'NONE', #29693, 8.000000000000000000 ) ;
#4237 = CARTESIAN_POINT ( 'NONE',  ( 123.1772414775786189, -4.089484607189486809, -7.948022111789456723 ) ) ;
#4238 = CARTESIAN_POINT ( 'NONE',  ( 112.4967077545247633, -2.791137627527939813, -18.39754474579286025 ) ) ;
#4239 = CARTESIAN_POINT ( 'NONE',  ( 120.2274548109119934, -9.859900752359374465, -12.68260735090039404 ) ) ;
#4240 = EDGE_CURVE ( 'NONE', #17567, #15954, #18311, .T. ) ;
#4241 = CARTESIAN_POINT ( 'NONE',  ( 116.5402214775786405, -9.565557343593413364, -10.61323700422348004 ) ) ;
#4242 = DIRECTION ( 'NONE',  ( -0.000000000000000000, -0.9284778069183720062, -0.3713878862591650232 ) ) ;
#4243 = CARTESIAN_POINT ( 'NONE',  ( 110.9687390045248350, 0.8980012041604421569, -15.77991374673208469 ) ) ;
#4244 = CARTESIAN_POINT ( 'NONE',  ( 121.6456214775786293, 0.4262465694468514643, -12.03445270309931736 ) ) ;
#4245 = CARTESIAN_POINT ( 'NONE',  ( 125.6732148109119862, -9.859900752359378018, -12.68260735090039759 ) ) ;
#4246 = CARTESIAN_POINT ( 'NONE',  ( 116.1777233795247781, -1.325403438956436419, -9.854619843455244776 ) ) ;
#4247 = CARTESIAN_POINT ( 'NONE',  ( 109.2293038749584753, -2.355862545069713043, -8.536032044935492280 ) ) ;
#4248 = CARTESIAN_POINT ( 'NONE',  ( 122.2437673109119629, -9.289237151508434209, -11.05642687123711276 ) ) ;
#4249 = CARTESIAN_POINT ( 'NONE',  ( 116.0388171295248014, -10.62599879583958540, -13.39321520033831447 ) ) ;
#4250 = CARTESIAN_POINT ( 'NONE',  ( 88.73939138327467901, -25.38011337280982715, -14.88121679464376257 ) ) ;
#4251 = CARTESIAN_POINT ( 'NONE',  ( 117.2776681442452968, -5.638512984488999180, -18.83840828888717311 ) ) ;
#4252 = CARTESIAN_POINT ( 'NONE',  ( 117.6180281442453150, -0.4660016031367893996, -10.09054647747474043 ) ) ;
#4253 = CARTESIAN_POINT ( 'NONE',  ( 110.8992858795247827, -0.7896495226426338832, -17.46756447353520159 ) ) ;
#4254 = CARTESIAN_POINT ( 'NONE',  ( 112.7395348109119766, -5.638512984488999180, -18.83840828888717311 ) ) ;
#4255 = ORIENTED_EDGE ( 'NONE', *, *, #9672, .F. ) ;
#4256 = DIRECTION ( 'NONE',  ( -1.000000000000000000, 0.000000000000000000, 0.000000000000000000 ) ) ;
#4257 = CARTESIAN_POINT ( 'NONE',  ( 117.6747548109119919, -1.834011780172310813, -8.268836392978581529 ) ) ;
#4258 = EDGE_CURVE ( 'NONE', #31347, #23752, #21505, .T. ) ;
#4259 = CARTESIAN_POINT ( 'NONE',  ( 121.5888948109119809, 0.1319031606808879209, -14.10382304977623669 ) ) ;
#4260 =( LENGTH_UNIT ( ) NAMED_UNIT ( * ) SI_UNIT ( .MILLI., .METRE. ) );
#4261 = CARTESIAN_POINT ( 'NONE',  ( 125.2761281442453054, -10.63000616557722466, -14.87417383870573495 ) ) ;
#4262 = CARTESIAN_POINT ( 'NONE',  ( 122.0427081442452817, 0.5811942927096110934, -14.16772938898807510 ) ) ;
#4263 = CARTESIAN_POINT ( 'NONE',  ( 112.1494421295248003, 0.8980012041604618078, -13.39321520033831447 ) ) ;
#4264 = CARTESIAN_POINT ( 'NONE',  ( 117.5613014775786525, -10.15424416112533912, -14.75197769757731336 ) ) ;
#4265 = CARTESIAN_POINT ( 'NONE',  ( 122.2437673109119629, 0.2312338769422704887, -16.08380026872395874 ) ) ;
#4266 = CARTESIAN_POINT ( 'NONE',  ( 123.6805967241997877, -5.999335727763315695, -18.26299091719257461 ) ) ;
#4267 = ORIENTED_EDGE ( 'NONE', *, *, #38622, .F. ) ;
#4268 = CARTESIAN_POINT ( 'NONE',  ( 121.5321681442453183, -9.988377603198976828, -10.36322818467138340 ) ) ;
#4269 = CARTESIAN_POINT ( 'NONE',  ( 123.2161110609119561, -3.163656168406935087, -18.89861972220014508 ) ) ;
#4270 = CARTESIAN_POINT ( 'NONE',  ( 120.1707281442453166, 0.2603800115204892296, -16.42320221600525088 ) ) ;
#4271 = ORIENTED_EDGE ( 'NONE', *, *, #16277, .T. ) ;
#4272 = CARTESIAN_POINT ( 'NONE',  ( 125.4463081442452932, -4.153390946401325223, -8.397313243818185668 ) ) ;
#4273 = CARTESIAN_POINT ( 'NONE',  ( -13.35201667389344315, -5.063733019641336597, -8.593215170849799023 ) ) ;
#4274 = ADVANCED_FACE ( 'NONE', ( #7143 ), #44904, .T. ) ;
#4275 = DIRECTION ( 'NONE',  ( -0.000000000000000000, -0.9284778069183721172, -0.3713878862591650232 ) ) ;
#4276 = CARTESIAN_POINT ( 'NONE',  ( 114.8951481442453115, -8.899110576539710493, -16.42337572283490132 ) ) ;
#4277 = CARTESIAN_POINT ( 'NONE',  ( 66.38809756183205479, -36.79083284667497367, -4.893215200338314474 ) ) ;
#4278 = CARTESIAN_POINT ( 'NONE',  ( 123.8427358961590130, -2.263366209404226392, -18.10533625161308180 ) ) ;
#4279 = CARTESIAN_POINT ( 'NONE',  ( 119.4900081442453086, -7.643976991954077427, -18.09477374809248928 ) ) ;
#4280 = PLANE ( 'NONE',  #38204 ) ;
#4281 = CARTESIAN_POINT ( 'NONE',  ( 121.1918081442452859, -10.15424416112533912, -14.75197769757731336 ) ) ;
#4282 = CARTESIAN_POINT ( 'NONE',  ( 124.9774582099991846, -10.98257783126069853, -8.877266956160429601 ) ) ;
#4283 = CARTESIAN_POINT ( 'NONE',  ( 119.7736414775786358, 0.1319031606808879209, -14.10382304977623669 ) ) ;
#4284 = CARTESIAN_POINT ( 'NONE',  ( 114.5547881442453217, -5.638512984488999180, -18.83840828888717311 ) ) ;
#4285 = CARTESIAN_POINT ( 'NONE',  ( 120.2841814775786276, 0.9020085738987339008, -11.91225656197089222 ) ) ;
#4286 = CARTESIAN_POINT ( 'NONE',  ( 113.3635281442453504, -9.988377603198976828, -10.36322818467138340 ) ) ;
#4287 = CARTESIAN_POINT ( 'NONE',  ( 70.19189222814998175, -58.54852247098141049, -36.62221405200617141 ) ) ;
#4288 = CARTESIAN_POINT ( 'NONE',  ( 118.7525614775786380, -1.833838273342659253, -17.42832698103878286 ) ) ;
#4289 = ORIENTED_EDGE ( 'NONE', *, *, #1356, .F. ) ;
#4290 = CARTESIAN_POINT ( 'NONE',  ( 119.5467348109119712, -4.089484607189486809, -7.948022111789456723 ) ) ;
#4291 = CARTESIAN_POINT ( 'NONE',  ( 112.7745202545247878, 0.1403307496149616695, -11.32035403202665336 ) ) ;
#4292 = DIRECTION ( 'NONE',  ( -1.000000000000000000, 0.000000000000000000, 0.000000000000000000 ) ) ;
#4293 = CARTESIAN_POINT ( 'NONE',  ( 113.8604010812576774, -0.01829820670803256055, -12.14321520033831625 ) ) ;
#4294 = LINE ( 'NONE', #22312, #24049 ) ;
#4295 = CARTESIAN_POINT ( 'NONE',  ( 125.7866681442452688, -0.4660016031367893996, -10.09054647747474043 ) ) ;
#4296 = ORIENTED_EDGE ( 'NONE', *, *, #7655, .F. ) ;
#4297 = CARTESIAN_POINT ( 'NONE',  ( 75.95778847736514194, -3.256761025687008537, -15.89321520033831447 ) ) ;
#4298 = AXIS2_PLACEMENT_3D ( 'NONE', #44140, #45035, #6036 ) ;
#4299 = CARTESIAN_POINT ( 'NONE',  ( 122.1561614775786353, -8.899110576539710493, -16.42337572283490132 ) ) ;
#4300 = CARTESIAN_POINT ( 'NONE',  ( 121.3408766859119794, -0.06289925094097943703, -9.412459353600674206 ) ) ;
#4301 = CARTESIAN_POINT ( 'NONE',  ( 62.73786426684350204, -14.56780133514543607, -18.73718775869126318 ) ) ;
#4302 = CARTESIAN_POINT ( 'NONE',  ( 120.7251408503701384, -8.552676153439012552, -17.65880394779906837 ) ) ;
#4303 = CARTESIAN_POINT ( 'NONE',  ( 110.2047546295247855, -4.863998795839590272, -18.39754474579285315 ) ) ;
#4304 = EDGE_LOOP ( 'NONE', ( #26211, #21951, #33680 ) ) ;
#4305 = CARTESIAN_POINT ( 'NONE',  ( 114.7816948109119863, 0.5811942927096154232, -14.16772938898807155 ) ) ;
#4306 = CARTESIAN_POINT ( 'NONE',  ( 113.1366214775786432, -1.834011780172310813, -8.268836392978581529 ) ) ;
#4307 = CARTESIAN_POINT ( 'NONE',  ( 88.75490232214124831, -11.10765887499229088, -14.11402746727662638 ) ) ;
#4308 = CARTESIAN_POINT ( 'NONE',  ( 121.0216281442452981, -7.894159318335828068, -9.358103419637847864 ) ) ;
#4309 = EDGE_CURVE ( 'NONE', #1665, #10336, #14441, .T. ) ;
#4310 = CARTESIAN_POINT ( 'NONE',  ( 126.2333338125921074, -4.013644120520951653, -8.458427223423711894 ) ) ;
#4311 = DIRECTION ( 'NONE',  ( 0.9609149988134843001, -0.1028163501681632064, 0.2570431154366505933 ) ) ;
#4312 = CARTESIAN_POINT ( 'NONE',  ( 122.4397948109119767, -9.988377603198976828, -10.36322818467138340 ) ) ;
#4313 = CARTESIAN_POINT ( 'NONE',  ( 123.5176014775786228, -0.8288870151387499607, -10.36305467784176493 ) ) ;
#4314 =( BOUNDED_CURVE ( )  B_SPLINE_CURVE ( 2, ( #28140, #24704, #42268, #4175, #3947, #3285, #27919, #42049, #31100, #20630, #17424, #31316, #24489, #38377, #17207, #38594, #7371 ),
 .UNSPECIFIED., .F., .F. ) 
 B_SPLINE_CURVE_WITH_KNOTS ( ( 3, 2, 2, 2, 2, 2, 2, 2, 3 ),
 ( 0.1421282416568590001, 0.1484375000000000000, 0.1562500000000000000, 0.1640625000000000000, 0.1718750000000000000, 0.1796875000000000000, 0.1875000000000000000, 0.1953125000000000000, 0.2016217583431409999 ),
 .UNSPECIFIED. ) 
 CURVE ( )  GEOMETRIC_REPRESENTATION_ITEM ( )  RATIONAL_B_SPLINE_CURVE ( ( 0.9763430640195970289, 0.9385262470928680267, 1.000000000000000000, 0.9238795325112869605, 1.000000000000000000, 0.9238795325112869605, 1.000000000000000000, 0.9238795325112869605, 1.000000000000000000, 0.9238795325112869605, 1.000000000000000000, 0.9238795325112869605, 1.000000000000000000, 0.9238795325112869605, 1.000000000000000000, 0.9385262470928680267, 0.9763430640195970289 ) ) 
 REPRESENTATION_ITEM ( '' )  );
#4315 = DIRECTION ( 'NONE',  ( -0.9908103287288504424, 0.1352586133457950590, 0.000000000000000000 ) ) ;
#4316 = CARTESIAN_POINT ( 'NONE',  ( 110.0616521944299819, 0.6269505268395592079, -12.14321520033828428 ) ) ;
#4317 = FILL_AREA_STYLE_COLOUR ( '', #28652 ) ;
#4318 = VERTEX_POINT ( 'NONE', #7364 ) ;
#4319 = DIRECTION ( 'NONE',  ( -1.000000000000000000, 0.000000000000000000, -0.000000000000000000 ) ) ;
#4320 = CARTESIAN_POINT ( 'NONE',  ( 120.8514481442452961, -7.893985811506177619, -18.51759400769804742 ) ) ;
#4321 = CARTESIAN_POINT ( 'NONE',  ( 136.2632467228247037, -10.27097813662025416, -15.60566243075115977 ) ) ;
#4322 = VERTEX_POINT ( 'NONE', #38822 ) ;
#4323 = DIRECTION ( 'NONE',  ( 0.000000000000000000, -1.000000000000000000, 1.195183497228115774E-16 ) ) ;
#4324 = CARTESIAN_POINT ( 'NONE',  ( 112.1155414775786454, -10.15424416112533912, -14.75197769757731336 ) ) ;
#4325 = CARTESIAN_POINT ( 'NONE',  ( 66.69189222814998175, -41.76310523276723785, -24.89321520033831447 ) ) ;
#4326 = CARTESIAN_POINT ( 'NONE',  ( 124.5954081442453116, -6.222761293078241884, -8.102969835052219238 ) ) ;
#4327 = ORIENTED_EDGE ( 'NONE', *, *, #25222, .T. ) ;
#4328 = CARTESIAN_POINT ( 'NONE',  ( 119.8870948109119752, -9.261995988541697145, -16.69588392320189030 ) ) ;
#4329 = AXIS2_PLACEMENT_3D ( 'NONE', #27418, #40644, #20352 ) ;
#4330 = DIRECTION ( 'NONE',  ( 0.000000000000000000, 0.000000000000000000, -1.000000000000000000 ) ) ;
#4331 = CIRCLE ( 'NONE', #41413, 2.999999999999999556 ) ;
#4332 = CARTESIAN_POINT ( 'NONE',  ( 79.45722259695331502, 5.067161157875061939, -20.39651227415351542 ) ) ;
#4333 = CARTESIAN_POINT ( 'NONE',  ( 73.07463722459043254, -59.42495381848112856, -36.07827564460922787 ) ) ;
#4334 = CARTESIAN_POINT ( 'NONE',  ( 111.4915481442453142, -1.833838273342658365, -17.42832698103878286 ) ) ;
#4335 = LINE ( 'NONE', #35791, #5117 ) ;
#4336 = CARTESIAN_POINT ( 'NONE',  ( 109.3272331777918822, -0.01829820670803256055, -14.64321520033831447 ) ) ;
#4337 = CARTESIAN_POINT ( 'NONE',  ( 125.0492214775786266, -6.344957434206665248, -7.627207830600338134 ) ) ;
#4338 = VECTOR ( 'NONE', #22507, 1000.000000000000000 ) ;
#4340 = CARTESIAN_POINT ( 'NONE',  ( 121.8158014775786171, -4.153390946401325223, -8.397313243818185668 ) ) ;
#4339 = CARTESIAN_POINT ( 'NONE',  ( 121.9292548109119849, -1.561330072975668948, -17.79121239304076951 ) ) ;
#4341 = CARTESIAN_POINT ( 'NONE',  ( 116.6216037019470235, -9.736060787689369889, -14.64821204404636745 ) ) ;
#4342 = CARTESIAN_POINT ( 'NONE',  ( 124.4252281442452812, -0.8288870151387760510, -10.36305467784173118 ) ) ;
#4343 = CARTESIAN_POINT ( 'NONE',  ( 65.22669769703878728, -15.48412439713661648, -16.39321520033832513 ) ) ;
#4344 = CARTESIAN_POINT ( 'NONE',  ( 121.3052614775786111, -1.834011780172310813, -8.268836392978581529 ) ) ;
#4345 = ORIENTED_EDGE ( 'NONE', *, *, #20682, .T. ) ;
#4346 = EDGE_LOOP ( 'NONE', ( #28342, #5057, #32867, #3965 ) ) ;
#4347 = CARTESIAN_POINT ( 'NONE',  ( 122.7443564273309988, -2.236191541394346061, -18.14152338500401029 ) ) ;
#4348 = DIRECTION ( 'NONE',  ( -0.9908103287288503314, 0.1352586133457956419, 0.000000000000000000 ) ) ;
#4349 = CARTESIAN_POINT ( 'NONE',  ( 115.3442858795247759, -8.402594152722688392, -9.854619843455216355 ) ) ;
#4350 = CARTESIAN_POINT ( 'NONE',  ( 112.4967077545247633, -2.791137627527939813, -18.39754474579286025 ) ) ;
#4351 = CARTESIAN_POINT ( 'NONE',  ( 125.1626748109119802, -9.988377603198980381, -10.36322818467138518 ) ) ;
#4352 = CARTESIAN_POINT ( 'NONE',  ( 125.2194014775786286, 0.1319031606808879209, -14.10382304977623669 ) ) ;
#4353 = VERTEX_POINT ( 'NONE', #35621 ) ;
#4354 = CARTESIAN_POINT ( 'NONE',  ( 114.5547881442453217, -4.153390946401321671, -8.397313243818183892 ) ) ;
#4355 = CARTESIAN_POINT ( 'NONE',  ( 105.8292077545248446, -7.250697342233347165, -7.631215200338321125 ) ) ;
#4356 = DIRECTION ( 'NONE',  ( 0.000000000000000000, 0.000000000000000000, -1.000000000000000000 ) ) ;
#4357 = CARTESIAN_POINT ( 'NONE',  ( 125.5597614775786326, -1.561330072975669392, -17.79121239304076951 ) ) ;
#4358 = CARTESIAN_POINT ( 'NONE',  ( 119.7434548109119703, -6.339884145921025116, -18.90789653539788517 ) ) ;
#4359 = CARTESIAN_POINT ( 'NONE',  ( 79.36790013323479798, 5.032986779684683221, -6.252821205110531189 ) ) ;
#4360 = CARTESIAN_POINT ( 'NONE',  ( 115.5758681442453053, -1.561330072975668060, -17.79121239304076951 ) ) ;
#4361 = CARTESIAN_POINT ( 'NONE',  ( 112.8439733795247832, -8.938348069036489818, -17.46756447353520159 ) ) ;
#4362 = CARTESIAN_POINT ( 'NONE',  ( 110.4825671295247815, 0.1403307496149613920, -13.39321520033831447 ) ) ;
#4363 = VERTEX_POINT ( 'NONE', #42261 ) ;
#4364 = CARTESIAN_POINT ( 'NONE',  ( 126.2184548109108420, -7.843366116849215253, -9.377719973493116257 ) ) ;
#4365 = CARTESIAN_POINT ( 'NONE',  ( 120.5678148109119832, -1.833838273342659253, -17.42832698103878286 ) ) ;
#4366 = CARTESIAN_POINT ( 'NONE',  ( 117.7882081442453170, -6.344957434206665248, -7.627207830600338134 ) ) ;
#4367 = CIRCLE ( 'NONE', #41531, 2.000000000000000444 ) ;
#4368 = B_SPLINE_CURVE_WITH_KNOTS ( 'NONE', 3,
 ( #14121, #24611, #45147, #38954, #27597, #6842, #35064, #20749, #41945, #34627 ),
 .UNSPECIFIED., .F., .F.,
 ( 4, 3, 3, 4 ),
 ( 0.000000000000000000, 0.0002476486447138875262, 0.0004952972925464129957, 0.0009604418836934569808 ),
 .UNSPECIFIED. ) ;
#4369 = CARTESIAN_POINT ( 'NONE',  ( 82.38065881859543538, -29.99489077589589314, -11.39321520033831447 ) ) ;
#4370 = CARTESIAN_POINT ( 'NONE',  ( 125.5030348109119558, -6.222761293078241884, -8.102969835052219238 ) ) ;
#4371 = CARTESIAN_POINT ( 'NONE',  ( 118.8092881442453290, -0.1624402480850797581, -16.17319339645315424 ) ) ;
#4372 = CARTESIAN_POINT ( 'NONE',  ( 115.1787814775786387, -0.1624402480850797581, -16.17319339645315424 ) ) ;
#4373 = ORIENTED_EDGE ( 'NONE', *, *, #34780, .T. ) ;
#4374 = ADVANCED_FACE ( 'NONE', ( #18086 ), #31048, .T. ) ;
#4375 = CARTESIAN_POINT ( 'NONE',  ( 120.7852516859119731, -9.665098340737509730, -17.37397104707595474 ) ) ;
#4376 = VECTOR ( 'NONE', #43012, 1000.000000000000114 ) ;
#4377 = CARTESIAN_POINT ( 'NONE',  ( 85.04324155394569118, -25.99489077589524300, -13.39321520033831447 ) ) ;
#4378 = CARTESIAN_POINT ( 'NONE',  ( 118.8092881442453290, -0.1624402480850797581, -16.17319339645315424 ) ) ;
#4379 = ORIENTED_EDGE ( 'NONE', *, *, #34764, .F. ) ;
#4380 =( REPRESENTATION_RELATIONSHIP ('NONE','NONE', #36667, #26250 ) REPRESENTATION_RELATIONSHIP_WITH_TRANSFORMATION ( #37291 )SHAPE_REPRESENTATION_RELATIONSHIP( ) );
#4381 = CIRCLE ( 'NONE', #17532, 2.999999999999999556 ) ;
#4382 = FACE_OUTER_BOUND ( 'NONE', #8454, .T. ) ;
#4383 = CARTESIAN_POINT ( 'NONE',  ( 114.1577014775786552, -6.344957434206662583, -7.627207830600332805 ) ) ;
#4384 = EDGE_CURVE ( 'NONE', #31317, #13043, #12118, .T. ) ;
#4385 = CARTESIAN_POINT ( 'NONE',  ( 106.9404577545248145, -2.791137627527939813, -18.39754474579286025 ) ) ;
#4386 = CARTESIAN_POINT ( 'NONE',  ( 113.8173414775786512, -9.565557343593413364, -10.61323700422348004 ) ) ;
#4387 = VERTEX_POINT ( 'NONE', #11250 ) ;
#4388 = ORIENTED_EDGE ( 'NONE', *, *, #27284, .F. ) ;
#4389 = CARTESIAN_POINT ( 'NONE',  ( 119.4900081442453086, -7.643976991954077427, -18.09477374809248928 ) ) ;
#4390 = CARTESIAN_POINT ( 'NONE',  ( 116.9940348109119839, -0.1624402480850797581, -16.17319339645315424 ) ) ;
#4391 = CARTESIAN_POINT ( 'NONE',  ( 124.5508470055817156, -9.863829598939307886, -13.27840026003464935 ) ) ;
#4392 = CARTESIAN_POINT ( 'NONE',  ( 123.9106423109119675, -9.959231468620755479, -10.70263013195267199 ) ) ;
#4393 = ORIENTED_EDGE ( 'NONE', *, *, #31960, .T. ) ;
#4394 = CARTESIAN_POINT ( 'NONE',  ( 121.1874648073892615, -1.081026697600536046, -17.18181821144402832 ) ) ;
#4395 = CARTESIAN_POINT ( 'NONE',  ( 125.0048763211382408, -2.344029031882285175, -6.249864847596490414 ) ) ;
#4396 = CARTESIAN_POINT ( 'NONE',  ( 110.1353015045248469, -2.477300249445798297, -7.631215200338321125 ) ) ;
#4397 = CIRCLE ( 'NONE', #38627, 2.000000000000000444 ) ;
#4398 =( BOUNDED_CURVE ( )  B_SPLINE_CURVE ( 2, ( #7422, #31375, #21343, #146, #14280, #35227, #593, #14503, #31159, #14060, #45077, #3776, #44864, #6548, #27978, #38436, #41882 ),
 .UNSPECIFIED., .F., .F. ) 
 B_SPLINE_CURVE_WITH_KNOTS ( ( 3, 2, 2, 2, 2, 2, 2, 2, 3 ),
 ( 0.4545046674808919662, 0.4609375000000000000, 0.4687500000000000000, 0.4765625000000000000, 0.4843750000000000000, 0.4921875000000000000, 0.5000000000000000000, 0.5078125000000000000, 0.5142453325190590174 ),
 .UNSPECIFIED. ) 
 CURVE ( )  GEOMETRIC_REPRESENTATION_ITEM ( )  RATIONAL_B_SPLINE_CURVE ( ( 0.9778625265006459788, 0.9373222120152210346, 1.000000000000000000, 0.9238795325112869605, 1.000000000000000000, 0.9238795325112869605, 1.000000000000000000, 0.9238795325112869605, 1.000000000000000000, 0.9238795325112869605, 1.000000000000000000, 0.9238795325112869605, 1.000000000000000000, 0.9238795325112869605, 1.000000000000000000, 0.9373222120157009840, 0.9778625265000250311 ) ) 
 REPRESENTATION_ITEM ( '' )  );
#4399 = CARTESIAN_POINT ( 'NONE',  ( 113.8173414775786512, 0.2603800115204892296, -16.42320221600525088 ) ) ;
#4400 = EDGE_CURVE ( 'NONE', #40778, #37706, #37595, .T. ) ;
#4401 = CARTESIAN_POINT ( 'NONE',  ( 126.1270281442452870, 0.1319031606808879209, -14.10382304977623669 ) ) ;
#4402 = CARTESIAN_POINT ( 'NONE',  ( 117.3343948109119737, -6.222761293078241884, -8.102969835052219238 ) ) ;
#4403 = DIRECTION ( 'NONE',  ( 0.000000000000000000, 0.9284778069183721172, 0.3713878862591650232 ) ) ;
#4404 = EDGE_CURVE ( 'NONE', #38601, #11611, #35139, .T. ) ;
#4405 = EDGE_CURVE ( 'NONE', #18186, #38837, #25230, .T. ) ;
#4406 = ORIENTED_EDGE ( 'NONE', *, *, #27344, .F. ) ;
#4407 = CARTESIAN_POINT ( 'NONE',  ( 118.8660148109119774, 0.1319031606808879209, -14.10382304977623669 ) ) ;
#4408 = CARTESIAN_POINT ( 'NONE',  ( 112.1874712410415924, 0.7607806665037644134, -12.14321520033829493 ) ) ;
#4409 = AXIS2_PLACEMENT_3D ( 'NONE', #10168, #13365, #3086 ) ;
#4410 = DIRECTION ( 'NONE',  ( -0.000000000000000000, -0.9284778069183720062, -0.3713878862591650232 ) ) ;
#4411 = CARTESIAN_POINT ( 'NONE',  ( 116.6536748109119941, 0.9020085738987339008, -11.91225656197089222 ) ) ;
#4412 = VERTEX_POINT ( 'NONE', #29464 ) ;
#4413 = CIRCLE ( 'NONE', #34288, 2.999999999999999556 ) ;
#4414 = CARTESIAN_POINT ( 'NONE',  ( 118.5256548109119876, -0.4660016031367893996, -10.09054647747474043 ) ) ;
#4415 = CARTESIAN_POINT ( 'NONE',  ( 109.8766384760652812, 0.6362173239733635022, -12.14321520033831625 ) ) ;
#4416 = CARTESIAN_POINT ( 'NONE',  ( 111.5938171295247940, -10.62599879583958540, -13.39321520033831447 ) ) ;
#4417 = CARTESIAN_POINT ( 'NONE',  ( 117.2776681442452968, -5.638512984488999180, -18.83840828888717311 ) ) ;
#4418 = CARTESIAN_POINT ( 'NONE',  ( 115.4056881442453459, -7.893985811506177619, -18.51759400769804742 ) ) ;
#4419 = CARTESIAN_POINT ( 'NONE',  ( 72.54180985774836188, -58.79995985531765967, -35.99361511320584128 ) ) ;
#4420 = DIRECTION ( 'NONE',  ( 0.9609149988134837450, -0.1028163501681639419, 0.2570431154366518145 ) ) ;
#4421 = CARTESIAN_POINT ( 'NONE',  ( 106.2459265045248173, -2.791137627527939813, -8.388885654883777576 ) ) ;
#4422 = ORIENTED_EDGE ( 'NONE', *, *, #38977, .T. ) ;
#4423 = CARTESIAN_POINT ( 'NONE',  ( 115.6220983795247861, -0.7896495226426338832, -9.318865927141430916 ) ) ;
#4424 = CARTESIAN_POINT ( 'NONE',  ( 109.2295940650973876, -4.951169889926434031, -18.58642991963417046 ) ) ;
#4425 = CARTESIAN_POINT ( 'NONE',  ( 115.9729548109119861, -3.505236298600246325, -18.68346056562440793 ) ) ;
#4426 = CARTESIAN_POINT ( 'NONE',  ( 63.41431291788855873, -12.69930909095325511, -10.45796961699282690 ) ) ;
#4427 = CARTESIAN_POINT ( 'NONE',  ( 115.9693640045247776, 0.1403307496149616695, -15.46607636864997204 ) ) ;
#4428 = CARTESIAN_POINT ( 'NONE',  ( 115.2053796295247849, -4.863998795839590272, -8.388885654883775800 ) ) ;
#4429 = CARTESIAN_POINT ( 'NONE',  ( 126.3444272079776454, -4.573690577007555547, -8.338462930989205546 ) ) ;
#4430 = CARTESIAN_POINT ( 'NONE',  ( 114.8384214775786489, -10.15424416112533912, -14.75197769757731336 ) ) ;
#4431 = CARTESIAN_POINT ( 'NONE',  ( 135.8113403534200074, 1.048617111794840628, -12.65718902849948435 ) ) ;
#4432 = CARTESIAN_POINT ( 'NONE',  ( 122.2128881442453263, -1.834011780172310813, -8.268836392978581529 ) ) ;
#4433 = CARTESIAN_POINT ( 'NONE',  ( 120.4543614775786295, -4.089484607189486809, -7.948022111789456723 ) ) ;
#4434 = ORIENTED_EDGE ( 'NONE', *, *, #42420, .T. ) ;
#4435 = CARTESIAN_POINT ( 'NONE',  ( 118.3554748109119998, -9.565557343593413364, -10.61323700422348004 ) ) ;
#4436 = CARTESIAN_POINT ( 'NONE',  ( 126.0135748109119902, -8.166667518702819706, -8.995218007635861213 ) ) ;
#4437 = VECTOR ( 'NONE', #14917, 1000.000000000000000 ) ;
#4438 = CARTESIAN_POINT ( 'NONE',  ( 119.4332814775786318, -0.4660016031367893996, -10.09054647747474043 ) ) ;
#4439 = CARTESIAN_POINT ( 'NONE',  ( 118.7525614775786380, -1.833838273342659253, -17.42832698103878286 ) ) ;
#4440 = ORIENTED_EDGE ( 'NONE', *, *, #28510, .F. ) ;
#4441 = CARTESIAN_POINT ( 'NONE',  ( 120.2274548109119934, -9.859900752359378018, -12.68260735090039759 ) ) ;
#4442 = CIRCLE ( 'NONE', #31386, 2.000000000000000444 ) ;
#4443 = CARTESIAN_POINT ( 'NONE',  ( 121.7590748109119687, -7.893985811506177619, -18.51759400769804742 ) ) ;
#4444 = CARTESIAN_POINT ( 'NONE',  ( 135.3184548109119874, 0.6402711692277546218, -15.78131322003127579 ) ) ;
#4445 = CARTESIAN_POINT ( 'NONE',  ( 108.4684265045247997, -7.250697342233347165, -19.15521520033831138 ) ) ;
#4446 = VECTOR ( 'NONE', #37878, 1000.000000000000114 ) ;
#4447 = CARTESIAN_POINT ( 'NONE',  ( 60.45894907855897316, -4.846173528048923096, -9.393215200338314474 ) ) ;
#4448 = DIRECTION ( 'NONE',  ( -1.000000000000000000, 0.000000000000000000, 0.000000000000000000 ) ) ;
#4449 = CARTESIAN_POINT ( 'NONE',  ( 111.7327233795247849, -1.325403438956436419, -9.854619843455211026 ) ) ;
#4450 = CARTESIAN_POINT ( 'NONE',  ( 116.7671281442453335, -1.834011780172310813, -8.268836392978581529 ) ) ;
#4451 = CYLINDRICAL_SURFACE ( 'NONE', #12799, 1.000000000000000888 ) ;
#4452 = CARTESIAN_POINT ( 'NONE',  ( 115.1787814775786387, -0.1624402480850797581, -16.17319339645315424 ) ) ;
#4453 = DIRECTION ( 'NONE',  ( 0.8636456077245080465, -0.5040994586965603652, 0.000000000000000000 ) ) ;
#4454 = EDGE_CURVE ( 'NONE', #16401, #39949, #1169, .T. ) ;
#4455 = DIRECTION ( 'NONE',  ( 0.000000000000000000, 0.000000000000000000, -1.000000000000000000 ) ) ;
#4456 = CARTESIAN_POINT ( 'NONE',  ( 109.7185827545247889, -6.936859964151250502, -8.388885654883777576 ) ) ;
#4457 = CARTESIAN_POINT ( 'NONE',  ( 112.6828081442453282, -2.084020599724406786, -8.691656652584148546 ) ) ;
#4458 = DIRECTION ( 'NONE',  ( 0.000000000000000000, 0.000000000000000000, 1.000000000000000000 ) ) ;
#4459 = CIRCLE ( 'NONE', #41630, 0.8509999999999994236 ) ;
#4460 = PLANE ( 'NONE',  #572 ) ;
#4462 = CARTESIAN_POINT ( 'NONE',  ( 118.6391081442452986, -4.089484607189486809, -7.948022111789456723 ) ) ;
#4461 = CARTESIAN_POINT ( 'NONE',  ( 63.72678816918493538, -14.88173340316315674, -8.505439947836993753 ) ) ;
#4463 = CARTESIAN_POINT ( 'NONE',  ( 119.0361948109119652, -2.084020599724406786, -8.691656652584148546 ) ) ;
#4464 = CARTESIAN_POINT ( 'NONE',  ( 112.5126281442453120, 0.1319031606808879209, -14.10382304977623669 ) ) ;
#4465 = ORIENTED_EDGE ( 'NONE', *, *, #10351, .T. ) ;
#4466 = CARTESIAN_POINT ( 'NONE',  ( 137.4945747550013095, -7.665717176805711297, -9.228124848700741012 ) ) ;
#4467 = EDGE_CURVE ( 'NONE', #12877, #16491, #44160, .T. ) ;
#4468 = CARTESIAN_POINT ( 'NONE',  ( 122.6667014775786413, -7.893985811506177619, -18.51759400769804742 ) ) ;
#4469 = CARTESIAN_POINT ( 'NONE',  ( 114.7192077545248594, -2.791137627527939813, -18.39754474579286025 ) ) ;
#4470 = CARTESIAN_POINT ( 'NONE',  ( 118.1852948109119836, -4.153390946401325223, -8.397313243818185668 ) ) ;
#4471 = CARTESIAN_POINT ( 'NONE',  ( 117.7314814775786260, -5.574606645277164318, -18.38911715685844683 ) ) ;
#4472 = CARTESIAN_POINT ( 'NONE',  ( 86.24197381513980076, -26.64821576645285717, -8.446815953897829132 ) ) ;
#4473 = CARTESIAN_POINT ( 'NONE',  ( 107.7738952545248310, 0.8980012041604421569, -11.00651665394454071 ) ) ;
#4474 = CARTESIAN_POINT ( 'NONE',  ( 122.1561614775786353, -8.899110576539710493, -16.42337572283490132 ) ) ;
#4475 = CARTESIAN_POINT ( 'NONE',  ( 124.5386814775786206, -4.153390946401325223, -8.397313243818185668 ) ) ;
#4476 = CARTESIAN_POINT ( 'NONE',  ( 114.2354127111058659, -1.267766418764742387, -16.93314635290707315 ) ) ;
#4477 = CARTESIAN_POINT ( 'NONE',  ( 109.2293033147500125, -2.564670721265329689, -8.421802055769131101 ) ) ;
#4478 = CARTESIAN_POINT ( 'NONE',  ( 121.7575954359119805, 0.5291689781388270175, -13.89700978578772705 ) ) ;
#4479 = CARTESIAN_POINT ( 'NONE',  ( 106.0375671295248310, 0.1403307496149613920, -13.39321520033831447 ) ) ;
#4480 = DIRECTION ( 'NONE',  ( -0.000000000000000000, -0.9284778069183721172, -0.3713878862591650232 ) ) ;
#4481 = CARTESIAN_POINT ( 'NONE',  ( 83.86221371915534917, -31.76296181758290516, -22.89672297930211187 ) ) ;
#4482 = CARTESIAN_POINT ( 'NONE',  ( 116.4267681442453153, -3.383040157471821630, -19.15922257007629170 ) ) ;
#4483 = CARTESIAN_POINT ( 'NONE',  ( 119.8303681442453126, -10.63000616557722466, -14.87417383870573495 ) ) ;
#4484 = CARTESIAN_POINT ( 'NONE',  ( 111.8716296295247901, -4.863998795839590272, -19.15521520033831493 ) ) ;
#4485 = CARTESIAN_POINT ( 'NONE',  ( 112.6828081442453282, -7.893985811506177619, -18.51759400769804742 ) ) ;
#4486 = VERTEX_POINT ( 'NONE', #20062 ) ;
#4487 = CARTESIAN_POINT ( 'NONE',  ( 117.3711764575755012, -1.016270020561755860, -17.26805140881366896 ) ) ;
#4488 = CARTESIAN_POINT ( 'NONE',  ( 117.3343948109119737, -3.383040157471821630, -19.15922257007629170 ) ) ;
#4489 = CARTESIAN_POINT ( 'NONE',  ( 123.4041481442452834, 0.1319031606808879209, -14.10382304977623669 ) ) ;
#4490 = SHAPE_DEFINITION_REPRESENTATION ( #14670, #30918 ) ;
#4491 = CARTESIAN_POINT ( 'NONE',  ( 124.5386814775786206, -5.638512984488999180, -18.83840828888717311 ) ) ;
#4492 = CARTESIAN_POINT ( 'NONE',  ( 121.7023481442452777, -9.261995988541697145, -16.69588392320189030 ) ) ;
#4493 = B_SPLINE_CURVE_WITH_KNOTS ( 'NONE', 3,
 ( #8164, #35735, #8388, #4278, #11137, #25495, #43043, #11586, #14779, #32978 ),
 .UNSPECIFIED., .F., .F.,
 ( 4, 3, 3, 4 ),
 ( 0.000000000000000000, 0.0001671877560958130043, 0.0003343755126086565138, 0.0006438490228507229903 ),
 .UNSPECIFIED. ) ;
#4494 = CARTESIAN_POINT ( 'NONE',  ( 111.7327233795247849, -8.938348069036489818, -17.46756447353520159 ) ) ;
#4495 = CARTESIAN_POINT ( 'NONE',  ( 114.7249681442453237, -9.565557343593413364, -10.61323700422348004 ) ) ;
#4496 = CARTESIAN_POINT ( 'NONE',  ( 122.0354079359119908, -5.444069387712269226, -19.60292469916370450 ) ) ;
#4497 = LINE ( 'NONE', #21830, #11907 ) ;
#4498 = EDGE_LOOP ( 'NONE', ( #2231, #31266, #34221, #2103 ) ) ;
#4499 = EDGE_CURVE ( 'NONE', #19842, #38747, #7745, .T. ) ;
#4500 = CARTESIAN_POINT ( 'NONE',  ( 123.9800954359119771, -11.07370829466463569, -12.81314460846529002 ) ) ;
#4501 = CARTESIAN_POINT ( 'NONE',  ( 119.5467348109119712, -4.089484607189486809, -7.948022111789456723 ) ) ;
#4502 = EDGE_LOOP ( 'NONE', ( #4996, #1834, #5293, #16106 ) ) ;
#4503 = LINE ( 'NONE', #11581, #4338 ) ;
#4504 = AXIS2_PLACEMENT_3D ( 'NONE', #15233, #4057, #17757 ) ;
#4505 = CARTESIAN_POINT ( 'NONE',  ( 66.00964506737828685, -2.167441154595251440, -8.806695022995075561 ) ) ;
#4506 = DIRECTION ( 'NONE',  ( 0.000000000000000000, 0.6004852223388321697, -0.7996358532186279566 ) ) ;
#4507 = CARTESIAN_POINT ( 'NONE',  ( 114.0442481442453300, -7.643976991954077427, -18.09477374809248928 ) ) ;
#4508 = CARTESIAN_POINT ( 'NONE',  ( 77.49133083685892132, -56.78909331150907036, -1.672169083734631689 ) ) ;
#4509 = CARTESIAN_POINT ( 'NONE',  ( 64.43697033563542220, -36.18204866848747514, -5.722960826912006027 ) ) ;
#4510 = CARTESIAN_POINT ( 'NONE',  ( 120.7947214775786193, -0.8288870151387760510, -10.36305467784173118 ) ) ;
#4511 = CARTESIAN_POINT ( 'NONE',  ( 121.9470836909669913, -25.99489077589524300, -13.39321520033831447 ) ) ;
#4512 = CARTESIAN_POINT ( 'NONE',  ( 122.6667014775786413, -2.084020599724406786, -8.691656652584148546 ) ) ;
#4513 = EDGE_CURVE ( 'NONE', #26262, #37456, #26892, .T. ) ;
#4514 = CARTESIAN_POINT ( 'NONE',  ( 117.1171583007951966, 0.5154571626197618217, -14.64321520033831447 ) ) ;
#4515 = ADVANCED_FACE ( 'NONE', ( #12148, #37370, #42935 ), #9568, .T. ) ;
#4516 = CARTESIAN_POINT ( 'NONE',  ( 122.7801548109119665, -6.222761293078241884, -8.102969835052219238 ) ) ;
#4517 = CARTESIAN_POINT ( 'NONE',  ( 112.2289948109119848, -1.834011780172310813, -8.268836392978581529 ) ) ;
#4518 = CARTESIAN_POINT ( 'NONE',  ( 119.5467348109119712, -4.089484607189486809, -7.948022111789456723 ) ) ;
#4519 = CARTESIAN_POINT ( 'NONE',  ( 126.4673881442452910, -7.894159318335828068, -9.358103419637847864 ) ) ;
#4520 = DIRECTION ( 'NONE',  ( 0.000000000000000000, 0.000000000000000000, 1.000000000000000000 ) ) ;
#4521 = CARTESIAN_POINT ( 'NONE',  ( 119.6601881442453106, -1.833838273342659253, -17.42832698103878286 ) ) ;
#4522 = ORIENTED_EDGE ( 'NONE', *, *, #16161, .T. ) ;
#4523 = CARTESIAN_POINT ( 'NONE',  ( 122.1561614775786353, -0.4660016031367893996, -10.09054647747474043 ) ) ;
#4524 = CARTESIAN_POINT ( 'NONE',  ( 115.2748327545248657, -6.936859964151250502, -8.388885654883777576 ) ) ;
#4525 = DIRECTION ( 'NONE',  ( 0.000000000000000000, 0.000000000000000000, -1.000000000000000000 ) ) ;
#4526 = DIRECTION ( 'NONE',  ( 0.5735764363510498232, -0.3127926500124802445, 0.7570804645221007600 ) ) ;
#4527 = AXIS2_PLACEMENT_3D ( 'NONE', #9186, #13288, #12842 ) ;
#4528 = CARTESIAN_POINT ( 'NONE',  ( 119.7821199480702603, -6.365377317481695663, -18.95617363400926081 ) ) ;
#4529 = ORIENTED_EDGE ( 'NONE', *, *, #12554, .F. ) ;
#4530 = CARTESIAN_POINT ( 'NONE',  ( 121.5888948109119809, 0.1319031606808879209, -14.10382304977623669 ) ) ;
#4531 = CARTESIAN_POINT ( 'NONE',  ( 124.4252281442453238, -9.261995988541050551, -16.69588392320275361 ) ) ;
#4532 = CARTESIAN_POINT ( 'NONE',  ( 60.62025573688512736, -14.54431086544325247, -19.30358038137204701 ) ) ;
#4533 = CARTESIAN_POINT ( 'NONE',  ( 94.20708369096698220, -25.89439488952623591, -12.28775498424876211 ) ) ;
#4534 = CARTESIAN_POINT ( 'NONE',  ( 105.4819421295248247, -9.868328341294093420, -13.39321520033831447 ) ) ;
#4535 = ORIENTED_EDGE ( 'NONE', *, *, #21109, .F. ) ;
#4536 = CARTESIAN_POINT ( 'NONE',  ( 114.4413348109119823, -9.261995988541697145, -16.69588392320189030 ) ) ;
#4537 = CARTESIAN_POINT ( 'NONE',  ( 125.7866681442452688, -0.4660016031367893996, -10.09054647747474043 ) ) ;
#4538 = CARTESIAN_POINT ( 'NONE',  ( 119.7736414775786358, 0.1319031606808879209, -14.10382304977623669 ) ) ;
#4539 = CARTESIAN_POINT ( 'NONE',  ( 128.2184548109119930, -2.475900776146301219, -7.888945235271306977 ) ) ;
#4540 = CARTESIAN_POINT ( 'NONE',  ( 123.0637881442452937, -0.4660016031367893996, -10.09054647747474043 ) ) ;
#4541 = CARTESIAN_POINT ( 'NONE',  ( 91.11246428952674137, -25.99489077589524300, -13.39321520033831625 ) ) ;
#4542 = PLANE ( 'NONE',  #35390 ) ;
#4543 = DIRECTION ( 'NONE',  ( 0.000000000000000000, -1.000000000000000000, 0.000000000000000000 ) ) ;
#4544 = VERTEX_POINT ( 'NONE', #39729 ) ;
#4545 = DIRECTION ( 'NONE',  ( 0.000000000000000000, 0.000000000000000000, 1.000000000000000000 ) ) ;
#4546 = CARTESIAN_POINT ( 'NONE',  ( 120.3409081442453044, -0.4660016031367893996, -10.09054647747474043 ) ) ;
#4547 = CARTESIAN_POINT ( 'NONE',  ( 67.28358753636723577, -1.679921224420888981, -17.24955508517946967 ) ) ;
#4548 = ORIENTED_EDGE ( 'NONE', *, *, #18053, .T. ) ;
#4549 = PLANE ( 'NONE',  #25480 ) ;
#4550 = CARTESIAN_POINT ( 'NONE',  ( 111.7184548109119788, -0.8288870151387760510, -10.36305467784173118 ) ) ;
#4551 = VECTOR ( 'NONE', #42634, 1000.000000000000114 ) ;
#4552 = CARTESIAN_POINT ( 'NONE',  ( 127.1653849502244498, -4.492243868911367066, -18.85410977821037548 ) ) ;
#4553 = CARTESIAN_POINT ( 'NONE',  ( 124.7088614775786226, -9.565557343593413364, -10.61323700422348004 ) ) ;
#4554 = ORIENTED_EDGE ( 'NONE', *, *, #5509, .T. ) ;
#4555 = CARTESIAN_POINT ( 'NONE',  ( 117.3343948109119737, -3.383040157471821630, -19.15922257007629170 ) ) ;
#4556 = DIRECTION ( 'NONE',  ( -0.5735764363510446051, 0.3127926500124816878, -0.7570804645221042017 ) ) ;
#4557 = LINE ( 'NONE', #21670, #3280 ) ;
#4558 = PRODUCT_DEFINITION_FORMATION_WITH_SPECIFIED_SOURCE ( 'ANY', '', #10294, .NOT_KNOWN. ) ;
#4559 = DIRECTION ( 'NONE',  ( 0.000000000000000000, -0.3818493186865927203, 0.9242245927363029745 ) ) ;
#4560 = CARTESIAN_POINT ( 'NONE',  ( 112.0020881442453344, -9.565557343593413364, -10.61323700422348004 ) ) ;
#4561 = CYLINDRICAL_SURFACE ( 'NONE', #23339, 4.999999999999998224 ) ;
#4562 = VECTOR ( 'NONE', #10190, 1000.000000000000000 ) ;
#4563 = EDGE_CURVE ( 'NONE', #41325, #5895, #29246, .T. ) ;
#4564 = CARTESIAN_POINT ( 'NONE',  ( 67.30914723170953096, -58.80805571747214344, -37.62053433722914519 ) ) ;
#4565 = CARTESIAN_POINT ( 'NONE',  ( 125.5030348109119558, -3.383040157471821630, -19.15922257007629170 ) ) ;
#4566 = CARTESIAN_POINT ( 'NONE',  ( 124.2550481442452792, -0.1624402480850797581, -16.17319339645315424 ) ) ;
#4567 = CARTESIAN_POINT ( 'NONE',  ( 116.6973107111196271, -7.645574652714573816, -17.67460368773177493 ) ) ;
#4568 = CARTESIAN_POINT ( 'NONE',  ( 122.2696148109119889, -5.574606645277164318, -18.38911715685844683 ) ) ;
#4569 = CARTESIAN_POINT ( 'NONE',  ( 112.7395348109119766, -4.153390946401321671, -8.397313243818183892 ) ) ;
#4570 = CARTESIAN_POINT ( 'NONE',  ( 118.0151148109119816, -10.63000616557722466, -14.87417383870573495 ) ) ;
#4571 = CARTESIAN_POINT ( 'NONE',  ( 126.3063647503475693, -8.674798189681249383, -16.69767936789492069 ) ) ;
#4572 = CARTESIAN_POINT ( 'NONE',  ( 116.3860827545247787, -2.477300249445798297, -19.15521520033831138 ) ) ;
#4573 = CARTESIAN_POINT ( 'NONE',  ( 115.4137390045248566, -9.868328341294098749, -11.32035403202665869 ) ) ;
#4574 = CARTESIAN_POINT ( 'NONE',  ( 115.4831921295247952, -9.868328341294093420, -13.39321520033831447 ) ) ;
#4575 = CARTESIAN_POINT ( 'NONE',  ( 126.2758031835838608, -9.794238051865816530, -12.40301975007665192 ) ) ;
#4576 = CARTESIAN_POINT ( 'NONE',  ( 115.0086014775786509, -4.089484607189486809, -7.948022111789456723 ) ) ;
#4577 = ORIENTED_EDGE ( 'NONE', *, *, #31338, .T. ) ;
#4578 = CARTESIAN_POINT ( 'NONE',  ( 113.2500748109119968, -3.505236298600246325, -18.68346056562440793 ) ) ;
#4579 = CARTESIAN_POINT ( 'NONE',  ( 106.4542858795248179, -0.7896495226426338832, -17.46756447353520159 ) ) ;
#4580 = CARTESIAN_POINT ( 'NONE',  ( 119.4900081442453086, -7.643976991954101408, -18.09477374809246797 ) ) ;
#4581 = DIRECTION ( 'NONE',  ( -0.000000000000000000, -0.3818493186865928313, 0.9242245927363027524 ) ) ;
#4582 =( BOUNDED_CURVE ( )  B_SPLINE_CURVE ( 2, ( #37283, #2630, #2403, #20209, #44606, #23862, #20433, #27044, #37748, #33861, #40961, #27274, #44155, #33627, #17235, #19743, #30908 ),
 .UNSPECIFIED., .F., .F. ) 
 B_SPLINE_CURVE_WITH_KNOTS ( ( 3, 2, 2, 2, 2, 2, 2, 2, 3 ),
 ( 0.1035091206787220053, 0.1125000000000000028, 0.1250000000000000000, 0.1375000000000000111, 0.1499999999999999944, 0.1625000000000000056, 0.1749999999999999889, 0.1875000000000000000, 0.1964908793212780114 ),
 .UNSPECIFIED. ) 
 CURVE ( )  GEOMETRIC_REPRESENTATION_ITEM ( )  RATIONAL_B_SPLINE_CURVE ( ( 0.9692594319298230010, 0.9452488050343769155, 1.000000000000000000, 0.9238795325112869605, 1.000000000000000000, 0.9238795325112869605, 1.000000000000000000, 0.9238795325112869605, 1.000000000000000000, 0.9238795325112869605, 1.000000000000000000, 0.9238795325112869605, 1.000000000000000000, 0.9238795325112869605, 1.000000000000000000, 0.9452488050343769155, 0.9692594319298220018 ) ) 
 REPRESENTATION_ITEM ( '' )  );
#4583 = CARTESIAN_POINT ( 'NONE',  ( 67.84197459855160162, -57.36860727972680252, -36.87942510454734446 ) ) ;
#4584 = CARTESIAN_POINT ( 'NONE',  ( 65.24959551893836363, -14.08404458135744797, -17.40216478443592507 ) ) ;
#4585 = CARTESIAN_POINT ( 'NONE',  ( 117.2776681442452968, -5.638512984488999180, -18.83840828888717311 ) ) ;
#4586 = AXIS2_PLACEMENT_3D ( 'NONE', #44356, #30212, #43666 ) ;
#4587 = CARTESIAN_POINT ( 'NONE',  ( 112.5661608795247872, -8.938348069036489818, -9.318865927141430916 ) ) ;
#4588 = CARTESIAN_POINT ( 'NONE',  ( 112.8439733795247832, -1.325403438956436419, -9.854619843455211026 ) ) ;
#4589 = ORIENTED_EDGE ( 'NONE', *, *, #24222, .F. ) ;
#4590 = CARTESIAN_POINT ( 'NONE',  ( 126.2758031835833918, -7.650030489068367245, -9.206835671950464928 ) ) ;
#4591 = CARTESIAN_POINT ( 'NONE',  ( 120.2841814775786276, -10.15424416112533912, -14.75197769757731336 ) ) ;
#4592 = CIRCLE ( 'NONE', #1687, 4.999999999999997335 ) ;
#4593 = CARTESIAN_POINT ( 'NONE',  ( 115.9729548109119861, -6.344957434206662583, -7.627207830600332805 ) ) ;
#4594 = DIRECTION ( 'NONE',  ( 0.000000000000000000, -0.3818493186865927203, 0.9242245927363029745 ) ) ;
#4595 = CARTESIAN_POINT ( 'NONE',  ( 124.8223148109119762, -10.15424416112533912, -14.75197769757731336 ) ) ;
#4596 = PRODUCT_DEFINITION_CONTEXT ( 'detailed design', #40213, 'design' ) ;
#4597 = CARTESIAN_POINT ( 'NONE',  ( 121.0216281442452981, -7.894159318335828068, -9.358103419637847864 ) ) ;
#4598 = CARTESIAN_POINT ( 'NONE',  ( 116.0864081442453113, -0.1624402480850797581, -16.17319339645315424 ) ) ;
#4599 = VERTEX_POINT ( 'NONE', #11696 ) ;
#4600 = CARTESIAN_POINT ( 'NONE',  ( 120.0907204359119760, 1.345710702986147034, -13.97328579221134426 ) ) ;
#4601 = AXIS2_PLACEMENT_3D ( 'NONE', #1971, #36846, #25930 ) ;
#4602 = CARTESIAN_POINT ( 'NONE',  ( 70.19189222814998175, -83.06146523326388831, -51.81246404331846378 ) ) ;
#4603 = CARTESIAN_POINT ( 'NONE',  ( 117.5613014775786525, -10.15424416112533912, -14.75197769757731336 ) ) ;
#4604 = ORIENTED_EDGE ( 'NONE', *, *, #36969, .T. ) ;
#4605 = DIRECTION ( 'NONE',  ( 0.000000000000000000, 0.000000000000000000, 1.000000000000000000 ) ) ;
#4606 = CARTESIAN_POINT ( 'NONE',  ( 116.1431348109119881, -10.30919188438810075, -12.61870101168855918 ) ) ;
#4607 = CARTESIAN_POINT ( 'NONE',  ( 115.6915515045247531, -2.477300249445798297, -7.631215200338321125 ) ) ;
#4608 = CARTESIAN_POINT ( 'NONE',  ( 113.9875214775786532, -8.899110576539710493, -16.42337572283490132 ) ) ;
#4609 = ORIENTED_EDGE ( 'NONE', *, *, #19759, .T. ) ;
#4610 = ORIENTED_EDGE ( 'NONE', *, *, #44845, .T. ) ;
#4611 = CARTESIAN_POINT ( 'NONE',  ( 123.5176014775786228, -0.8288870151387760510, -10.36305467784173118 ) ) ;
#4612 = CARTESIAN_POINT ( 'NONE',  ( 118.6391081442452986, -5.574606645277164318, -18.38911715685844683 ) ) ;
#4613 = CARTESIAN_POINT ( 'NONE',  ( 3.060777270043529619, -5.064559853354640317, -8.893215200338314474 ) ) ;
#4614 = CARTESIAN_POINT ( 'NONE',  ( 121.2714235609119697, 0.6414057260225851653, -11.69287257290600657 ) ) ;
#4615 = ORIENTED_EDGE ( 'NONE', *, *, #41306, .F. ) ;
#4616 = VECTOR ( 'NONE', #15882, 1000.000000000000227 ) ;
#4617 = CARTESIAN_POINT ( 'NONE',  ( 112.1391434465618318, -8.920658433412334887, -16.34206577034920471 ) ) ;
#4618 = CARTESIAN_POINT ( 'NONE',  ( 61.75619731659804756, -65.97429037005174735, -43.35256525270300187 ) ) ;
#4619 = CARTESIAN_POINT ( 'NONE',  ( 111.8021765045248372, -7.250697342233347165, -19.15521520033831138 ) ) ;
#4620 = FACE_OUTER_BOUND ( 'NONE', #22616, .T. ) ;
#4621 = CARTESIAN_POINT ( 'NONE',  ( 113.2500748109119968, -6.344957434206662583, -7.627207830600332805 ) ) ;
#4622 = CARTESIAN_POINT ( 'NONE',  ( 122.0427081442452817, -9.859900752359378018, -12.68260735090039759 ) ) ;
#4623 = DIRECTION ( 'NONE',  ( 0.000000000000000000, 0.000000000000000000, -1.000000000000000000 ) ) ;
#4624 = ORIENTED_EDGE ( 'NONE', *, *, #44819, .F. ) ;
#4625 = CARTESIAN_POINT ( 'NONE',  ( 121.5888948109119809, 0.1319031606808879209, -14.10382304977623669 ) ) ;
#4626 = CARTESIAN_POINT ( 'NONE',  ( 116.4555358795247884, -0.7896495226426338832, -17.46756447353520159 ) ) ;
#4627 = VECTOR ( 'NONE', #20845, 999.9999999999998863 ) ;
#4628 = CARTESIAN_POINT ( 'NONE',  ( 85.43169907558235820, -25.99489077589524300, -13.39321520033831625 ) ) ;
#4629 = CARTESIAN_POINT ( 'NONE',  ( 114.9275671295247889, -10.62599879583958540, -13.39321520033831447 ) ) ;
#4630 = CARTESIAN_POINT ( 'NONE',  ( 117.2776681442452968, -5.638512984488999180, -18.83840828888717311 ) ) ;
#4631 = ORIENTED_EDGE ( 'NONE', *, *, #34388, .T. ) ;
#4632 = CARTESIAN_POINT ( 'NONE',  ( 117.5045748109119756, 0.5811942927096110934, -14.16772938898807510 ) ) ;
#4633 = DIRECTION ( 'NONE',  ( 0.9609149988134837450, -0.1028163501681639419, 0.2570431154366518145 ) ) ;
#4634 = CARTESIAN_POINT ( 'NONE',  ( 107.5655358795247736, -0.7896495226426338832, -17.46756447353520159 ) ) ;
#4635 = CARTESIAN_POINT ( 'NONE',  ( 117.1642148109119859, -9.261995988541697145, -16.69588392320189030 ) ) ;
#4636 = CARTESIAN_POINT ( 'NONE',  ( 118.5823814775786360, -1.834011780172310813, -8.268836392978581529 ) ) ;
#4637 = CARTESIAN_POINT ( 'NONE',  ( 126.5125895482211718, -10.01042591126173598, -13.31191545708816371 ) ) ;
#4638 = DIRECTION ( 'NONE',  ( 0.000000000000000000, 0.000000000000000000, 1.000000000000000000 ) ) ;
#4639 = CARTESIAN_POINT ( 'NONE',  ( 107.7738952545248310, -9.868328341294098749, -15.46607636864997204 ) ) ;
#4640 = ORIENTED_EDGE ( 'NONE', *, *, #40451, .T. ) ;
#4641 = CARTESIAN_POINT ( 'NONE',  ( 92.32016463086877422, -24.14644159042263993, -12.62951656296512937 ) ) ;
#4642 = CARTESIAN_POINT ( 'NONE',  ( 109.2294689093245523, -8.931516418046212991, -16.93750435124538356 ) ) ;
#4643 = CARTESIAN_POINT ( 'NONE',  ( 121.0216281442452981, -7.894159318335828068, -9.358103419637847864 ) ) ;
#4644 = CARTESIAN_POINT ( 'NONE',  ( 112.8439733795247832, -1.325403438956436419, -9.854619843455211026 ) ) ;
#4645 = CARTESIAN_POINT ( 'NONE',  ( 113.6774108795247997, -1.325403438956436419, -16.93181055722141792 ) ) ;
#4646 = CARTESIAN_POINT ( 'NONE',  ( 121.5688035400977611, -1.223627541775709426, -16.99192386690442547 ) ) ;
#4647 = CARTESIAN_POINT ( 'NONE',  ( 115.4056881442453459, -2.084020599724406786, -8.691656652584148546 ) ) ;
#4648 = CARTESIAN_POINT ( 'NONE',  ( 121.9470836909669913, -25.99489077589524300, -13.39321520033831447 ) ) ;
#4649 = CARTESIAN_POINT ( 'NONE',  ( 122.3263414775786373, -6.344957434206665248, -7.627207830600338134 ) ) ;
#4650 = CARTESIAN_POINT ( 'NONE',  ( 119.4900081442453086, -1.834011780172310813, -8.268836392978581529 ) ) ;
#4651 = ORIENTED_EDGE ( 'NONE', *, *, #11207, .T. ) ;
#4652 = VECTOR ( 'NONE', #27634, 1000.000000000000227 ) ;
#4653 = CARTESIAN_POINT ( 'NONE',  ( 118.0718414775786442, -0.8288870151387760510, -10.36305467784173118 ) ) ;
#4654 = CARTESIAN_POINT ( 'NONE',  ( 112.4559014775786494, -9.988377603198976828, -10.36322818467138340 ) ) ;
#4655 = CARTESIAN_POINT ( 'NONE',  ( 120.1140014775786398, -1.561330072975668504, -17.79121239304076951 ) ) ;
#4656 = CARTESIAN_POINT ( 'NONE',  ( 118.1852948109119836, -4.153390946401325223, -8.397313243818185668 ) ) ;
#4657 = ORIENTED_EDGE ( 'NONE', *, *, #38994, .F. ) ;
#4658 = CARTESIAN_POINT ( 'NONE',  ( 123.5743281442453139, -2.084020599724406786, -8.691656652584148546 ) ) ;
#4659 = ADVANCED_FACE ( 'NONE', ( #8717 ), #24477, .T. ) ;
#4660 = ADVANCED_FACE ( 'NONE', ( #6141 ), #18761, .T. ) ;
#4661 = CARTESIAN_POINT ( 'NONE',  ( 121.3619881442452879, -4.089484607189486809, -7.948022111789456723 ) ) ;
#4662 = CARTESIAN_POINT ( 'NONE',  ( 125.0302870206146082, -8.104358653442693239, -6.574584932803245962 ) ) ;
#4663 = CARTESIAN_POINT ( 'NONE',  ( 108.3295202545248657, -10.62599879583958717, -15.77991374673208469 ) ) ;
#4664 = CARTESIAN_POINT ( 'NONE',  ( 60.06931813437629586, -14.72076136720887085, -8.603412892520118760 ) ) ;
#4665 = DIRECTION ( 'NONE',  ( 0.9908103287288504424, -0.1352586133457949757, 0.000000000000000000 ) ) ;
#4666 = CARTESIAN_POINT ( 'NONE',  ( 113.2606921295247702, -9.868328341294093420, -13.39321520033831447 ) ) ;
#4667 = CARTESIAN_POINT ( 'NONE',  ( 118.8660148109119774, -10.30919188438810075, -12.61870101168855918 ) ) ;
#4668 = DIRECTION ( 'NONE',  ( 1.000000000000000000, 0.000000000000000000, 0.000000000000000000 ) ) ;
#4669 = CARTESIAN_POINT ( 'NONE',  ( 117.4478481442453131, -9.565557343593413364, -10.61323700422348004 ) ) ;
#4670 = CARTESIAN_POINT ( 'NONE',  ( 124.6521348109119884, -1.561330072975668948, -17.79121239304076951 ) ) ;
#4671 = CARTESIAN_POINT ( 'NONE',  ( 126.2872529661351848, -0.6579534352730314062, -10.62653152189244388 ) ) ;
#4672 = CARTESIAN_POINT ( 'NONE',  ( -13.74784922440762713, -3.813634959067930819, -8.495864720811209025 ) ) ;
#4673 = CARTESIAN_POINT ( 'NONE',  ( 111.3854577545248645, -2.791137627527939813, -18.39754474579286025 ) ) ;
#4674 = CARTESIAN_POINT ( 'NONE',  ( 114.3278814775786429, 0.1319031606808879209, -14.10382304977623669 ) ) ;
#4675 = DIRECTION ( 'NONE',  ( -1.000000000000000000, 0.000000000000000000, 0.000000000000000000 ) ) ;
#4676 = EDGE_CURVE ( 'NONE', #31533, #14596, #43154, .T. ) ;
#4677 = LINE ( 'NONE', #18598, #17313 ) ;
#4679 = CARTESIAN_POINT ( 'NONE',  ( 120.3409081442453044, -0.4660016031367893996, -10.09054647747474043 ) ) ;
#4678 = CARTESIAN_POINT ( 'NONE',  ( 66.01387875770896585, -14.50705293059987788, -10.06447537375617252 ) ) ;
#4680 = CARTESIAN_POINT ( 'NONE',  ( 120.6812681442452941, 0.1319031606808879209, -14.10382304977623669 ) ) ;
#4681 = CARTESIAN_POINT ( 'NONE',  ( 114.1577014775786552, -3.505236298600246325, -18.68346056562440793 ) ) ;
#4682 = ORIENTED_EDGE ( 'NONE', *, *, #38681, .T. ) ;
#4683 = CARTESIAN_POINT ( 'NONE',  ( 136.7082020370380349, -9.210996569390418998, -9.790749321066718025 ) ) ;
#4684 = CARTESIAN_POINT ( 'NONE',  ( 126.1837548109119211, -10.63000616557722466, -14.87417383870573495 ) ) ;
#4685 = CARTESIAN_POINT ( 'NONE',  ( 115.4137390045248566, -9.868328341294098749, -11.32035403202665869 ) ) ;
#4686 = CARTESIAN_POINT ( 'NONE',  ( 120.1707281442453166, -9.565557343593413364, -10.61323700422348004 ) ) ;
#4687 = EDGE_CURVE ( 'NONE', #28617, #13270, #42710, .T. ) ;
#4688 = CARTESIAN_POINT ( 'NONE',  ( 123.0637881442452937, -8.899110576539710493, -16.42337572283490132 ) ) ;
#4689 = CARTESIAN_POINT ( 'NONE',  ( 116.4267681442453153, -6.222761293078241884, -8.102969835052219238 ) ) ;
#4690 = EDGE_CURVE ( 'NONE', #8497, #14657, #20835, .T. ) ;
#4691 = CARTESIAN_POINT ( 'NONE',  ( 86.51169734173754478, -25.99489077589583630, -8.393215200338314474 ) ) ;
#4692 = CARTESIAN_POINT ( 'NONE',  ( 106.3153796295248412, -4.863998795839590272, -19.15521520033831493 ) ) ;
#4693 = CARTESIAN_POINT ( 'NONE',  ( 124.7655881442452852, -9.859900752359378018, -12.68260735090039759 ) ) ;
#4694 = CARTESIAN_POINT ( 'NONE',  ( 123.9714148109119805, -8.899110576539710493, -16.42337572283490132 ) ) ;
#4695 = DIRECTION ( 'NONE',  ( 1.000000000000000000, 0.000000000000000000, 0.000000000000000000 ) ) ;
#4696 = CARTESIAN_POINT ( 'NONE',  ( 73.01241679510815175, -68.13509210538408922, -39.58160742654554554 ) ) ;
#4697 = CARTESIAN_POINT ( 'NONE',  ( 123.4244704359119709, 1.345710702986147034, -13.97328579221134426 ) ) ;
#4698 = CARTESIAN_POINT ( 'NONE',  ( 114.9970202545248412, -10.62599879583958717, -15.77991374673208469 ) ) ;
#4699 = B_SPLINE_CURVE_WITH_KNOTS ( 'NONE', 3,
 ( #33056, #34144, #20258, #1606, #19175, #15759, #44659, #5260, #2683, #6111 ),
 .UNSPECIFIED., .F., .F.,
 ( 4, 3, 3, 4 ),
 ( 0.000000000000000000, 0.0001671877560958105107, 0.0003343755126086574896, 0.0006438490228507220145 ),
 .UNSPECIFIED. ) ;
#4700 = CARTESIAN_POINT ( 'NONE',  ( 116.9314277858571955, 1.864452410925628856, -21.08963232287759837 ) ) ;
#4701 = CARTESIAN_POINT ( 'NONE',  ( 116.2471765045247594, -7.250697342233347165, -19.15521520033831138 ) ) ;
#4702 = CARTESIAN_POINT ( 'NONE',  ( 118.1285681442453068, -7.893985811506177619, -18.51759400769804742 ) ) ;
#4703 = CARTESIAN_POINT ( 'NONE',  ( 118.7525614775786380, -8.166667518702819706, -8.995218007635861213 ) ) ;
#4704 = CARTESIAN_POINT ( 'NONE',  ( 107.7044421295247929, 0.8980012041604618078, -13.39321520033831447 ) ) ;
#4705 = CARTESIAN_POINT ( 'NONE',  ( 114.0442481442453300, -1.834011780172310813, -8.268836392978581529 ) ) ;
#4706 = LINE ( 'NONE', #32516, #24999 ) ;
#4707 = EDGE_LOOP ( 'NONE', ( #16154, #4167, #4930, #15408 ) ) ;
#4708 = CARTESIAN_POINT ( 'NONE',  ( 116.2503515045248719, -2.792930983974093007, -8.393215200338321580 ) ) ;
#4709 = EDGE_CURVE ( 'NONE', #15070, #23958, #36857, .T. ) ;
#4710 = AXIS2_PLACEMENT_3D ( 'NONE', #41168, #13788, #37727 ) ;
#4711 = CARTESIAN_POINT ( 'NONE',  ( 116.0296814775786345, -8.166667518702817929, -8.995218007635861213 ) ) ;
#4712 = CARTESIAN_POINT ( 'NONE',  ( 121.4187148109119789, -3.505236298600246325, -18.68346056562440793 ) ) ;
#4713 = EDGE_CURVE ( 'NONE', #16653, #3445, #36003, .T. ) ;
#4714 = CARTESIAN_POINT ( 'NONE',  ( 115.1787814775786387, -0.1624402480850797581, -16.17319339645315424 ) ) ;
#4715 = CARTESIAN_POINT ( 'NONE',  ( 122.1561614775786353, -0.4660016031367893996, -10.09054647747474043 ) ) ;
#4716 = EDGE_CURVE ( 'NONE', #35115, #21529, #43427, .T. ) ;
#4717 = ADVANCED_FACE ( 'NONE', ( #41964 ), #42858, .T. ) ;
#4718 = AXIS2_PLACEMENT_3D ( 'NONE', #14274, #11305, #25214 ) ;
#4719 = CARTESIAN_POINT ( 'NONE',  ( 114.8581140045248361, -10.62599879583958717, -11.00651665394454604 ) ) ;
#4720 = CARTESIAN_POINT ( 'NONE',  ( 116.7671281442453335, -7.643976991954077427, -18.09477374809248928 ) ) ;
#4721 = CARTESIAN_POINT ( 'NONE',  ( 123.0772048109119652, -7.554583864224885481, -18.48844787311982785 ) ) ;
#4722 = LINE ( 'NONE', #24802, #27924 ) ;
#4723 = ORIENTED_EDGE ( 'NONE', *, *, #29098, .F. ) ;
#4724 = CARTESIAN_POINT ( 'NONE',  ( 120.1601735609119856, -9.645473719204776586, -14.86997237629376656 ) ) ;
#4725 = CARTESIAN_POINT ( 'NONE',  ( 118.9227414775786400, -10.63000616557722466, -14.87417383870573495 ) ) ;
#4726 = ORIENTED_EDGE ( 'NONE', *, *, #18366, .F. ) ;
#4727 = LINE ( 'NONE', #32753, #29842 ) ;
#4728 = CARTESIAN_POINT ( 'NONE',  ( 128.2184548109119930, -7.252096815532139473, -18.89748516540533529 ) ) ;
#4729 = LINE ( 'NONE', #5847, #519 ) ;
#4730 = CARTESIAN_POINT ( 'NONE',  ( 115.6325948109119821, -9.565557343593413364, -10.61323700422348004 ) ) ;
#4731 = FACE_OUTER_BOUND ( 'NONE', #29352, .T. ) ;
#4732 = CARTESIAN_POINT ( 'NONE',  ( 124.5122867449678097, -9.720823321642505732, -12.20364227757116282 ) ) ;
#4733 = CARTESIAN_POINT ( 'NONE',  ( 122.5532481442453019, 0.4262465694468514643, -12.03445270309931736 ) ) ;
#4734 = CARTESIAN_POINT ( 'NONE',  ( 121.1918081442452859, 0.9020085738987244639, -11.91225656197088156 ) ) ;
#4735 = CARTESIAN_POINT ( 'NONE',  ( 125.1059481442452750, -1.833838273342660141, -17.42832698103878286 ) ) ;
#4736 = DIRECTION ( 'NONE',  ( 1.000000000000000000, 0.000000000000000000, -0.000000000000000000 ) ) ;
#4737 = CARTESIAN_POINT ( 'NONE',  ( 124.0281414775786146, -7.643976991954077427, -18.09477374809248928 ) ) ;
#4738 = CARTESIAN_POINT ( 'NONE',  ( 114.3278814775786429, -10.30919188438810075, -12.61870101168855918 ) ) ;
#4739 = CARTESIAN_POINT ( 'NONE',  ( 117.7314814775786260, -4.089484607189486809, -7.948022111789456723 ) ) ;
#4740 = CARTESIAN_POINT ( 'NONE',  ( 125.7299414775786346, -10.15424416112533912, -14.75197769757731336 ) ) ;
#4741 = DIRECTION ( 'NONE',  ( 1.000000000000000000, 0.000000000000000000, 0.000000000000000000 ) ) ;
#4742 = CONICAL_SURFACE ( 'NONE', #14941, 1.610000000000000986, 0.9599310885968765916 ) ;
#4743 = CARTESIAN_POINT ( 'NONE',  ( 118.8660148109119774, 0.1319031606808879209, -14.10382304977623669 ) ) ;
#4744 = VERTEX_POINT ( 'NONE', #15891 ) ;
#4745 = CARTESIAN_POINT ( 'NONE',  ( 121.4754414775786131, -8.166667518702819706, -8.995218007635861213 ) ) ;
#4746 = CARTESIAN_POINT ( 'NONE',  ( 112.9134265045247645, -2.791137627527939813, -8.388885654883777576 ) ) ;
#4747 = CARTESIAN_POINT ( 'NONE',  ( 82.55633208288642777, -31.76683555124534664, -22.98062779949958312 ) ) ;
#4748 = CARTESIAN_POINT ( 'NONE',  ( 113.2500748109119968, -3.505236298600246325, -18.68346056562440793 ) ) ;
#4749 = CARTESIAN_POINT ( 'NONE',  ( 86.04230958663552542, -25.82262605124138943, -7.893215200338315363 ) ) ;
#4750 = CARTESIAN_POINT ( 'NONE',  ( 125.1626748109119802, -9.988377603198980381, -10.36322818467138518 ) ) ;
#4751 = ORIENTED_EDGE ( 'NONE', *, *, #20284, .T. ) ;
#4752 = CARTESIAN_POINT ( 'NONE',  ( 121.0783548109119749, -9.565557343593413364, -10.61323700422348004 ) ) ;
#4753 = CARTESIAN_POINT ( 'NONE',  ( 121.2714235609119697, 0.6414057260225851653, -11.69287257290600657 ) ) ;
#4754 = CARTESIAN_POINT ( 'NONE',  ( 121.4103298109119748, -2.173413727453600508, -8.297982527556802879 ) ) ;
#4755 = EDGE_CURVE ( 'NONE', #31560, #2818, #7969, .T. ) ;
#4756 = CARTESIAN_POINT ( 'NONE',  ( 55.68041887817022939, -39.85035523279287162, -17.39321520033831447 ) ) ;
#4757 = CARTESIAN_POINT ( 'NONE',  ( 108.5378796295247810, -4.863998795839590272, -8.388885654883775800 ) ) ;
#4758 = ORIENTED_EDGE ( 'NONE', *, *, #41547, .F. ) ;
#4759 = CARTESIAN_POINT ( 'NONE',  ( 115.0653281442453277, -6.344957434206662583, -7.627207830600332805 ) ) ;
#4760 = DIRECTION ( 'NONE',  ( 1.000000000000000000, 0.000000000000000000, 0.000000000000000000 ) ) ;
#4761 = CARTESIAN_POINT ( 'NONE',  ( 120.7379948109119709, 0.4262465694468514643, -12.03445270309931736 ) ) ;
#4762 = CARTESIAN_POINT ( 'NONE',  ( 126.2202699136542066, -4.102562024790352702, -8.450529750232742998 ) ) ;
#4763 = SHAPE_REPRESENTATION_RELATIONSHIP ( 'NONE' , 'NONE' ,  #30918, #43323 ) ;
#4764 = CARTESIAN_POINT ( 'NONE',  ( 111.9453614775786434, -7.894159318335828068, -9.358103419637847864 ) ) ;
#4765 = CARTESIAN_POINT ( 'NONE',  ( 63.10250807381770244, -31.76310523276723430, -22.89321520033831803 ) ) ;
#4766 = DIRECTION ( 'NONE',  ( 0.000000000000000000, 0.000000000000000000, -1.000000000000000000 ) ) ;
#4767 = CARTESIAN_POINT ( 'NONE',  ( 124.8790414775786246, -8.899110576539710493, -16.42337572283490132 ) ) ;
#4768 = ORIENTED_EDGE ( 'NONE', *, *, #41411, .F. ) ;
#4769 = AXIS2_PLACEMENT_3D ( 'NONE', #35677, #5351, #15166 ) ;
#4770 = LINE ( 'NONE', #15045, #37993 ) ;
#4771 = CARTESIAN_POINT ( 'NONE',  ( 119.8303681442453126, -10.63000616557722466, -14.87417383870573495 ) ) ;
#4772 = CARTESIAN_POINT ( 'NONE',  ( 137.1886586612278052, -9.618365390465340781, -15.78023550484489235 ) ) ;
#4773 = EDGE_LOOP ( 'NONE', ( #8065, #43824, #9275, #22865, #23073, #33451 ) ) ;
#4774 = EDGE_CURVE ( 'NONE', #44682, #27626, #39435, .T. ) ;
#4775 = CARTESIAN_POINT ( 'NONE',  ( 73.37572422742091760, -11.86958442233774313, -21.89321520033831447 ) ) ;
#4776 = CARTESIAN_POINT ( 'NONE',  ( 124.6521348109119884, -1.561330072975668948, -17.79121239304076951 ) ) ;
#4777 = CIRCLE ( 'NONE', #41931, 2.000000000000000444 ) ;
#4778 = PLANE ( 'NONE',  #19126 ) ;
#4779 = CARTESIAN_POINT ( 'NONE',  ( 124.3685014775786328, 0.4262465694468514643, -12.03445270309931736 ) ) ;
#4780 = ORIENTED_EDGE ( 'NONE', *, *, #43691, .T. ) ;
#4781 = CARTESIAN_POINT ( 'NONE',  ( 116.5969481442453031, 0.5811942927096154232, -14.16772938898807155 ) ) ;
#4782 = DIRECTION ( 'NONE',  ( -1.000000000000000000, 0.000000000000000000, -0.000000000000000000 ) ) ;
#4783 = CARTESIAN_POINT ( 'NONE',  ( 116.7715436525450343, -2.378957183258571639, -17.95140958770219086 ) ) ;
#4784 = DIRECTION ( 'NONE',  ( 4.844864995884620227E-15, -6.938893903907220489E-15, 1.000000000000000000 ) ) ;
#4785 = CARTESIAN_POINT ( 'NONE',  ( 111.4481564080329576, -2.480768857730201393, -17.81583212108824554 ) ) ;
#4786 = CARTESIAN_POINT ( 'NONE',  ( 112.3991748109119868, -1.833838273342658809, -17.42832698103878286 ) ) ;
#4787 = DIRECTION ( 'NONE',  ( 1.000000000000000000, 0.000000000000000000, 0.000000000000000000 ) ) ;
#4788 = DIRECTION ( 'NONE',  ( -0.9908103287288504424, 0.1352586133457950590, 0.000000000000000000 ) ) ;
#4789 = CARTESIAN_POINT ( 'NONE',  ( 112.7962614775786676, -6.222761293078241884, -8.102969835052219238 ) ) ;
#4790 = CARTESIAN_POINT ( 'NONE',  ( 111.7751814775786556, -7.893985811506177619, -18.51759400769804742 ) ) ;
#4791 = CARTESIAN_POINT ( 'NONE',  ( 116.7009281483881296, -7.496663152239960048, -17.77315041048467847 ) ) ;
#4792 = CARTESIAN_POINT ( 'NONE',  ( 122.8368814775786291, -7.894159318335828068, -9.358103419637847864 ) ) ;
#4793 = CARTESIAN_POINT ( 'NONE',  ( 113.5337081442453240, -0.8288870151387760510, -10.36305467784173118 ) ) ;
#4794 = CARTESIAN_POINT ( 'NONE',  ( 117.9583881442453048, -10.30919188438810075, -12.61870101168855918 ) ) ;
#4795 = ORIENTED_EDGE ( 'NONE', *, *, #23426, .F. ) ;
#4796 = CARTESIAN_POINT ( 'NONE',  ( 117.8266488976800161, -1.244021962887374544, -16.96476564598603076 ) ) ;
#4797 = CARTESIAN_POINT ( 'NONE',  ( 96.46827370896536991, -25.99489077589524300, -13.39321520033831447 ) ) ;
#4798 = CIRCLE ( 'NONE', #14278, 2.000000000000000444 ) ;
#4799 = CARTESIAN_POINT ( 'NONE',  ( 110.8298327545248299, -6.936859964151250502, -8.388885654883777576 ) ) ;
#4800 = CARTESIAN_POINT ( 'NONE',  ( 109.0240515045248202, -6.936859964151250502, -18.39754474579286025 ) ) ;
#4801 = CARTESIAN_POINT ( 'NONE',  ( 126.2202699136542350, -9.806684245945831435, -12.63177842929600203 ) ) ;
#4802 = CARTESIAN_POINT ( 'NONE',  ( 116.3133148109119759, -7.893985811506177619, -18.51759400769804742 ) ) ;
#4803 = ORIENTED_EDGE ( 'NONE', *, *, #24252, .T. ) ;
#4804 = CARTESIAN_POINT ( 'NONE',  ( 116.0864081442453113, -0.1624402480850797581, -16.17319339645315424 ) ) ;
#4805 = CARTESIAN_POINT ( 'NONE',  ( 109.0240515045248202, -2.477300249445798297, -7.631215200338321125 ) ) ;
#4806 = DIRECTION ( 'NONE',  ( -0.000000000000000000, -0.9284778069183721172, -0.3713878862591650232 ) ) ;
#4807 = CARTESIAN_POINT ( 'NONE',  ( 125.7866681442452688, -0.4660016031367893996, -10.09054647747474043 ) ) ;
#4808 = CARTESIAN_POINT ( 'NONE',  ( 123.1772414775786189, -5.574606645277164318, -18.38911715685844683 ) ) ;
#4809 = FACE_BOUND ( 'NONE', #14857, .T. ) ;
#4810 = CARTESIAN_POINT ( 'NONE',  ( 116.4834948109119779, -1.561330072975668504, -17.79121239304076951 ) ) ;
#4811 = CARTESIAN_POINT ( 'NONE',  ( 109.9269421295247753, 0.8980012041604618078, -13.39321520033831447 ) ) ;
#4812 = CARTESIAN_POINT ( 'NONE',  ( 110.2742077545248094, -2.791137627527939813, -18.39754474579286025 ) ) ;
#4813 = ORIENTED_EDGE ( 'NONE', *, *, #43220, .T. ) ;
#4814 = CYLINDRICAL_SURFACE ( 'NONE', #5541, 1.999999999999998890 ) ;
#4815 = CARTESIAN_POINT ( 'NONE',  ( 119.3198281442452924, -9.859900752359374465, -12.68260735090039404 ) ) ;
#4816 = CARTESIAN_POINT ( 'NONE',  ( 114.7249681442453237, 0.2603800115204892296, -16.42320221600525088 ) ) ;
#4817 = CARTESIAN_POINT ( 'NONE',  ( 113.5337081442453240, -9.261995988541697145, -16.69588392320189030 ) ) ;
#4818 = CARTESIAN_POINT ( 'NONE',  ( 124.9357681442453014, -7.643976991954077427, -18.09477374809248928 ) ) ;
#4819 = CARTESIAN_POINT ( 'NONE',  ( 123.6877814775786533, -6.222761293078241884, -8.102969835052219238 ) ) ;
#4820 = CARTESIAN_POINT ( 'NONE',  ( 115.4624148109119943, -4.153390946401321671, -8.397313243818183892 ) ) ;
#4821 = VERTEX_POINT ( 'NONE', #42412 ) ;
#4822 = CARTESIAN_POINT ( 'NONE',  ( 121.2019704359119743, 1.345710702986147034, -13.97328579221134426 ) ) ;
#4823 = ADVANCED_FACE ( 'NONE', ( #25529 ), #25080, .F. ) ;
#4824 = VECTOR ( 'NONE', #24022, 1000.000000000000114 ) ;
#4825 = CARTESIAN_POINT ( 'NONE',  ( 113.7248434012278722, 0.04929351793716424401, -14.64321520033828605 ) ) ;
#4826 = CARTESIAN_POINT ( 'NONE',  ( 118.6391081442452986, -5.574606645277164318, -18.38911715685844683 ) ) ;
#4827 = EDGE_LOOP ( 'NONE', ( #9468, #44057, #16669, #18786, #23239 ) ) ;
#4828 = DIRECTION ( 'NONE',  ( 0.9908103287288504424, -0.1352586133457951423, 0.000000000000000000 ) ) ;
#4829 = CARTESIAN_POINT ( 'NONE',  ( 116.0864081442453113, -9.988377603198976828, -10.36322818467138340 ) ) ;
#4830 = CARTESIAN_POINT ( 'NONE',  ( 108.3989733795247759, -1.325403438956436419, -9.854619843455211026 ) ) ;
#4831 = CARTESIAN_POINT ( 'NONE',  ( 113.0798948109119948, -8.899110576539710493, -16.42337572283490132 ) ) ;
#4832 = AXIS2_PLACEMENT_3D ( 'NONE', #37080, #13836, #6777 ) ;
#4833 = ORIENTED_EDGE ( 'NONE', *, *, #23174, .T. ) ;
#4834 = ORIENTED_EDGE ( 'NONE', *, *, #2994, .T. ) ;
#4835 = CARTESIAN_POINT ( 'NONE',  ( 121.6456214775786293, 0.4262465694468514643, -12.03445270309931736 ) ) ;
#4836 = B_SPLINE_CURVE_WITH_KNOTS ( 'NONE', 3,
 ( #24961, #35426, #42523, #7859, #565, #4431, #777, #7397, #14700, #41855 ),
 .UNSPECIFIED., .F., .F.,
 ( 4, 2, 2, 2, 4 ),
 ( 0.000000000000000000, 0.2499999999999472644, 0.3749999999999558686, 0.4999999999999644729, 1.000000000000000000 ),
 .UNSPECIFIED. ) ;
#4837 = CARTESIAN_POINT ( 'NONE',  ( 116.1431348109119881, 0.1319031606808879209, -14.10382304977623669 ) ) ;
#4838 = CARTESIAN_POINT ( 'NONE',  ( 88.98550738977573360, -10.74509419609185379, -14.14321520033831625 ) ) ;
#4839 = CONICAL_SURFACE ( 'NONE', #25981, 2.999999999999999556, 0.9599310885968830309 ) ;
#4840 = CARTESIAN_POINT ( 'NONE',  ( 116.1998614775786649, 0.4262465694468561273, -12.03445270309934223 ) ) ;
#4841 = EDGE_LOOP ( 'NONE', ( #27472, #24 ) ) ;
#4842 = DIRECTION ( 'NONE',  ( 0.5040994586965589219, 0.8636456077245089347, 0.000000000000000000 ) ) ;
#4843 = CARTESIAN_POINT ( 'NONE',  ( 61.69189222814999596, -66.25068106556746272, -42.68838236875360792 ) ) ;
#4844 = CARTESIAN_POINT ( 'NONE',  ( 109.3713171295247832, -10.62599879583958540, -13.39321520033831447 ) ) ;
#4845 = EDGE_CURVE ( 'NONE', #35887, #24167, #34676, .T. ) ;
#4846 = CARTESIAN_POINT ( 'NONE',  ( 115.6893214775786447, 0.5811942927096154232, -14.16772938898807155 ) ) ;
#4848 = CARTESIAN_POINT ( 'NONE',  ( 115.4056881442453459, -2.084020599724406786, -8.691656652584148546 ) ) ;
#4847 = CARTESIAN_POINT ( 'NONE',  ( 125.9001214775786224, -5.574606645277164318, -18.38911715685844683 ) ) ;
#4849 =( BOUNDED_SURFACE ( )  B_SPLINE_SURFACE ( 1, 2, ( 
 ( #44806, #13564, #24056, #37949, #23374, #37254, #23607, #19717, #9461, #44582, #6722, #2837, #26566, #27249, #12896, #16077, #2380, #29981, #37724, #30211, #6027, #33839, #26794, #43899, #19950, #40478, #9239, #27022, #40937, #9690, #40703, #2607, #16539, #6266, #20186, #34071, #16766, #30663, #9924, #23837, #35401, #24706, #31319, #38831, #28589, #31545, #7835, #21287, #10370, #21741, #21062, #31990, #11035, #313, #34727, #24279, #42270, #20848, #41615, #31768, #540, #14006, #27698, #34940, #7151, #27922, #3510, #38166, #7599, #38596, #14452, #42499, #25167, #31103, #3289, #3949, #17647, #21515, #6945, #14228, #28142, #17427, #3727, #39065, #24934, #17210, #94, #17872, #7373, #41832, #42053, #10811, #10592, #45028, #13786, #24494, #28357, #38379, #35172, #4177, #18094, #751, #14675, #11259, #36304, #1871, #42722, #32439, #1428, #12157, #32660, #39964, #29256, #43612, #32213, #35630, #11935, #18771, #4407, #43165, #25831, #39739, #22185, #12387, #5072, #1212, #15347, #26285, #36531, #15570, #15126, #29033, #987, #5303, #42943, #11705, #40193, #15798, #8507, #21965, #26060, #8726, #18546, #19219, #29700, #22411, #8959, #8283, #33099, #18989, #11489, #36082, #32877, #22632, #1648, #8058, #18322, #14902, #28814, #29476, #43390, #25616, #25394, #39521, #39290, #35851, #4625, #4853, #16023, #16482, #40647, #2785, #20355, #13513, #30382, #36750, #23781, #23089, #12612, #37198, #6447, #19660, #2097, #41112, #40880, #9870, #13059, #30157, #41343, #37437, #27192, #44304, #19440, #43845, #9634, #12840, #26515, #23554, #37671, #16254, #44075, #26959, #29931, #26739, #30831, #6208, #34240, #16711, #40423, #9183, #23313, #36972, #5519, #20130, #27422, #22859, #9403, #5741, #19895, #33323, #33547, #5971, #33782, #30604, #3013, #34016, #2326, #44522, #13286, #2552, #16936, #44754, #14560, #35282, #10318, #17161, #1097, #32103, #39175, #4740, #32552, #37891, #10100, #11373, #25051, #15013, #13736, #7713, #21626, #44978, #42383, #1321, #4519, #24004, #34455, #25279, #14789 ),
 ( #31049, #28703, #645, #27645, #7939, #42833, #4056, #17980, #870, #3235, #31880, #18661, #42608, #25504, #35746, #41559, #24221, #11147, #38714, #6668, #21850, #15232, #29141, #28479, #7483, #35514, #20577, #21402, #38945, #4286, #18442, #28926, #32331, #11594, #18205, #39409, #8172, #22082, #35970, #43733, #9300, #4964, #39858, #8843, #19556, #40080, #2212, #36644, #5861, #39635, #43054, #19333, #26174, #11820, #5417, #33219, #1994, #29593, #19783, #12502, #8623, #22742, #33665, #43959, #22975, #22521, #36418, #8398, #12722, #5186, #19103, #2443, #23208, #15919, #29368, #33433, #16141, #25951, #26625, #37087, #29817, #16365, #15690, #40539, #26399, #18876, #43510, #40309, #30043, #9073, #12278, #15462, #25728, #36865, #22302, #36199, #32990, #12049, #5635, #32767, #43279, #1764, #1541, #38008, #34570, #20469, #6552, #44193, #20692, #41448, #44413, #27757, #30945, #41672, #37322, #27082, #41226, #6782, #27309, #3353, #23896, #38221, #26851, #30267, #34350, #13407, #12955, #37779, #3128, #17053, #16828, #7001, #44868, #41002, #9985, #20912, #31163, #10206, #9756, #23667, #40764, #45082, #37555, #6326, #34786, #10429, #13624, #16600, #17272, #13841, #13179, #24337, #3569, #27534, #9521, #2899, #23438, #24114, #6093, #30721, #20012, #33897, #2667, #30493, #20244, #34130, #44644, #42334, #14511, #28205, #27983, #375, #17481, #1044, #22025, #600, #10649, #11095, #35233, #42555, #14960, #8123, #24996, #31379, #18388, #17706, #7211, #31830, #28872, #14286, #41887, #35692, #35462, #4468, #7660, #24768, #35918, #32051, #21798, #38891, #14064, #38441, #4237, #7428, #21124, #18155, #32276, #10873, #38659, #21575, #24555, #21349, #25453, #818, #42785, #11317, #34998, #3782, #31606, #11546, #14737, #39355, #28649, #4009, #150, #25227, #42113, #39125, #17931, #28423, #7892, #39800, #8343, #5367, #36813, #43227, #11994, #40024, #42998, #25896, #12676, #36592, #19505, #29761, #11765, #36140, #5135, #22244, #32496, #8789, #9247, #23156, #8569, #18824, #1712, #4684, #4908 ) ),
 .UNSPECIFIED., .F., .F., .F. ) 
 B_SPLINE_SURFACE_WITH_KNOTS ( ( 2, 2 ),
 ( 3, 2, 2, 2, 2, 2, 2, 2, 2, 2, 2, 2, 2, 2, 2, 2, 2, 2, 2, 2, 2, 2, 2, 2, 2, 2, 2, 2, 2, 2, 2, 2, 2, 2, 2, 2, 2, 2, 2, 2, 2, 2, 2, 2, 2, 2, 2, 2, 2, 2, 2, 2, 2, 2, 2, 2, 2, 2, 2, 2, 2, 2, 2, 2, 2, 2, 2, 2, 2, 2, 2, 2, 2, 2, 2, 2, 2, 2, 2, 2, 2, 2, 2, 2, 2, 2, 2, 2, 2, 2, 2, 2, 2, 2, 2, 2, 2, 2, 2, 2, 2, 2, 2, 2, 2, 2, 2, 2, 2, 2, 2, 2, 2, 2, 2, 2, 2, 2, 2, 2, 2, 2, 2, 2, 2, 2, 2, 2, 3 ),
 ( 0.000000000000000000, 1.000000000000000000 ),
 ( 0.000000000000000000, 0.007812500000000000000, 0.01562500000000000000, 0.02343750000000000000, 0.03125000000000000000, 0.03906250000000000000, 0.04687500000000000000, 0.05468750000000000000, 0.06250000000000000000, 0.07031250000000000000, 0.07812500000000000000, 0.08593750000000000000, 0.09375000000000000000, 0.1015625000000000000, 0.1093750000000000000, 0.1171875000000000000, 0.1250000000000000000, 0.1328125000000000000, 0.1406250000000000000, 0.1484375000000000000, 0.1562500000000000000, 0.1640625000000000000, 0.1718750000000000000, 0.1796875000000000000, 0.1875000000000000000, 0.1953125000000000000, 0.2031250000000000000, 0.2109375000000000000, 0.2187500000000000000, 0.2265625000000000000, 0.2343750000000000000, 0.2421875000000000000, 0.2500000000000000000, 0.2578125000000000000, 0.2656250000000000000, 0.2734375000000000000, 0.2812500000000000000, 0.2890625000000000000, 0.2968750000000000000, 0.3046875000000000000, 0.3125000000000000000, 0.3203125000000000000, 0.3281250000000000000, 0.3359375000000000000, 0.3437500000000000000, 0.3515625000000000000, 0.3593750000000000000, 0.3671875000000000000, 0.3750000000000000000, 0.3828125000000000000, 0.3906250000000000000, 0.3984375000000000000, 0.4062500000000000000, 0.4140625000000000000, 0.4218750000000000000, 0.4296875000000000000, 0.4375000000000000000, 0.4453125000000000000, 0.4531250000000000000, 0.4609375000000000000, 0.4687500000000000000, 0.4765625000000000000, 0.4843750000000000000, 0.4921875000000000000, 0.5000000000000000000, 0.5078125000000000000, 0.5156250000000000000, 0.5234375000000000000, 0.5312500000000000000, 0.5390625000000000000, 0.5468750000000000000, 0.5546875000000000000, 0.5625000000000000000, 0.5703125000000000000, 0.5781250000000000000, 0.5859375000000000000, 0.5937500000000000000, 0.6015625000000000000, 0.6093750000000000000, 0.6171875000000000000, 0.6250000000000000000, 0.6328125000000000000, 0.6406250000000000000, 0.6484375000000000000, 0.6562500000000000000, 0.6640625000000000000, 0.6718750000000000000, 0.6796875000000000000, 0.6875000000000000000, 0.6953125000000000000, 0.7031250000000000000, 0.7109375000000000000, 0.7187500000000000000, 0.7265625000000000000, 0.7343750000000000000, 0.7421875000000000000, 0.7500000000000000000, 0.7578125000000000000, 0.7656250000000000000, 0.7734375000000000000, 0.7812500000000000000, 0.7890625000000000000, 0.7968750000000000000, 0.8046875000000000000, 0.8125000000000000000, 0.8203125000000000000, 0.8281250000000000000, 0.8359375000000000000, 0.8437500000000000000, 0.8515625000000000000, 0.8593750000000000000, 0.8671875000000000000, 0.8750000000000000000, 0.8828125000000000000, 0.8906250000000000000, 0.8984375000000000000, 0.9062500000000000000, 0.9140625000000000000, 0.9218750000000000000, 0.9296875000000000000, 0.9375000000000000000, 0.9453125000000000000, 0.9531250000000000000, 0.9609375000000000000, 0.9687500000000000000, 0.9765625000000000000, 0.9843750000000000000, 0.9921875000000000000, 1.000000000000000000 ),
 .UNSPECIFIED. ) 
 GEOMETRIC_REPRESENTATION_ITEM ( )  RATIONAL_B_SPLINE_SURFACE ( (
 ( 1.000000000000000000, 0.9238795325112869605, 1.000000000000000000, 0.9238795325112869605, 1.000000000000000000, 0.9238795325112869605, 1.000000000000000000, 0.9238795325112869605, 1.000000000000000000, 0.9238795325112869605, 1.000000000000000000, 0.9238795325112869605, 1.000000000000000000, 0.9238795325112869605, 1.000000000000000000, 0.9238795325112869605, 1.000000000000000000, 0.9238795325112869605, 1.000000000000000000, 0.9238795325112869605, 1.000000000000000000, 0.9238795325112869605, 1.000000000000000000, 0.9238795325112869605, 1.000000000000000000, 0.9238795325112869605, 1.000000000000000000, 0.9238795325112869605, 1.000000000000000000, 0.9238795325112869605, 1.000000000000000000, 0.9238795325112869605, 1.000000000000000000, 0.9238795325112869605, 1.000000000000000000, 0.9238795325112869605, 1.000000000000000000, 0.9238795325112869605, 1.000000000000000000, 0.9238795325112869605, 1.000000000000000000, 0.9238795325112869605, 1.000000000000000000, 0.9238795325112869605, 1.000000000000000000, 0.9238795325112869605, 1.000000000000000000, 0.9238795325112869605, 1.000000000000000000, 0.9238795325112869605, 1.000000000000000000, 0.9238795325112869605, 1.000000000000000000, 0.9238795325112869605, 1.000000000000000000, 0.9238795325112869605, 1.000000000000000000, 0.9238795325112869605, 1.000000000000000000, 0.9238795325112869605, 1.000000000000000000, 0.9238795325112869605, 1.000000000000000000, 0.9238795325112869605, 1.000000000000000000, 0.9238795325112869605, 1.000000000000000000, 0.9238795325112869605, 1.000000000000000000, 0.9238795325112869605, 1.000000000000000000, 0.9238795325112869605, 1.000000000000000000, 0.9238795325112869605, 1.000000000000000000, 0.9238795325112869605, 1.000000000000000000, 0.9238795325112869605, 1.000000000000000000, 0.9238795325112869605, 1.000000000000000000, 0.9238795325112869605, 1.000000000000000000, 0.9238795325112869605, 1.000000000000000000, 0.9238795325112869605, 1.000000000000000000, 0.9238795325112869605, 1.000000000000000000, 0.9238795325112869605, 1.000000000000000000, 0.9238795325112869605, 1.000000000000000000, 0.9238795325112869605, 1.000000000000000000, 0.9238795325112869605, 1.000000000000000000, 0.9238795325112869605, 1.000000000000000000, 0.9238795325112869605, 1.000000000000000000, 0.9238795325112869605, 1.000000000000000000, 0.9238795325112869605, 1.000000000000000000, 0.9238795325112869605, 1.000000000000000000, 0.9238795325112869605, 1.000000000000000000, 0.9238795325112869605, 1.000000000000000000, 0.9238795325112869605, 1.000000000000000000, 0.9238795325112869605, 1.000000000000000000, 0.9238795325112869605, 1.000000000000000000, 0.9238795325112869605, 1.000000000000000000, 0.9238795325112869605, 1.000000000000000000, 0.9238795325112869605, 1.000000000000000000, 0.9238795325112869605, 1.000000000000000000, 0.9238795325112869605, 1.000000000000000000, 0.9238795325112869605, 1.000000000000000000, 0.9238795325112869605, 1.000000000000000000, 0.9238795325112869605, 1.000000000000000000, 0.9238795325112869605, 1.000000000000000000, 0.9238795325112869605, 1.000000000000000000, 0.9238795325112869605, 1.000000000000000000, 0.9238795325112869605, 1.000000000000000000, 0.9238795325112869605, 1.000000000000000000, 0.9238795325112869605, 1.000000000000000000, 0.9238795325112869605, 1.000000000000000000, 0.9238795325112869605, 1.000000000000000000, 0.9238795325112869605, 1.000000000000000000, 0.9238795325112869605, 1.000000000000000000, 0.9238795325112869605, 1.000000000000000000, 0.9238795325112869605, 1.000000000000000000, 0.9238795325112869605, 1.000000000000000000, 0.9238795325112869605, 1.000000000000000000, 0.9238795325112869605, 1.000000000000000000, 0.9238795325112869605, 1.000000000000000000, 0.9238795325112869605, 1.000000000000000000, 0.9238795325112869605, 1.000000000000000000, 0.9238795325112869605, 1.000000000000000000, 0.9238795325112869605, 1.000000000000000000, 0.9238795325112869605, 1.000000000000000000, 0.9238795325112869605, 1.000000000000000000, 0.9238795325112869605, 1.000000000000000000, 0.9238795325112869605, 1.000000000000000000, 0.9238795325112869605, 1.000000000000000000, 0.9238795325112869605, 1.000000000000000000, 0.9238795325112869605, 1.000000000000000000, 0.9238795325112869605, 1.000000000000000000, 0.9238795325112869605, 1.000000000000000000, 0.9238795325112869605, 1.000000000000000000, 0.9238795325112869605, 1.000000000000000000, 0.9238795325112869605, 1.000000000000000000, 0.9238795325112869605, 1.000000000000000000, 0.9238795325112869605, 1.000000000000000000, 0.9238795325112869605, 1.000000000000000000, 0.9238795325112869605, 1.000000000000000000, 0.9238795325112869605, 1.000000000000000000, 0.9238795325112869605, 1.000000000000000000, 0.9238795325112869605, 1.000000000000000000, 0.9238795325112869605, 1.000000000000000000, 0.9238795325112869605, 1.000000000000000000, 0.9238795325112869605, 1.000000000000000000, 0.9238795325112869605, 1.000000000000000000, 0.9238795325112869605, 1.000000000000000000, 0.9238795325112869605, 1.000000000000000000, 0.9238795325112869605, 1.000000000000000000, 0.9238795325112869605, 1.000000000000000000, 0.9238795325112869605, 1.000000000000000000, 0.9238795325112869605, 1.000000000000000000, 0.9238795325112869605, 1.000000000000000000, 0.9238795325112869605, 1.000000000000000000, 0.9238795325112869605, 1.000000000000000000, 0.9238795325112869605, 1.000000000000000000, 0.9238795325112869605, 1.000000000000000000, 0.9238795325112869605, 1.000000000000000000, 0.9238795325112869605, 1.000000000000000000, 0.9238795325112869605, 1.000000000000000000, 0.9238795325112869605, 1.000000000000000000, 0.9238795325112869605, 1.000000000000000000, 0.9238795325112869605, 1.000000000000000000, 0.9238795325112869605, 1.000000000000000000, 0.9238795325112869605, 1.000000000000000000),
 ( 1.000000000000000000, 0.9238795325112869605, 1.000000000000000000, 0.9238795325112869605, 1.000000000000000000, 0.9238795325112869605, 1.000000000000000000, 0.9238795325112869605, 1.000000000000000000, 0.9238795325112869605, 1.000000000000000000, 0.9238795325112869605, 1.000000000000000000, 0.9238795325112869605, 1.000000000000000000, 0.9238795325112869605, 1.000000000000000000, 0.9238795325112869605, 1.000000000000000000, 0.9238795325112869605, 1.000000000000000000, 0.9238795325112869605, 1.000000000000000000, 0.9238795325112869605, 1.000000000000000000, 0.9238795325112869605, 1.000000000000000000, 0.9238795325112869605, 1.000000000000000000, 0.9238795325112869605, 1.000000000000000000, 0.9238795325112869605, 1.000000000000000000, 0.9238795325112869605, 1.000000000000000000, 0.9238795325112869605, 1.000000000000000000, 0.9238795325112869605, 1.000000000000000000, 0.9238795325112869605, 1.000000000000000000, 0.9238795325112869605, 1.000000000000000000, 0.9238795325112869605, 1.000000000000000000, 0.9238795325112869605, 1.000000000000000000, 0.9238795325112869605, 1.000000000000000000, 0.9238795325112869605, 1.000000000000000000, 0.9238795325112869605, 1.000000000000000000, 0.9238795325112869605, 1.000000000000000000, 0.9238795325112869605, 1.000000000000000000, 0.9238795325112869605, 1.000000000000000000, 0.9238795325112869605, 1.000000000000000000, 0.9238795325112869605, 1.000000000000000000, 0.9238795325112869605, 1.000000000000000000, 0.9238795325112869605, 1.000000000000000000, 0.9238795325112869605, 1.000000000000000000, 0.9238795325112869605, 1.000000000000000000, 0.9238795325112869605, 1.000000000000000000, 0.9238795325112869605, 1.000000000000000000, 0.9238795325112869605, 1.000000000000000000, 0.9238795325112869605, 1.000000000000000000, 0.9238795325112869605, 1.000000000000000000, 0.9238795325112869605, 1.000000000000000000, 0.9238795325112869605, 1.000000000000000000, 0.9238795325112869605, 1.000000000000000000, 0.9238795325112869605, 1.000000000000000000, 0.9238795325112869605, 1.000000000000000000, 0.9238795325112869605, 1.000000000000000000, 0.9238795325112869605, 1.000000000000000000, 0.9238795325112869605, 1.000000000000000000, 0.9238795325112869605, 1.000000000000000000, 0.9238795325112869605, 1.000000000000000000, 0.9238795325112869605, 1.000000000000000000, 0.9238795325112869605, 1.000000000000000000, 0.9238795325112869605, 1.000000000000000000, 0.9238795325112869605, 1.000000000000000000, 0.9238795325112869605, 1.000000000000000000, 0.9238795325112869605, 1.000000000000000000, 0.9238795325112869605, 1.000000000000000000, 0.9238795325112869605, 1.000000000000000000, 0.9238795325112869605, 1.000000000000000000, 0.9238795325112869605, 1.000000000000000000, 0.9238795325112869605, 1.000000000000000000, 0.9238795325112869605, 1.000000000000000000, 0.9238795325112869605, 1.000000000000000000, 0.9238795325112869605, 1.000000000000000000, 0.9238795325112869605, 1.000000000000000000, 0.9238795325112869605, 1.000000000000000000, 0.9238795325112869605, 1.000000000000000000, 0.9238795325112869605, 1.000000000000000000, 0.9238795325112869605, 1.000000000000000000, 0.9238795325112869605, 1.000000000000000000, 0.9238795325112869605, 1.000000000000000000, 0.9238795325112869605, 1.000000000000000000, 0.9238795325112869605, 1.000000000000000000, 0.9238795325112869605, 1.000000000000000000, 0.9238795325112869605, 1.000000000000000000, 0.9238795325112869605, 1.000000000000000000, 0.9238795325112869605, 1.000000000000000000, 0.9238795325112869605, 1.000000000000000000, 0.9238795325112869605, 1.000000000000000000, 0.9238795325112869605, 1.000000000000000000, 0.9238795325112869605, 1.000000000000000000, 0.9238795325112869605, 1.000000000000000000, 0.9238795325112869605, 1.000000000000000000, 0.9238795325112869605, 1.000000000000000000, 0.9238795325112869605, 1.000000000000000000, 0.9238795325112869605, 1.000000000000000000, 0.9238795325112869605, 1.000000000000000000, 0.9238795325112869605, 1.000000000000000000, 0.9238795325112869605, 1.000000000000000000, 0.9238795325112869605, 1.000000000000000000, 0.9238795325112869605, 1.000000000000000000, 0.9238795325112869605, 1.000000000000000000, 0.9238795325112869605, 1.000000000000000000, 0.9238795325112869605, 1.000000000000000000, 0.9238795325112869605, 1.000000000000000000, 0.9238795325112869605, 1.000000000000000000, 0.9238795325112869605, 1.000000000000000000, 0.9238795325112869605, 1.000000000000000000, 0.9238795325112869605, 1.000000000000000000, 0.9238795325112869605, 1.000000000000000000, 0.9238795325112869605, 1.000000000000000000, 0.9238795325112869605, 1.000000000000000000, 0.9238795325112869605, 1.000000000000000000, 0.9238795325112869605, 1.000000000000000000, 0.9238795325112869605, 1.000000000000000000, 0.9238795325112869605, 1.000000000000000000, 0.9238795325112869605, 1.000000000000000000, 0.9238795325112869605, 1.000000000000000000, 0.9238795325112869605, 1.000000000000000000, 0.9238795325112869605, 1.000000000000000000, 0.9238795325112869605, 1.000000000000000000, 0.9238795325112869605, 1.000000000000000000, 0.9238795325112869605, 1.000000000000000000, 0.9238795325112869605, 1.000000000000000000, 0.9238795325112869605, 1.000000000000000000, 0.9238795325112869605, 1.000000000000000000, 0.9238795325112869605, 1.000000000000000000, 0.9238795325112869605, 1.000000000000000000, 0.9238795325112869605, 1.000000000000000000, 0.9238795325112869605, 1.000000000000000000, 0.9238795325112869605, 1.000000000000000000, 0.9238795325112869605, 1.000000000000000000, 0.9238795325112869605, 1.000000000000000000, 0.9238795325112869605, 1.000000000000000000, 0.9238795325112869605, 1.000000000000000000, 0.9238795325112869605, 1.000000000000000000, 0.9238795325112869605, 1.000000000000000000, 0.9238795325112869605, 1.000000000000000000) ) ) 
 REPRESENTATION_ITEM ( '' )  SURFACE ( )  );
#4850 = CARTESIAN_POINT ( 'NONE',  ( 122.5532481442453019, 0.4262465694468514643, -12.03445270309931736 ) ) ;
#4851 = DIRECTION ( 'NONE',  ( 0.9908103287288504424, -0.1352586133457952533, 0.000000000000000000 ) ) ;
#4852 = ORIENTED_EDGE ( 'NONE', *, *, #44578, .F. ) ;
#4853 = CARTESIAN_POINT ( 'NONE',  ( 121.6456214775786293, 0.4262465694468514643, -12.03445270309931736 ) ) ;
#4854 = CARTESIAN_POINT ( 'NONE',  ( 124.4819548109119722, -2.084020599724406786, -8.691656652584148546 ) ) ;
#4855 = CARTESIAN_POINT ( 'NONE',  ( 27.78057335388972504, -13.48551096636548330, -19.39321520033831447 ) ) ;
#4856 = DIRECTION ( 'NONE',  ( 0.000000000000000000, -0.3818493186865936084, 0.9242245927363024194 ) ) ;
#4857 = FACE_OUTER_BOUND ( 'NONE', #6650, .T. ) ;
#4858 = CARTESIAN_POINT ( 'NONE',  ( 119.2063748109119814, -1.561330072975668504, -17.79121239304076951 ) ) ;
#4859 = ORIENTED_EDGE ( 'NONE', *, *, #8994, .F. ) ;
#4860 = CARTESIAN_POINT ( 'NONE',  ( 121.5888948109119809, -10.30919188438810075, -12.61870101168855918 ) ) ;
#4861 = CARTESIAN_POINT ( 'NONE',  ( 63.16139403827867937, -37.76446527787062735, -4.964738833969116527 ) ) ;
#4862 = CARTESIAN_POINT ( 'NONE',  ( 107.9822546295247889, -4.863998795839590272, -7.631215200338315796 ) ) ;
#4863 = CARTESIAN_POINT ( 'NONE',  ( 115.5191414775786569, -3.383040157471821630, -19.15922257007629170 ) ) ;
#4864 = CARTESIAN_POINT ( 'NONE',  ( 116.4267681442453153, -3.383040157471821630, -19.15922257007629170 ) ) ;
#4865 = DIRECTION ( 'NONE',  ( -0.5735764363510446051, 0.3127926500124816878, -0.7570804645221042017 ) ) ;
#4866 = CARTESIAN_POINT ( 'NONE',  ( 117.2294421295247844, -10.76310523276723785, -5.182735500338556456 ) ) ;
#4867 = CARTESIAN_POINT ( 'NONE',  ( 91.38554522942851577, -25.99489077589524300, -13.39321520033831625 ) ) ;
#4868 = CIRCLE ( 'NONE', #32525, 1.610000000000000986 ) ;
#4869 = EDGE_LOOP ( 'NONE', ( #19071, #18537, #13713, #22784 ) ) ;
#4870 = CARTESIAN_POINT ( 'NONE',  ( 121.6307382662982945, -6.118135741080345191, -18.48796566952144005 ) ) ;
#4871 = CARTESIAN_POINT ( 'NONE',  ( 109.2294420847119625, -10.34908636181675412, -14.14639072714987833 ) ) ;
#4872 = CARTESIAN_POINT ( 'NONE',  ( 122.0427081442452817, -9.859900752359378018, -12.68260735090039759 ) ) ;
#4873 = CARTESIAN_POINT ( 'NONE',  ( 110.6214733795247867, -1.325403438956436419, -9.854619843455211026 ) ) ;
#4874 = CARTESIAN_POINT ( 'NONE',  ( 107.0793640045248196, -10.62599879583958717, -11.00651665394454604 ) ) ;
#4875 = CARTESIAN_POINT ( 'NONE',  ( 116.0296814775786345, -1.833838273342658809, -17.42832698103878286 ) ) ;
#4876 = CARTESIAN_POINT ( 'NONE',  ( 88.35093386163799778, -24.14644159042263993, -12.62951656296512937 ) ) ;
#4877 = CARTESIAN_POINT ( 'NONE',  ( 126.1270281442452870, -10.30919188438810075, -12.61870101168855918 ) ) ;
#4878 = CARTESIAN_POINT ( 'NONE',  ( 118.3554748109119998, 0.2603800115204892296, -16.42320221600525088 ) ) ;
#4879 = VERTEX_POINT ( 'NONE', #38972 ) ;
#4880 = COLOUR_RGB ( '',0.7921568627450980005, 0.8196078431372548767, 0.9333333333333333481 ) ;
#4881 = CARTESIAN_POINT ( 'NONE',  ( 120.1707281442453166, -9.565557343593413364, -10.61323700422348004 ) ) ;
#4882 = CARTESIAN_POINT ( 'NONE',  ( 113.6471614775786492, -5.638512984488999180, -18.83840828888717311 ) ) ;
#4883 = CARTESIAN_POINT ( 'NONE',  ( 121.7590748109119687, -7.893985811506177619, -18.51759400769804742 ) ) ;
#4884 = CARTESIAN_POINT ( 'NONE',  ( 120.7379948109119709, 0.4262465694468514643, -12.03445270309931736 ) ) ;
#4885 = ORIENTED_EDGE ( 'NONE', *, *, #33887, .T. ) ;
#4886 = CARTESIAN_POINT ( 'NONE',  ( 116.1230435400977825, -1.223627541775731631, -16.99192386690444323 ) ) ;
#4887 = CARTESIAN_POINT ( 'NONE',  ( 119.8870948109119752, -9.261995988541697145, -16.69588392320189030 ) ) ;
#4888 = AXIS2_PLACEMENT_3D ( 'NONE', #2421, #6531, #37304 ) ;
#4889 = DIRECTION ( 'NONE',  ( -0.9609149988134837450, 0.1028163501681639419, -0.2570431154366518145 ) ) ;
#4890 = CARTESIAN_POINT ( 'NONE',  ( 137.5098279454183796, -1.294660118266357296, -16.89733337109311861 ) ) ;
#4891 = CARTESIAN_POINT ( 'NONE',  ( 113.8163171295247764, 0.1403307496149613920, -13.39321520033831447 ) ) ;
#4892 = LINE ( 'NONE', #43891, #29240 ) ;
#4893 = CARTESIAN_POINT ( 'NONE',  ( 94.20708369096698220, -26.09538666226425363, -14.49867541642786861 ) ) ;
#4894 = CARTESIAN_POINT ( 'NONE',  ( 116.4834948109119779, -7.894159318335828068, -9.358103419637847864 ) ) ;
#4895 = CARTESIAN_POINT ( 'NONE',  ( 125.2194014775786286, -10.30919188438810075, -12.61870101168855918 ) ) ;
#4896 = CARTESIAN_POINT ( 'NONE',  ( 90.99708770779186295, -25.23119213852205789, -15.24166438581092109 ) ) ;
#4897 = CARTESIAN_POINT ( 'NONE',  ( 115.9363194150596001, -2.423081321603731020, -17.89265170041263175 ) ) ;
#4898 = CARTESIAN_POINT ( 'NONE',  ( 111.1076452545248259, -9.868328341294098749, -15.46607636864997204 ) ) ;
#4899 = AXIS2_PLACEMENT_3D ( 'NONE', #36805, #11758, #11987 ) ;
#4900 = CARTESIAN_POINT ( 'NONE',  ( 116.8805814775786445, -3.505236298600246325, -18.68346056562440793 ) ) ;
#4901 = CARTESIAN_POINT ( 'NONE',  ( 114.6874464091100947, -0.9924539043446216624, -17.29976612834909133 ) ) ;
#4902 = LINE ( 'NONE', #15174, #8580 ) ;
#4904 = CARTESIAN_POINT ( 'NONE',  ( 120.4543614775786295, -4.089484607189486809, -7.948022111789456723 ) ) ;
#4903 = CARTESIAN_POINT ( 'NONE',  ( 59.75121349346655109, -13.58877957849837692, -7.404803486908546617 ) ) ;
#4905 = CARTESIAN_POINT ( 'NONE',  ( 123.0070614775786169, -10.15424416112533912, -14.75197769757731336 ) ) ;
#4906 = VERTEX_POINT ( 'NONE', #21652 ) ;
#4907 = CARTESIAN_POINT ( 'NONE',  ( 69.51487126532624927, -51.06495315005575719, -31.09787670850536756 ) ) ;
#4908 = CARTESIAN_POINT ( 'NONE',  ( 126.2404814775786264, -9.261995988541697145, -16.69588392320189030 ) ) ;
#4909 = CARTESIAN_POINT ( 'NONE',  ( 108.6073327545248048, -6.936859964151250502, -8.388885654883777576 ) ) ;
#4910 = CARTESIAN_POINT ( 'NONE',  ( 120.9649014775786355, -6.222761293078241884, -8.102969835052219238 ) ) ;
#4911 = EDGE_CURVE ( 'NONE', #11410, #23361, #23047, .T. ) ;
#4912 = CARTESIAN_POINT ( 'NONE',  ( 123.2906948109119867, -1.833838273342659697, -17.42832698103878286 ) ) ;
#4913 = CARTESIAN_POINT ( 'NONE',  ( 117.1074881442453233, 0.4262465694468514643, -12.03445270309931736 ) ) ;
#4914 = CARTESIAN_POINT ( 'NONE',  ( 119.5240753663348556, -1.172797794773259072, -17.05961127468926719 ) ) ;
#4915 = CARTESIAN_POINT ( 'NONE',  ( 108.8851452545248151, 0.8980012041604421569, -11.00651665394454071 ) ) ;
#4916 = CARTESIAN_POINT ( 'NONE',  ( 122.4397948109119767, -0.1624402480850797581, -16.17319339645315424 ) ) ;
#4917 = CARTESIAN_POINT ( 'NONE',  ( 124.6521348109119884, -7.894159318335828068, -9.358103419637847864 ) ) ;
#4918 = FACE_OUTER_BOUND ( 'NONE', #3819, .T. ) ;
#4919 = CARTESIAN_POINT ( 'NONE',  ( 96.54708369096698561, -24.69793907545987466, -15.18364567559777178 ) ) ;
#4920 = CARTESIAN_POINT ( 'NONE',  ( 119.6740016859119748, -0.6942167230862511529, -9.935906262978006609 ) ) ;
#4921 = B_SPLINE_CURVE_WITH_KNOTS ( 'NONE', 3,
 ( #3883, #7984, #8214, #39452, #7762, #36014, #25545, #4783, #8441, #39675 ),
 .UNSPECIFIED., .F., .F.,
 ( 4, 3, 3, 4 ),
 ( 0.000000000000000000, 0.0001671877560958109985, 0.0003343755126086545080, 0.0006438490228507220145 ),
 .UNSPECIFIED. ) ;
#4922 = CARTESIAN_POINT ( 'NONE',  ( 116.1777233795247781, -8.938348069036489818, -17.46756447353520159 ) ) ;
#4923 = CARTESIAN_POINT ( 'NONE',  ( 93.44708369096697709, -22.29799240495002977, -11.86581792559194426 ) ) ;
#4924 = CARTESIAN_POINT ( 'NONE',  ( 83.60368610585459237, -32.46739910898208592, -21.41484521824674658 ) ) ;
#4925 = CARTESIAN_POINT ( 'NONE',  ( 122.6667014775786413, -7.893985811506177619, -18.51759400769804742 ) ) ;
#4926 = CARTESIAN_POINT ( 'NONE',  ( 116.6536748109119941, 0.9020085738987339008, -11.91225656197089222 ) ) ;
#4927 = CARTESIAN_POINT ( 'NONE',  ( 107.0793640045248196, -10.62599879583958717, -11.00651665394454604 ) ) ;
#4928 = CARTESIAN_POINT ( 'NONE',  ( 113.8740681442453138, 0.5811942927096154232, -14.16772938898807155 ) ) ;
#4929 = DIRECTION ( 'NONE',  ( 0.000000000000000000, 0.3818493186865927203, -0.9242245927363029745 ) ) ;
#4930 = ORIENTED_EDGE ( 'NONE', *, *, #14554, .F. ) ;
#4931 = LINE ( 'NONE', #15431, #13790 ) ;
#4932 = CARTESIAN_POINT ( 'NONE',  ( 116.4267681442453153, -3.383040157471821630, -19.15922257007629170 ) ) ;
#4933 = CARTESIAN_POINT ( 'NONE',  ( 126.1837548109119496, 0.4262465694468514643, -12.03445270309931736 ) ) ;
#4934 = DIRECTION ( 'NONE',  ( 0.000000000000000000, 0.000000000000000000, 1.000000000000000000 ) ) ;
#4935 = CARTESIAN_POINT ( 'NONE',  ( 115.6893214775786447, -9.859900752359374465, -12.68260735090039404 ) ) ;
#4936 = CARTESIAN_POINT ( 'NONE',  ( 125.5030348109119558, -3.383040157471821630, -19.15922257007629170 ) ) ;
#4937 = EDGE_CURVE ( 'NONE', #12500, #23757, #18234, .T. ) ;
#4938 = CARTESIAN_POINT ( 'NONE',  ( 111.4549108795247747, -8.938348069036489818, -9.318865927141430916 ) ) ;
#4939 = CARTESIAN_POINT ( 'NONE',  ( 121.1350814775786233, -9.859900752359378018, -12.68260735090039759 ) ) ;
#4940 = DIRECTION ( 'NONE',  ( 0.000000000000000000, 0.000000000000000000, -1.000000000000000000 ) ) ;
#4941 = DIRECTION ( 'NONE',  ( 0.000000000000000000, -0.3818493186865927203, 0.9242245927363029745 ) ) ;
#4942 = ORIENTED_EDGE ( 'NONE', *, *, #7164, .F. ) ;
#4943 = EDGE_CURVE ( 'NONE', #2128, #10182, #40530, .T. ) ;
#4944 = CARTESIAN_POINT ( 'NONE',  ( 123.9106423109119675, -9.959231468620755479, -10.70263013195267199 ) ) ;
#4945 = ADVANCED_FACE ( 'NONE', ( #28730 ), #4542, .F. ) ;
#4946 = CARTESIAN_POINT ( 'NONE',  ( 119.9438214775786378, -7.893985811506177619, -18.51759400769804742 ) ) ;
#4947 = ORIENTED_EDGE ( 'NONE', *, *, #8308, .T. ) ;
#4948 = CARTESIAN_POINT ( 'NONE',  ( 70.19189222814998175, -70.34019061884472990, -41.33884020749756871 ) ) ;
#4949 = CARTESIAN_POINT ( 'NONE',  ( -13.43092278348643376, -3.953837739881414848, -7.878202387284918728 ) ) ;
#4950 = DIRECTION ( 'NONE',  ( 0.9609149988134837450, -0.1028163501681639419, 0.2570431154366518145 ) ) ;
#4951 = CARTESIAN_POINT ( 'NONE',  ( 118.0718414775786442, -0.8288870151387760510, -10.36305467784173118 ) ) ;
#4952 = DIRECTION ( 'NONE',  ( 1.000000000000000000, 0.000000000000000000, 0.000000000000000000 ) ) ;
#4953 = CARTESIAN_POINT ( 'NONE',  ( 124.5273704333169320, -9.803742449528428438, -12.61775372557454844 ) ) ;
#4954 = CARTESIAN_POINT ( 'NONE',  ( 125.0492214775786266, -3.505236298600246325, -18.68346056562440793 ) ) ;
#4955 = CARTESIAN_POINT ( 'NONE',  ( 70.19189222814998175, -65.04786711941001442, -39.22192925582032785 ) ) ;
#4956 = EDGE_CURVE ( 'NONE', #8943, #2680, #31680, .T. ) ;
#4957 = CARTESIAN_POINT ( 'NONE',  ( 124.2550481442452792, -0.1624402480850797581, -16.17319339645315424 ) ) ;
#4958 = CARTESIAN_POINT ( 'NONE',  ( 124.9868051361382868, -12.36944789948101331, -14.53642012793133986 ) ) ;
#4959 = CARTESIAN_POINT ( 'NONE',  ( 118.2987481442453088, -7.894159318335828068, -9.358103419637847864 ) ) ;
#4960 = CARTESIAN_POINT ( 'NONE',  ( 121.3052614775786111, -7.643976991954077427, -18.09477374809248928 ) ) ;
#4961 = ADVANCED_FACE ( 'NONE', ( #22106 ), #21206, .T. ) ;
#4962 = CARTESIAN_POINT ( 'NONE',  ( 113.7038881442453402, -3.383040157471821630, -19.15922257007629170 ) ) ;
#4963 = CARTESIAN_POINT ( 'NONE',  ( 120.8514481442452961, -7.893985811506177619, -18.51759400769804742 ) ) ;
#4964 = CARTESIAN_POINT ( 'NONE',  ( 114.0442481442453300, -1.834011780172310813, -8.268836392978581529 ) ) ;
#4965 = CARTESIAN_POINT ( 'NONE',  ( 115.8999108795247821, -1.325403438956436419, -16.93181055722141792 ) ) ;
#4966 = ADVANCED_FACE ( 'NONE', ( #21878 ), #1964, .T. ) ;
#4967 = EDGE_CURVE ( 'NONE', #9213, #33021, #15040, .T. ) ;
#4968 = CARTESIAN_POINT ( 'NONE',  ( 124.1415948109119540, -3.505236298600246325, -18.68346056562440793 ) ) ;
#4969 = ORIENTED_EDGE ( 'NONE', *, *, #15053, .F. ) ;
#4970 = CARTESIAN_POINT ( 'NONE',  ( 121.3619881442452879, -4.089484607189486809, -7.948022111789456723 ) ) ;
#4971 = CARTESIAN_POINT ( 'NONE',  ( 115.8304577545247582, -7.250697342233347165, -7.631215200338321125 ) ) ;
#4972 = CARTESIAN_POINT ( 'NONE',  ( 107.2877233795247776, -1.325403438956436419, -9.854619843455211026 ) ) ;
#4973 = CARTESIAN_POINT ( 'NONE',  ( 70.19189222814998175, -65.04786711941002864, -39.22192925581980916 ) ) ;
#4974 = CARTESIAN_POINT ( 'NONE',  ( 113.0798948109119948, -8.899110576539710493, -16.42337572283490132 ) ) ;
#4975 = CARTESIAN_POINT ( 'NONE',  ( 120.2990798109119766, -2.173413727453600508, -8.297982527556802879 ) ) ;
#4976 = CARTESIAN_POINT ( 'NONE',  ( 125.2194014775786286, -10.30919188438810075, -12.61870101168855918 ) ) ;
#4977 = EDGE_LOOP ( 'NONE', ( #14039, #7606, #8265, #14143 ) ) ;
#4978 = CARTESIAN_POINT ( 'NONE',  ( 125.2761281442453054, 0.4262465694468514643, -12.03445270309931736 ) ) ;
#4979 = DIRECTION ( 'NONE',  ( 0.000000000000000000, 0.000000000000000000, 1.000000000000000000 ) ) ;
#4980 = CARTESIAN_POINT ( 'NONE',  ( 120.9241579359119925, -5.444069387712269226, -19.60292469916370450 ) ) ;
#4981 = LINE ( 'NONE', #22759, #37743 ) ;
#4982 = CARTESIAN_POINT ( 'NONE',  ( 107.0793640045248196, 0.1403307496149616695, -15.46607636864997204 ) ) ;
#4983 = EDGE_LOOP ( 'NONE', ( #33509, #43895, #4007, #12481 ) ) ;
#4984 = CARTESIAN_POINT ( 'NONE',  ( 116.3700414775786527, -5.638512984488999180, -18.83840828888717311 ) ) ;
#4985 = CARTESIAN_POINT ( 'NONE',  ( 125.2761281442453054, -10.63000616557722466, -14.87417383870573495 ) ) ;
#4986 = CARTESIAN_POINT ( 'NONE',  ( 121.1350814775786233, -9.859900752359378018, -12.68260735090039759 ) ) ;
#4987 = CARTESIAN_POINT ( 'NONE',  ( 113.5337081442453240, -0.8288870151387760510, -10.36305467784173118 ) ) ;
#4988 = SURFACE_STYLE_FILL_AREA ( #895 ) ;
#4989 = CARTESIAN_POINT ( 'NONE',  ( 90.72400676789006013, -25.38011337280982715, -14.88121679464376257 ) ) ;
#4990 = CARTESIAN_POINT ( 'NONE',  ( 123.8119224739651969, 0.3208234527006275094, -15.99825685930878194 ) ) ;
#4991 = CARTESIAN_POINT ( 'NONE',  ( 112.0020881442453344, 0.2603800115204892296, -16.42320221600525088 ) ) ;
#4992 = ORIENTED_EDGE ( 'NONE', *, *, #41240, .T. ) ;
#4993 = CARTESIAN_POINT ( 'NONE',  ( 116.5944421295247793, -9.868328341294093420, -13.39321520033831447 ) ) ;
#4994 = CARTESIAN_POINT ( 'NONE',  ( 123.0637881442452937, -0.4660016031367893996, -10.09054647747474043 ) ) ;
#4995 = CARTESIAN_POINT ( 'NONE',  ( 136.8611794030194346, -9.932755188769407440, -15.66772631836134444 ) ) ;
#4996 = ORIENTED_EDGE ( 'NONE', *, *, #17087, .F. ) ;
#4997 = CARTESIAN_POINT ( 'NONE',  ( 114.2144281442453178, -8.166667518702817929, -8.995218007635859436 ) ) ;
#4998 = CARTESIAN_POINT ( 'NONE',  ( 124.4252281442452812, -9.261995988541697145, -16.69588392320189030 ) ) ;
#4999 = DIRECTION ( 'NONE',  ( -0.2768435750659253847, -0.3568721902840677473, 0.8921882507333133150 ) ) ;
#5000 = EDGE_CURVE ( 'NONE', #25709, #35629, #41968, .T. ) ;
#5001 = CARTESIAN_POINT ( 'NONE',  ( 125.1626748109119802, -0.1624402480850797581, -16.17319339645315424 ) ) ;
#5002 = ORIENTED_EDGE ( 'NONE', *, *, #8299, .F. ) ;
#5003 = CARTESIAN_POINT ( 'NONE',  ( 116.8238548109119819, -4.089484607189486809, -7.948022111789456723 ) ) ;
#5004 = CARTESIAN_POINT ( 'NONE',  ( 90.06246830635160450, -25.99489077589524300, -13.39321520033831625 ) ) ;
#5005 = CARTESIAN_POINT ( 'NONE',  ( 109.7185827545248600, -6.936859964151250502, -8.388885654883788234 ) ) ;
#5006 = DIRECTION ( 'NONE',  ( -1.000000000000000000, 0.000000000000000000, 0.000000000000000000 ) ) ;
#5007 = CARTESIAN_POINT ( 'NONE',  ( 111.4630944056972623, -2.471736349583551817, -17.82786025615278191 ) ) ;
#5008 = CARTESIAN_POINT ( 'NONE',  ( 115.6325948109119821, -9.565557343593413364, -10.61323700422348004 ) ) ;
#5009 = CARTESIAN_POINT ( 'NONE',  ( 86.36631847702263087, -25.99489077589524300, -13.39321520033831447 ) ) ;
#5010 = CIRCLE ( 'NONE', #2842, 1.610000000000000986 ) ;
#5011 = CARTESIAN_POINT ( 'NONE',  ( 125.3046178784917828, -3.279438446396415241, -20.37743778007813233 ) ) ;
#5012 = CARTESIAN_POINT ( 'NONE',  ( 113.5904348109119866, -2.084020599724406786, -8.691656652584148546 ) ) ;
#5013 = CARTESIAN_POINT ( 'NONE',  ( 112.1155414775786454, 0.9020085738987339008, -11.91225656197089222 ) ) ;
#5014 = CARTESIAN_POINT ( 'NONE',  ( 116.6368254076533759, -9.513716847284458211, -15.34440693972388559 ) ) ;
#5015 = CARTESIAN_POINT ( 'NONE',  ( 124.8223148109119762, -10.15424416112533912, -14.75197769757731336 ) ) ;
#5016 = CARTESIAN_POINT ( 'NONE',  ( 112.9664414775786412, -9.859900752359374465, -12.68260735090039404 ) ) ;
#5017 = CARTESIAN_POINT ( 'NONE',  ( 118.2987481442453088, -1.561330072975668504, -17.79121239304076951 ) ) ;
#5018 = EDGE_CURVE ( 'NONE', #23812, #3754, #32809, .T. ) ;
#5019 = CARTESIAN_POINT ( 'NONE',  ( 120.9081748109119872, -5.638512984488999180, -18.83840828888717311 ) ) ;
#5020 = ORIENTED_EDGE ( 'NONE', *, *, #28401, .T. ) ;
#5021 = CARTESIAN_POINT ( 'NONE',  ( 114.6032811052981941, 0.4930828106259610433, -12.14321520033831625 ) ) ;
#5022 = CARTESIAN_POINT ( 'NONE',  ( 114.4413952545248350, 0.8980012041604421569, -11.00651665394454071 ) ) ;
#5023 = CARTESIAN_POINT ( 'NONE',  ( 111.3854577545248645, -2.791137627527939813, -18.39754474579286025 ) ) ;
#5024 = CARTESIAN_POINT ( 'NONE',  ( 110.9687390045248350, -9.868328341294098749, -11.32035403202665869 ) ) ;
#5025 = ADVANCED_FACE ( 'NONE', ( #22120 ), #12540, .T. ) ;
#5026 = CARTESIAN_POINT ( 'NONE',  ( 126.4262034846940708, -9.811855180994648151, -12.14055829856050472 ) ) ;
#5027 = CARTESIAN_POINT ( 'NONE',  ( 114.8951481442453115, -0.4660016031367893996, -10.09054647747474043 ) ) ;
#5028 = ORIENTED_EDGE ( 'NONE', *, *, #4213, .T. ) ;
#5029 = CARTESIAN_POINT ( 'NONE',  ( 106.5237390045248418, 0.8980012041604421569, -15.77991374673208469 ) ) ;
#5030 = CARTESIAN_POINT ( 'NONE',  ( 119.3198281442452924, -9.859900752359374465, -12.68260735090039404 ) ) ;
#5031 = ADVANCED_FACE ( 'NONE', ( #15274 ), #1361, .T. ) ;
#5032 = CARTESIAN_POINT ( 'NONE',  ( 77.05532149770296257, 0.06670422450934243574, -8.143215200338314474 ) ) ;
#5033 = CARTESIAN_POINT ( 'NONE',  ( 122.6667014775786413, -2.084020599724391687, -8.691656652584152098 ) ) ;
#5034 = CARTESIAN_POINT ( 'NONE',  ( 112.5693548109119888, -10.63000616557722466, -14.87417383870573495 ) ) ;
#5035 = CARTESIAN_POINT ( 'NONE',  ( 119.8870948109119752, -9.261995988541697145, -16.69588392320189030 ) ) ;
#5036 = CARTESIAN_POINT ( 'NONE',  ( 111.7327233795247849, -8.938348069036489818, -17.46756447353520159 ) ) ;
#5037 = CARTESIAN_POINT ( 'NONE',  ( 112.2188952545247531, -9.868328341294098749, -15.46607636864997204 ) ) ;
#5038 = ORIENTED_EDGE ( 'NONE', *, *, #9270, .F. ) ;
#5039 = CARTESIAN_POINT ( 'NONE',  ( 120.9649014775786497, -6.222761293078217903, -8.102969835052215686 ) ) ;
#5040 = CARTESIAN_POINT ( 'NONE',  ( 119.6034614775786196, -3.505236298600246325, -18.68346056562440793 ) ) ;
#5041 = CARTESIAN_POINT ( 'NONE',  ( 117.3343948109119737, -3.383040157471821630, -19.15922257007629170 ) ) ;
#5042 = CARTESIAN_POINT ( 'NONE',  ( 90.45092582798827152, -25.99489077589524300, -13.39321520033831625 ) ) ;
#5043 = DIRECTION ( 'NONE',  ( 0.000000000000000000, -0.3818493186865929978, 0.9242245927363029745 ) ) ;
#5044 = CARTESIAN_POINT ( 'NONE',  ( 121.9292548109119849, -7.894159318335828068, -9.358103419637847864 ) ) ;
#5045 = CARTESIAN_POINT ( 'NONE',  ( 114.2144281442453178, -1.833838273342658809, -17.42832698103878286 ) ) ;
#5046 = VERTEX_POINT ( 'NONE', #25994 ) ;
#5047 = CARTESIAN_POINT ( 'NONE',  ( 119.8823610609119754, -3.163656168406935087, -18.89861972220014508 ) ) ;
#5048 = VECTOR ( 'NONE', #24433, 1000.000000000000000 ) ;
#5049 = CARTESIAN_POINT ( 'NONE',  ( 113.3992004682427819, 0.5115630086001619059, -14.64321520033833401 ) ) ;
#5050 = CARTESIAN_POINT ( 'NONE',  ( 117.2209414775786485, -2.084020599724406786, -8.691656652584148546 ) ) ;
#5051 = ORIENTED_EDGE ( 'NONE', *, *, #10574, .T. ) ;
#5052 = AXIS2_PLACEMENT_3D ( 'NONE', #32669, #15359, #18998 ) ;
#5053 = FACE_OUTER_BOUND ( 'NONE', #30142, .T. ) ;
#5054 = CARTESIAN_POINT ( 'NONE',  ( 115.6325948109119821, 0.2603800115204892296, -16.42320221600525088 ) ) ;
#5055 = CARTESIAN_POINT ( 'NONE',  ( 107.4960827545248350, -6.936859964151250502, -8.388885654883777576 ) ) ;
#5056 = CARTESIAN_POINT ( 'NONE',  ( 112.5126281442453120, 0.1319031606808879209, -14.10382304977623669 ) ) ;
#5057 = ORIENTED_EDGE ( 'NONE', *, *, #16967, .T. ) ;
#5058 = VERTEX_POINT ( 'NONE', #43775 ) ;
#5059 = CARTESIAN_POINT ( 'NONE',  ( 122.6099748109119929, -0.8288870151387760510, -10.36305467784173118 ) ) ;
#5060 = CARTESIAN_POINT ( 'NONE',  ( 118.0151148109119816, 0.4262465694468514643, -12.03445270309931736 ) ) ;
#5061 = EDGE_CURVE ( 'NONE', #32385, #9071, #1912, .T. ) ;
#5062 = ORIENTED_EDGE ( 'NONE', *, *, #42087, .T. ) ;
#5063 = DIRECTION ( 'NONE',  ( 0.000000000000000000, -0.4669533266896290225, -0.8842819633428516957 ) ) ;
#5064 = CARTESIAN_POINT ( 'NONE',  ( 62.64709028481676967, -64.81681335280190126, -45.78210799152465427 ) ) ;
#5065 = CARTESIAN_POINT ( 'NONE',  ( 107.9822546295247889, -4.863998795839590272, -7.631215200338315796 ) ) ;
#5066 = CARTESIAN_POINT ( 'NONE',  ( 114.6115148109119986, -3.383040157471821630, -19.15922257007629170 ) ) ;
#5068 = CARTESIAN_POINT ( 'NONE',  ( 115.9162281442453235, -5.574606645277164318, -18.38911715685844683 ) ) ;
#5067 = CARTESIAN_POINT ( 'NONE',  ( 113.5904348109119866, -7.893985811506177619, -18.51759400769804742 ) ) ;
#5069 = CARTESIAN_POINT ( 'NONE',  ( 121.2485348109119769, -8.899110576539710493, -16.42337572283490132 ) ) ;
#5070 = CYLINDRICAL_SURFACE ( 'NONE', #2925, 35.00000000000000711 ) ;
#5071 = EDGE_LOOP ( 'NONE', ( #42487, #7890, #19368, #16058 ) ) ;
#5072 = CARTESIAN_POINT ( 'NONE',  ( 119.2063748109119814, -7.894159318335828068, -9.358103419637847864 ) ) ;
#5073 = CARTESIAN_POINT ( 'NONE',  ( 123.6310548109119765, -4.153390946401325223, -8.397313243818185668 ) ) ;
#5074 = CARTESIAN_POINT ( 'NONE',  ( 113.2606921295247702, 0.8980012041604618078, -13.39321520033831447 ) ) ;
#5075 = CARTESIAN_POINT ( 'NONE',  ( 115.8999108795247821, -1.325403438956436419, -16.93181055722141792 ) ) ;
#5076 = CARTESIAN_POINT ( 'NONE',  ( 110.4825671295247815, -10.62599879583958540, -13.39321520033831447 ) ) ;
#5077 = EDGE_CURVE ( 'NONE', #29714, #43791, #36116, .T. ) ;
#5078 = AXIS2_PLACEMENT_3D ( 'NONE', #10710, #38277, #24831 ) ;
#5079 = CARTESIAN_POINT ( 'NONE',  ( 120.0005481442453146, -5.638512984488999180, -18.83840828888717311 ) ) ;
#5080 = VERTEX_POINT ( 'NONE', #30089 ) ;
#5081 = CARTESIAN_POINT ( 'NONE',  ( 122.3263414775786373, -6.344957434206665248, -7.627207830600338134 ) ) ;
#5082 = CARTESIAN_POINT ( 'NONE',  ( 62.74100695445530818, -37.51187114369871978, -5.133703732075733939 ) ) ;
#5083 = CARTESIAN_POINT ( 'NONE',  ( 105.8292077545248446, -7.250697342233347165, -7.631215200338321125 ) ) ;
#5084 = CARTESIAN_POINT ( 'NONE',  ( 114.8951481442453115, -0.4660016031367893996, -10.09054647747474043 ) ) ;
#5085 = CARTESIAN_POINT ( 'NONE',  ( 117.5613014775786525, 0.9020085738987339008, -11.91225656197089222 ) ) ;
#5086 = CARTESIAN_POINT ( 'NONE',  ( 67.69800074041313565, -1.521566938544754999, -16.82025522485820446 ) ) ;
#5087 = CARTESIAN_POINT ( 'NONE',  ( 117.1518534370333811, -11.20570961459246107, -5.509241833875157646 ) ) ;
#5088 = ORIENTED_EDGE ( 'NONE', *, *, #19492, .F. ) ;
#5089 = PLANE ( 'NONE',  #32480 ) ;
#5090 = CARTESIAN_POINT ( 'NONE',  ( 109.2294604103198452, -10.11295469467371966, -11.27150632045694323 ) ) ;
#5091 = CARTESIAN_POINT ( 'NONE',  ( 120.4543614775786295, -5.574606645277164318, -18.38911715685844683 ) ) ;
#5092 = CARTESIAN_POINT ( 'NONE',  ( 110.3436608795247764, -1.325403438956436419, -16.93181055722141792 ) ) ;
#5093 = CARTESIAN_POINT ( 'NONE',  ( 115.8304577545247582, -2.791137627527939813, -18.39754474579286025 ) ) ;
#5094 = AXIS2_PLACEMENT_3D ( 'NONE', #44178, #41435, #3551 ) ;
#5095 = CARTESIAN_POINT ( 'NONE',  ( 115.0653281442453277, -3.505236298600246325, -18.68346056562440793 ) ) ;
#5096 = CARTESIAN_POINT ( 'NONE',  ( 125.4584548109119737, -7.476587315910852460, -21.06050163197695824 ) ) ;
#5097 = CARTESIAN_POINT ( 'NONE',  ( 71.10462995142283660, -24.78225172292188816, -5.217245182122844938 ) ) ;
#5098 = CARTESIAN_POINT ( 'NONE',  ( 113.1366214775786432, -7.643976991954077427, -18.09477374809248928 ) ) ;
#5099 = CARTESIAN_POINT ( 'NONE',  ( 119.5467348109119712, -4.089484607189486809, -7.948022111789456723 ) ) ;
#5100 = ORIENTED_EDGE ( 'NONE', *, *, #41365, .F. ) ;
#5101 = CARTESIAN_POINT ( 'NONE',  ( 117.0507614775786465, 0.1319031606808879209, -14.10382304977623669 ) ) ;
#5102 = CARTESIAN_POINT ( 'NONE',  ( 115.8595014775786609, -1.834011780172310813, -8.268836392978581529 ) ) ;
#5103 = CARTESIAN_POINT ( 'NONE',  ( 122.8936081442453059, 0.2603800115204892296, -16.42320221600525088 ) ) ;
#5104 = CARTESIAN_POINT ( 'NONE',  ( 121.1350814775786233, -9.859900752359378018, -12.68260735090039759 ) ) ;
#5105 = ORIENTED_EDGE ( 'NONE', *, *, #17516, .T. ) ;
#5106 = CARTESIAN_POINT ( 'NONE',  ( 125.3895814775786448, -2.084020599724406786, -8.691656652584148546 ) ) ;
#5107 = CARTESIAN_POINT ( 'NONE',  ( 119.3198281442452924, 0.5811942927096110934, -14.16772938898807510 ) ) ;
#5108 = AXIS2_PLACEMENT_3D ( 'NONE', #3903, #14855, #17821 ) ;
#5109 = CARTESIAN_POINT ( 'NONE',  ( 123.9584548109119737, -8.523281198020143279, -6.279169073056789507 ) ) ;
#5110 = CARTESIAN_POINT ( 'NONE',  ( 122.3263414775786373, -6.344957434206665248, -7.627207830600338134 ) ) ;
#5111 =( BOUNDED_CURVE ( )  B_SPLINE_CURVE ( 2, ( #45144, #21633, #4062, #25287, #17987, #35061, #31886, #28036, #13901, #27808, #38492, #39181, #7267, #651, #31436, #20966, #41722 ),
 .UNSPECIFIED., .F., .T. ) 
 B_SPLINE_CURVE_WITH_KNOTS ( ( 3, 2, 2, 2, 2, 2, 2, 2, 3 ),
 ( 0.2671282416568590001, 0.2734375000000000000, 0.2812500000000000000, 0.2890625000000000000, 0.2968750000000000000, 0.3046875000000000000, 0.3125000000000000000, 0.3203125000000000000, 0.3266217583431409999 ),
 .UNSPECIFIED. ) 
 CURVE ( )  GEOMETRIC_REPRESENTATION_ITEM ( )  RATIONAL_B_SPLINE_CURVE ( ( 0.9763430640195970289, 0.9385262470928680267, 1.000000000000000000, 0.9238795325112869605, 1.000000000000000000, 0.9238795325112869605, 1.000000000000000000, 0.9238795325112869605, 1.000000000000000000, 0.9238795325112869605, 1.000000000000000000, 0.9238795325112869605, 1.000000000000000000, 0.9238795325112869605, 1.000000000000000000, 0.9385262470928680267, 0.9763430640195970289 ) ) 
 REPRESENTATION_ITEM ( '' )  );
#5112 = CARTESIAN_POINT ( 'NONE',  ( 109.0935046295247872, -4.863998795839590272, -7.631215200338315796 ) ) ;
#5113 = DIRECTION ( 'NONE',  ( 1.000000000000000000, 0.000000000000000000, 0.000000000000000000 ) ) ;
#5114 = CARTESIAN_POINT ( 'NONE',  ( 112.4967077545247633, -2.791137627527939813, -18.39754474579286025 ) ) ;
#5115 = AXIS2_PLACEMENT_3D ( 'NONE', #6288, #20657, #9484 ) ;
#5116 = CARTESIAN_POINT ( 'NONE',  ( 65.52504830115719869, -2.484121567297625788, -16.32284768336232261 ) ) ;
#5117 = VECTOR ( 'NONE', #28975, 1000.000000000000000 ) ;
#5118 = DIRECTION ( 'NONE',  ( -0.000000000000000000, 0.9242245927363027524, 0.3818493186865931643 ) ) ;
#5119 = CARTESIAN_POINT ( 'NONE',  ( 118.8092881442453290, -0.1624402480850797581, -16.17319339645315424 ) ) ;
#5120 = CARTESIAN_POINT ( 'NONE',  ( 123.9714148109119805, -0.4660016031367893996, -10.09054647747474043 ) ) ;
#5121 = FACE_OUTER_BOUND ( 'NONE', #34239, .T. ) ;
#5122 = ORIENTED_EDGE ( 'NONE', *, *, #26712, .F. ) ;
#5123 = CARTESIAN_POINT ( 'NONE',  ( 116.4587108795247730, -8.399532701772287169, -9.857681294405580275 ) ) ;
#5124 = CARTESIAN_POINT ( 'NONE',  ( 111.1770983795247787, -8.402594152722688392, -16.93181055722141792 ) ) ;
#5125 = CARTESIAN_POINT ( 'NONE',  ( 116.0296814775786345, -1.833838273342658809, -17.42832698103878286 ) ) ;
#5126 = CARTESIAN_POINT ( 'NONE',  ( 126.2184548109119788, -1.295815253274133161, -16.89579513612386563 ) ) ;
#5127 = DIRECTION ( 'NONE',  ( 0.000000000000000000, 0.000000000000000000, -1.000000000000000000 ) ) ;
#5128 = CARTESIAN_POINT ( 'NONE',  ( -2.055500662264778011, -6.901212958611610659, -18.95048905933739292 ) ) ;
#5130 = CARTESIAN_POINT ( 'NONE',  ( 121.5888948109119809, -10.30919188438810075, -12.61870101168855918 ) ) ;
#5129 = CARTESIAN_POINT ( 'NONE',  ( 63.13224612813447578, -13.41522658373937915, -8.141029825667127184 ) ) ;
#5131 = ADVANCED_FACE ( 'NONE', ( #29860 ), #13593, .T. ) ;
#5132 = CARTESIAN_POINT ( 'NONE',  ( 122.8936081442453059, -9.565557343593413364, -10.61323700422348004 ) ) ;
#5133 = EDGE_LOOP ( 'NONE', ( #40422, #35648, #18943, #41192 ) ) ;
#5134 = CARTESIAN_POINT ( 'NONE',  ( 110.2486464071292858, 0.2518737723193609224, -14.64321520033833934 ) ) ;
#5135 = CARTESIAN_POINT ( 'NONE',  ( 125.6732148109119862, 0.5811942927096110934, -14.16772938898807510 ) ) ;
#5136 = CARTESIAN_POINT ( 'NONE',  ( 108.6767858795247861, -8.402594152722688392, -9.854619843455216355 ) ) ;
#5137 = CARTESIAN_POINT ( 'NONE',  ( 122.3830681442452857, -1.833838273342659697, -17.42832698103878286 ) ) ;
#5138 = CARTESIAN_POINT ( 'NONE',  ( 123.3474214775786209, -0.1624402480850797581, -16.17319339645315424 ) ) ;
#5139 = CARTESIAN_POINT ( 'NONE',  ( 116.0864081442453113, -0.1624402480850797581, -16.17319339645315424 ) ) ;
#5140 = CARTESIAN_POINT ( 'NONE',  ( 70.19189222814998175, -62.26243369865490251, -38.10776559704283528 ) ) ;
#5141 = CARTESIAN_POINT ( 'NONE',  ( 106.8015515045248378, -2.477300249445798297, -7.631215200338321125 ) ) ;
#5142 = CARTESIAN_POINT ( 'NONE',  ( 125.0492214775786266, -3.505236298600246325, -18.68346056562440793 ) ) ;
#5143 = CARTESIAN_POINT ( 'NONE',  ( 122.4397948109119767, -0.1624402480850797581, -16.17319339645315424 ) ) ;
#5144 = DIRECTION ( 'NONE',  ( -1.000000000000000000, 0.000000000000000000, 0.000000000000000000 ) ) ;
#5145 = CARTESIAN_POINT ( 'NONE',  ( 70.19189222814998175, -86.77534409585553021, -42.52768597413476925 ) ) ;
#5146 = CARTESIAN_POINT ( 'NONE',  ( 115.5526452545247622, 0.8980012041604421569, -11.00651665394454071 ) ) ;
#5147 = CARTESIAN_POINT ( 'NONE',  ( -13.83992782281680078, -4.421549056456191451, -18.43133312422856562 ) ) ;
#5148 = CARTESIAN_POINT ( 'NONE',  ( 82.58377657508042091, -31.55352463209563751, -23.50578125650315542 ) ) ;
#5149 = CARTESIAN_POINT ( 'NONE',  ( 121.2485348109119769, -0.4660016031367893996, -10.09054647747474043 ) ) ;
#5150 = CARTESIAN_POINT ( 'NONE',  ( 119.1496481442453046, -3.383040157471821630, -19.15922257007629170 ) ) ;
#5151 = CARTESIAN_POINT ( 'NONE',  ( 69.69189222814998175, -41.76310523276723785, -23.89321520033831803 ) ) ;
#5152 = CARTESIAN_POINT ( 'NONE',  ( 117.4478481442453131, 0.2603800115204892296, -16.42320221600525088 ) ) ;
#5153 = CARTESIAN_POINT ( 'NONE',  ( 87.14323352029596492, -25.99489077589524300, -13.39321520033831625 ) ) ;
#5154 = ORIENTED_EDGE ( 'NONE', *, *, #41746, .F. ) ;
#5155 = DIRECTION ( 'NONE',  ( -0.1352586133458019424, -0.9908103287288495542, 0.000000000000000000 ) ) ;
#5156 = AXIS2_PLACEMENT_3D ( 'NONE', #6284, #37744, #27718 ) ;
#5157 = CARTESIAN_POINT ( 'NONE',  ( 119.2631014775786298, 0.2603800115204892296, -16.42320221600525088 ) ) ;
#5158 = CARTESIAN_POINT ( 'NONE',  ( 126.1270281442452870, 0.1319031606808879209, -14.10382304977623669 ) ) ;
#5159 = VECTOR ( 'NONE', #17717, 1000.000000000000114 ) ;
#5160 = CARTESIAN_POINT ( 'NONE',  ( 112.3424481442453384, -3.505236298600246325, -18.68346056562440793 ) ) ;
#5161 = CARTESIAN_POINT ( 'NONE',  ( 125.1059481442452750, -8.166667518702819706, -8.995218007635861213 ) ) ;
#5162 = STYLED_ITEM ( 'NONE', ( #21425 ), #34112 ) ;
#5163 = CARTESIAN_POINT ( 'NONE',  ( 109.8574890045247940, 0.8980012041604421569, -15.77991374673208469 ) ) ;
#5164 = CARTESIAN_POINT ( 'NONE',  ( 119.7169148109119874, -0.1624402480850797581, -16.17319339645315424 ) ) ;
#5165 = CYLINDRICAL_SURFACE ( 'NONE', #6371, 3.000000000000001776 ) ;
#5166 = CARTESIAN_POINT ( 'NONE',  ( 116.1082702545247827, -10.62599879583958717, -15.77991374673208469 ) ) ;
#5167 = EDGE_LOOP ( 'NONE', ( #4589, #3408, #5787, #27784, #30265, #1926 ) ) ;
#5168 = CARTESIAN_POINT ( 'NONE',  ( 121.0630641859119976, -8.321307733199551748, -9.223433127585318303 ) ) ;
#5169 = CARTESIAN_POINT ( 'NONE',  ( 123.6310548109119765, -5.638512984488999180, -18.83840828888717311 ) ) ;
#5170 = CARTESIAN_POINT ( 'NONE',  ( 96.54708369096698561, -24.69793907545987466, -15.18364567559777178 ) ) ;
#5171 = CARTESIAN_POINT ( 'NONE',  ( 111.4231914802848422, -3.929494816611151631, -18.62311481910791144 ) ) ;
#5172 = CIRCLE ( 'NONE', #8092, 1.610000000000000986 ) ;
#5173 = CARTESIAN_POINT ( 'NONE',  ( 118.4689281442453392, -10.15424416112533912, -14.75197769757731336 ) ) ;
#5174 = CARTESIAN_POINT ( 'NONE',  ( 68.03116533996660564, -0.6815855639037916580, -16.39321520033830737 ) ) ;
#5175 = CARTESIAN_POINT ( 'NONE',  ( 124.5068972094509689, -9.682373403232579889, -12.05773893725193879 ) ) ;
#5176 = CARTESIAN_POINT ( 'NONE',  ( 124.3685014775786328, 0.4262465694468514643, -12.03445270309931736 ) ) ;
#5177 = CARTESIAN_POINT ( 'NONE',  ( 121.2714235609119697, 0.6414057260225808355, -11.69287257290601545 ) ) ;
#5178 = CARTESIAN_POINT ( 'NONE',  ( 124.1415948109119540, -3.505236298600246325, -18.68346056562440793 ) ) ;
#5179 = AXIS2_PLACEMENT_3D ( 'NONE', #39761, #43635, #1237 ) ;
#5180 = CARTESIAN_POINT ( 'NONE',  ( 125.2986504416607261, -11.52710089177262098, -16.05128639071223162 ) ) ;
#5181 = CARTESIAN_POINT ( 'NONE',  ( 122.6667014775786413, -7.893985811506177619, -18.51759400769804742 ) ) ;
#5182 = CARTESIAN_POINT ( 'NONE',  ( 118.8092881442453290, -0.1624402480850797581, -16.17319339645315424 ) ) ;
#5183 = CARTESIAN_POINT ( 'NONE',  ( 121.4187148109119789, -3.505236298600246325, -18.68346056562440793 ) ) ;
#5184 = ORIENTED_EDGE ( 'NONE', *, *, #36160, .F. ) ;
#5185 = CARTESIAN_POINT ( 'NONE',  ( 123.4041481442452834, -10.30919188438810075, -12.61870101168855918 ) ) ;
#5186 = CARTESIAN_POINT ( 'NONE',  ( 115.6325948109119821, 0.2603800115204892296, -16.42320221600525088 ) ) ;
#5187 = CARTESIAN_POINT ( 'NONE',  ( 114.8581140045248361, 0.1403307496149616695, -15.46607636864997204 ) ) ;
#5188 = CYLINDRICAL_SURFACE ( 'NONE', #18927, 3.499999999999998668 ) ;
#5189 =( GEOMETRIC_REPRESENTATION_CONTEXT ( 3 ) GLOBAL_UNCERTAINTY_ASSIGNED_CONTEXT ( ( #4147 ) ) GLOBAL_UNIT_ASSIGNED_CONTEXT ( ( #7073, #34041, #28503 ) ) REPRESENTATION_CONTEXT ( 'NONE', 'WORKASPACE' ) );
#5190 = CARTESIAN_POINT ( 'NONE',  ( 122.7801548109119665, -6.222761293078241884, -8.102969835052219238 ) ) ;
#5191 = ORIENTED_EDGE ( 'NONE', *, *, #495, .T. ) ;
#5192 = CARTESIAN_POINT ( 'NONE',  ( 121.3052614775786111, -1.834011780172310813, -8.268836392978581529 ) ) ;
#5193 = CARTESIAN_POINT ( 'NONE',  ( 106.1070202545248407, 0.1403307496149616695, -11.32035403202665336 ) ) ;
#5194 = CARTESIAN_POINT ( 'NONE',  ( 111.1076452545248259, -9.868328341294098749, -15.46607636864997204 ) ) ;
#5195 = CARTESIAN_POINT ( 'NONE',  ( 121.9470836909669913, -25.99489077589524300, -13.39321520033831447 ) ) ;
#5196 = CARTESIAN_POINT ( 'NONE',  ( 113.1933481442453058, -5.574606645277164318, -18.38911715685844683 ) ) ;
#5197 = CARTESIAN_POINT ( 'NONE',  ( 74.47157298427187300, -3.053873105668316601, -14.39321520033831625 ) ) ;
#5198 = CARTESIAN_POINT ( 'NONE',  ( 116.3166296295247832, -4.863998795839590272, -8.388885654883775800 ) ) ;
#5199 = ORIENTED_EDGE ( 'NONE', *, *, #39518, .T. ) ;
#5200 = CARTESIAN_POINT ( 'NONE',  ( 125.6164881442453094, -9.565557343593413364, -10.61323700422348004 ) ) ;
#5201 = CARTESIAN_POINT ( 'NONE',  ( 123.9800954359119771, -11.07370829466463569, -12.81314460846529002 ) ) ;
#5202 = CARTESIAN_POINT ( 'NONE',  ( 121.1325173109119788, 0.2312338769422704887, -16.08380026872395874 ) ) ;
#5203 = DIRECTION ( 'NONE',  ( -0.9495615000563050190, 0.3135808629537517600, 0.000000000000000000 ) ) ;
#5204 = ADVANCED_FACE ( 'NONE', ( #43094 ), #37629, .T. ) ;
#5205 = CARTESIAN_POINT ( 'NONE',  ( 108.2600671295247992, 0.1403307496149613920, -13.39321520033831447 ) ) ;
#5206 = ORIENTED_EDGE ( 'NONE', *, *, #10240, .F. ) ;
#5207 = CARTESIAN_POINT ( 'NONE',  ( 115.0086014775786509, -4.089484607189486809, -7.948022111789456723 ) ) ;
#5208 = CARTESIAN_POINT ( 'NONE',  ( 125.3895814775786448, -7.893985811506177619, -18.51759400769804742 ) ) ;
#5209 = VECTOR ( 'NONE', #37485, 1000.000000000000000 ) ;
#5210 = CARTESIAN_POINT ( 'NONE',  ( 125.7299414775786346, -10.15424416112533912, -14.75197769757731336 ) ) ;
#5211 = CARTESIAN_POINT ( 'NONE',  ( 116.0296814775786345, -1.833838273342658809, -17.42832698103878286 ) ) ;
#5212 = SHAPE_REPRESENTATION_RELATIONSHIP ( 'NONE' , 'NONE' ,  #850, #15621 ) ;
#5213 = CARTESIAN_POINT ( 'NONE',  ( 70.19189222814998175, -54.47411573338475677, -34.99246555962335492 ) ) ;
#5214 = B_SPLINE_CURVE_WITH_KNOTS ( 'NONE', 3,
 ( #43337, #21907, #26231, #8455, #12331, #22579, #39690, #40140, #33045, #39465, #15746, #29648, #15071, #15290, #8904, #29198, #28983, #36697, #26010, #39234, #5466, #22136, #18496, #39914, #43109, #43562, #35801, #4571, #36028, #42889, #25558 ),
 .UNSPECIFIED., .F., .F.,
 ( 4, 2, 2, 1, 1, 1, 2, 2, 2, 1, 1, 1, 2, 2, 2, 1, 2, 2, 4 ),
 ( 0.000000000000000000, 0.2499999999998858691, 0.3749999999998160916, 0.4374999999997945532, 0.4687499999997689626, 0.4843749999997562505, 0.4921874999997510325, 0.4999999999997458699, 0.6249999999996926903, 0.6874999999996759259, 0.7187499999996675992, 0.7343749999996631583, 0.7421874999996734834, 0.7499999999996838085, 0.8124999999997638556, 0.8437499999997956079, 0.8593749999998111511, 0.8749999999998266942, 1.000000000000000000 ),
 .UNSPECIFIED. ) ;
#5215 = DIRECTION ( 'NONE',  ( 1.000000000000000000, 0.000000000000000000, -0.000000000000000000 ) ) ;
#5216 = CARTESIAN_POINT ( 'NONE',  ( 115.9162281442453235, -4.089484607189486809, -7.948022111789456723 ) ) ;
#5217 = CARTESIAN_POINT ( 'NONE',  ( 113.7468640045248236, 0.1403307496149616695, -15.46607636864997204 ) ) ;
#5218 = AXIS2_PLACEMENT_3D ( 'NONE', #17388, #24232, #18276 ) ;
#5219 = CARTESIAN_POINT ( 'NONE',  ( 122.6099748109119929, -9.261995988541697145, -16.69588392320189030 ) ) ;
#5220 = CARTESIAN_POINT ( 'NONE',  ( 84.10862215250544693, -26.60966817898065884, -11.90521360603286816 ) ) ;
#5221 = ORIENTED_EDGE ( 'NONE', *, *, #29199, .T. ) ;
#5222 = EDGE_CURVE ( 'NONE', #21278, #37706, #20878, .T. ) ;
#5223 = CARTESIAN_POINT ( 'NONE',  ( 114.3278814775786429, -10.30919188438810075, -12.61870101168855918 ) ) ;
#5224 = EDGE_CURVE ( 'NONE', #25522, #39963, #16521, .T. ) ;
#5225 = EDGE_CURVE ( 'NONE', #44907, #3542, #22786, .T. ) ;
#5226 = CARTESIAN_POINT ( 'NONE',  ( 112.2289948109119848, -7.643976991954077427, -18.09477374809248928 ) ) ;
#5227 = CARTESIAN_POINT ( 'NONE',  ( -3.429934629567074733, -4.841764211284793618, -8.893215200338314474 ) ) ;
#5228 = CARTESIAN_POINT ( 'NONE',  ( 112.2289948109119848, -1.834011780172310813, -8.268836392978581529 ) ) ;
#5229 = ORIENTED_EDGE ( 'NONE', *, *, #23105, .F. ) ;
#5230 = CARTESIAN_POINT ( 'NONE',  ( 118.1852948109119836, -5.638512984488999180, -18.83840828888717311 ) ) ;
#5231 = DIRECTION ( 'NONE',  ( 0.000000000000000000, 0.000000000000000000, -1.000000000000000000 ) ) ;
#5232 = CARTESIAN_POINT ( 'NONE',  ( 121.9470836909669913, -27.84333996136784961, -14.15691383771150136 ) ) ;
#5233 = CARTESIAN_POINT ( 'NONE',  ( 115.4451630180080883, 0.7607806665037644134, -14.64321520033834467 ) ) ;
#5234 = CARTESIAN_POINT ( 'NONE',  ( 136.2315975805971959, -2.595879224868264945, -7.997781276090496938 ) ) ;
#5235 = CARTESIAN_POINT ( 'NONE',  ( 114.7816948109119863, -9.859900752359374465, -12.68260735090039404 ) ) ;
#5236 = DIRECTION ( 'NONE',  ( 1.000000000000000000, 0.000000000000000000, -0.000000000000000000 ) ) ;
#5237 = CIRCLE ( 'NONE', #14693, 2.000000000000001776 ) ;
#5238 = CARTESIAN_POINT ( 'NONE',  ( 125.3082514830540788, -3.264913200334888632, -20.36649584582930572 ) ) ;
#5239 = CARTESIAN_POINT ( 'NONE',  ( 112.5693548109119888, 0.4262465694468514643, -12.03445270309931736 ) ) ;
#5240 = CARTESIAN_POINT ( 'NONE',  ( 112.2857214775786474, -4.089484607189486809, -7.948022111789456723 ) ) ;
#5241 = CARTESIAN_POINT ( 'NONE',  ( 116.6378439406596073, -9.495374643002518766, -15.38986610286289647 ) ) ;
#5242 = CARTESIAN_POINT ( 'NONE',  ( 123.5743281442453139, -2.084020599724406786, -8.691656652584148546 ) ) ;
#5243 = CARTESIAN_POINT ( 'NONE',  ( 88.46631044337289040, -25.99489077589524300, -13.39321520033831625 ) ) ;
#5244 = CARTESIAN_POINT ( 'NONE',  ( 124.0848681442452772, -4.089484607189486809, -7.948022111789456723 ) ) ;
#5245 = CARTESIAN_POINT ( 'NONE',  ( 122.5532481442453019, -10.63000616557722466, -14.87417383870573495 ) ) ;
#5246 = ORIENTED_EDGE ( 'NONE', *, *, #31182, .F. ) ;
#5247 = CARTESIAN_POINT ( 'NONE',  ( 117.5569581407225996, -1.081026697600512732, -17.18181821144401056 ) ) ;
#5248 = CARTESIAN_POINT ( 'NONE',  ( 112.9134265045247645, -7.250697342233347165, -19.15521520033831138 ) ) ;
#5249 = ADVANCED_FACE ( 'NONE', ( #8885 ), #43547, .T. ) ;
#5250 = CARTESIAN_POINT ( 'NONE',  ( 112.1494421295248003, -9.868328341294093420, -13.39321520033831447 ) ) ;
#5251 = CARTESIAN_POINT ( 'NONE',  ( 109.8574890045248509, -9.868328341294098749, -11.32035403202665869 ) ) ;
#5252 = CARTESIAN_POINT ( 'NONE',  ( 125.2194014775786286, 0.1319031606810284196, -14.10382304977525614 ) ) ;
#5253 = CARTESIAN_POINT ( 'NONE',  ( 116.8238548109119819, -4.089484607189486809, -7.948022111789456723 ) ) ;
#5254 = ORIENTED_EDGE ( 'NONE', *, *, #6693, .T. ) ;
#5255 = CARTESIAN_POINT ( 'NONE',  ( 119.7434548109119703, -2.527210466738042172, -8.967976844669124148 ) ) ;
#5256 = DIRECTION ( 'NONE',  ( -0.9970811988817434024, 0.07634843047859724008, 0.000000000000000000 ) ) ;
#5257 = CARTESIAN_POINT ( 'NONE',  ( 113.2500748109119968, -3.505236298600246325, -18.68346056562440793 ) ) ;
#5258 = EDGE_CURVE ( 'NONE', #22202, #7697, #8496, .T. ) ;
#5259 = B_SPLINE_CURVE_WITH_KNOTS ( 'NONE', 3,
 ( #16416, #9570, #40353, #2488, #26217, #26670, #12543, #6143, #23485, #20064 ),
 .UNSPECIFIED., .F., .F.,
 ( 4, 3, 3, 4 ),
 ( 0.000000000000000000, 0.0001671877548681254834, 0.0003343755096277680285, 0.0006463528481650619413 ),
 .UNSPECIFIED. ) ;
#5260 = CARTESIAN_POINT ( 'NONE',  ( 113.1410369858783724, -2.378957183258581853, -17.95140958770220152 ) ) ;
#5261 = CARTESIAN_POINT ( 'NONE',  ( 120.0572748109119772, -3.383040157471821630, -19.15922257007629170 ) ) ;
#5262 = EDGE_CURVE ( 'NONE', #17071, #38525, #36894, .T. ) ;
#5263 = CARTESIAN_POINT ( 'NONE',  ( 111.8021765045248372, -7.250697342233347165, -19.15521520033831138 ) ) ;
#5264 = FACE_OUTER_BOUND ( 'NONE', #17363, .T. ) ;
#5265 = ORIENTED_EDGE ( 'NONE', *, *, #43179, .F. ) ;
#5266 = CARTESIAN_POINT ( 'NONE',  ( 115.4451630180080883, 0.7607806665037644134, -14.64321520033834467 ) ) ;
#5267 = CARTESIAN_POINT ( 'NONE',  ( 120.3976348109119812, -7.643976991954077427, -18.09477374809248928 ) ) ;
#5268 = CARTESIAN_POINT ( 'NONE',  ( 115.1787814775786387, -9.988377603198976828, -10.36322818467138340 ) ) ;
#5269 = CARTESIAN_POINT ( 'NONE',  ( 117.2209414775786485, -7.893985811506177619, -18.51759400769804742 ) ) ;
#5270 = CARTESIAN_POINT ( 'NONE',  ( 136.2916311807211400, -7.115752929798599524, -18.77480778557723440 ) ) ;
#5271 = CARTESIAN_POINT ( 'NONE',  ( 122.5532481442453019, 0.4262465694468514643, -12.03445270309931736 ) ) ;
#5272 = CARTESIAN_POINT ( 'NONE',  ( 120.3976348109119812, -7.643976991954077427, -18.09477374809248928 ) ) ;
#5273 = EDGE_LOOP ( 'NONE', ( #19015, #20640, #32798, #23613, #3675 ) ) ;
#5274 = VECTOR ( 'NONE', #41527, 1000.000000000000227 ) ;
#5275 = CARTESIAN_POINT ( 'NONE',  ( 121.3408766859119794, -0.06289925094097943703, -9.412459353600674206 ) ) ;
#5276 = VECTOR ( 'NONE', #32610, 1000.000000000000114 ) ;
#5277 = CARTESIAN_POINT ( 'NONE',  ( 112.0588148109119828, 0.5811942927096154232, -14.16772938898807155 ) ) ;
#5278 = B_SPLINE_CURVE_WITH_KNOTS ( 'NONE', 3,
 ( #39787, #36580, #19715, #19039 ),
 .UNSPECIFIED., .F., .F.,
 ( 4, 4 ),
 ( 0.000000000000000000, 1.568264261493034943E-06 ),
 .UNSPECIFIED. ) ;
#5279 = CARTESIAN_POINT ( 'NONE',  ( 117.1642148109119859, -0.8288870151387760510, -10.36305467784173118 ) ) ;
#5280 = ORIENTED_EDGE ( 'NONE', *, *, #3581, .T. ) ;
#5281 = CARTESIAN_POINT ( 'NONE',  ( 120.5074391859119913, -1.406689858478933353, -17.56299727309130887 ) ) ;
#5282 = B_SPLINE_CURVE_WITH_KNOTS ( 'NONE', 3,
 ( #11356, #21837, #856, #4728 ),
 .UNSPECIFIED., .F., .F.,
 ( 4, 4 ),
 ( 0.000000000000000000, 1.000000000000000000 ),
 .UNSPECIFIED. ) ;
#5283 = ADVANCED_FACE ( 'NONE', ( #22561 ), #36680, .T. ) ;
#5284 = CARTESIAN_POINT ( 'NONE',  ( 115.8595014775786609, -1.834011780172310813, -8.268836392978581529 ) ) ;
#5285 = CARTESIAN_POINT ( 'NONE',  ( 115.4137390045248566, 0.8980012041604421569, -15.77991374673208469 ) ) ;
#5286 = CARTESIAN_POINT ( 'NONE',  ( 114.1577014775786552, -3.505236298600246325, -18.68346056562440793 ) ) ;
#5287 = ORIENTED_EDGE ( 'NONE', *, *, #1737, .T. ) ;
#5288 = CIRCLE ( 'NONE', #30780, 1.499999999999998002 ) ;
#5289 = ORIENTED_EDGE ( 'NONE', *, *, #16411, .F. ) ;
#5290 = CARTESIAN_POINT ( 'NONE',  ( 121.8158014775786171, -4.153390946401325223, -8.397313243818185668 ) ) ;
#5291 = CARTESIAN_POINT ( 'NONE',  ( 120.7379948109119709, 0.4262465694468514643, -12.03445270309931736 ) ) ;
#5292 = DIRECTION ( 'NONE',  ( 0.8636456077245089347, -0.5040994586965589219, 0.000000000000000000 ) ) ;
#5293 = ORIENTED_EDGE ( 'NONE', *, *, #550, .T. ) ;
#5294 = DIRECTION ( 'NONE',  ( 1.000000000000000000, 0.000000000000000000, 0.000000000000000000 ) ) ;
#5295 = CARTESIAN_POINT ( 'NONE',  ( 62.76162801216658949, -64.72030100442231060, -45.93989290692245220 ) ) ;
#5296 = CARTESIAN_POINT ( 'NONE',  ( 108.3989733795248753, -8.938348069036489818, -17.46756447353520159 ) ) ;
#5297 = CARTESIAN_POINT ( 'NONE',  ( 115.8027748109119841, -0.4660016031367893996, -10.09054647747474043 ) ) ;
#5299 = CARTESIAN_POINT ( 'NONE',  ( 115.6325948109119821, -9.565557343593413364, -10.61323700422348004 ) ) ;
#5298 = CARTESIAN_POINT ( 'NONE',  ( 115.0653281442453277, -6.344957434206662583, -7.627207830600332805 ) ) ;
#5300 = CARTESIAN_POINT ( 'NONE',  ( 120.3409081442453044, -8.899110576539710493, -16.42337572283490132 ) ) ;
#5301 = CARTESIAN_POINT ( 'NONE',  ( 35.90261398037149121, 14.17005867477686820, -8.593215200338315540 ) ) ;
#5302 = ORIENTED_EDGE ( 'NONE', *, *, #4120, .T. ) ;
#5303 = CARTESIAN_POINT ( 'NONE',  ( 119.7169148109119874, -0.1624402480850797581, -16.17319339645315424 ) ) ;
#5304 = CIRCLE ( 'NONE', #7517, 1.500000000000001332 ) ;
#5305 = FACE_OUTER_BOUND ( 'NONE', #20275, .T. ) ;
#5306 = CARTESIAN_POINT ( 'NONE',  ( 114.3024890045248156, 0.8980012041604421569, -15.77991374673208469 ) ) ;
#5307 = VECTOR ( 'NONE', #35865, 1000.000000000000000 ) ;
#5308 = CARTESIAN_POINT ( 'NONE',  ( 115.6220983795247861, -8.402594152722688392, -16.93181055722141792 ) ) ;
#5309 = CARTESIAN_POINT ( 'NONE',  ( 111.3160046295247838, -4.863998795839590272, -7.631215200338315796 ) ) ;
#5310 = CARTESIAN_POINT ( 'NONE',  ( 117.8449348109119938, -8.166667518702817929, -8.995218007635861213 ) ) ;
#5311 = ORIENTED_EDGE ( 'NONE', *, *, #18143, .T. ) ;
#5312 = CARTESIAN_POINT ( 'NONE',  ( 122.5532481442453019, -10.63000616557722466, -14.87417383870573495 ) ) ;
#5313 = CARTESIAN_POINT ( 'NONE',  ( 88.46631044337289040, -24.14644159042263993, -12.62951656296512937 ) ) ;
#5314 = CARTESIAN_POINT ( 'NONE',  ( 109.1629577545248395, -7.250697342233347165, -7.631215200338321125 ) ) ;
#5315 = CARTESIAN_POINT ( 'NONE',  ( 118.8660148109119774, -10.30919188438810075, -12.61870101168855918 ) ) ;
#5316 = CARTESIAN_POINT ( 'NONE',  ( 115.9162281442453235, -4.089484607189486809, -7.948022111789456723 ) ) ;
#5317 = DIRECTION ( 'NONE',  ( 1.000000000000000000, 0.000000000000000000, 0.000000000000000000 ) ) ;
#5318 = CARTESIAN_POINT ( 'NONE',  ( 54.86886719809545809, -45.79521720516596872, -17.39321520033831447 ) ) ;
#5319 = ORIENTED_EDGE ( 'NONE', *, *, #18365, .F. ) ;
#5320 = CARTESIAN_POINT ( 'NONE',  ( -2.326236797655081290, -6.982629615722759198, -7.609261158995283658 ) ) ;
#5321 = CARTESIAN_POINT ( 'NONE',  ( 109.2294421287695059, -10.35035779373698972, -14.13938231603832207 ) ) ;
#5322 = CARTESIAN_POINT ( 'NONE',  ( 120.9081748109119872, -4.153390946401325223, -8.397313243818185668 ) ) ;
#5323 = CARTESIAN_POINT ( 'NONE',  ( 109.9269421295247753, -9.868328341294093420, -13.39321520033831447 ) ) ;
#5324 = CARTESIAN_POINT ( 'NONE',  ( 111.5938171295247940, 0.1403307496149613920, -13.39321520033831447 ) ) ;
#5325 = CARTESIAN_POINT ( 'NONE',  ( 116.1431348109119881, 0.1319031606808879209, -14.10382304977623669 ) ) ;
#5326 = DIRECTION ( 'NONE',  ( 0.000000000000000000, -0.4669533266896288004, -0.8842819633428519177 ) ) ;
#5327 = CARTESIAN_POINT ( 'NONE',  ( 70.88883345414545545, -25.51877778662253604, -5.473826388607204940 ) ) ;
#5328 = CARTESIAN_POINT ( 'NONE',  ( 111.3213681442453264, -7.643976991954077427, -18.09477374809248928 ) ) ;
#5329 = CARTESIAN_POINT ( 'NONE',  ( 119.3198281442452924, 0.5811942927096110934, -14.16772938898807510 ) ) ;
#5331 = ORIENTED_EDGE ( 'NONE', *, *, #23077, .F. ) ;
#5330 = EDGE_CURVE ( 'NONE', #8760, #33236, #32592, .T. ) ;
#5332 = CARTESIAN_POINT ( 'NONE',  ( 116.9940348109119839, -0.1624402480850797581, -16.17319339645315424 ) ) ;
#5333 = CARTESIAN_POINT ( 'NONE',  ( 116.4834948109119779, -1.561330072975668504, -17.79121239304076951 ) ) ;
#5334 = CARTESIAN_POINT ( 'NONE',  ( 119.9438214775786378, -7.893985811506177619, -18.51759400769804742 ) ) ;
#5335 = B_SPLINE_CURVE_WITH_KNOTS ( 'NONE', 3,
 ( #32284, #25001, #35696, #379 ),
 .UNSPECIFIED., .F., .F.,
 ( 4, 4 ),
 ( 0.000000000000000000, 1.000000000000000000 ),
 .UNSPECIFIED. ) ;
#5336 = CARTESIAN_POINT ( 'NONE',  ( 123.5743281442453139, -2.084020599724406786, -8.691656652584148546 ) ) ;
#5337 = EDGE_LOOP ( 'NONE', ( #2376, #16218, #13316, #13104 ) ) ;
#5338 = CARTESIAN_POINT ( 'NONE',  ( 91.11246428952674137, -25.99489077589524300, -13.39321520033831625 ) ) ;
#5339 = CIRCLE ( 'NONE', #43231, 1.200000000000000178 ) ;
#5340 = AXIS2_PLACEMENT_3D ( 'NONE', #17069, #38457, #38237 ) ;
#5341 = CARTESIAN_POINT ( 'NONE',  ( 120.9649014775786355, -3.383040157471821630, -19.15922257007629170 ) ) ;
#5342 = CARTESIAN_POINT ( 'NONE',  ( 124.6565730087413044, -8.387630329567796750, -6.398857485523961941 ) ) ;
#5343 = CARTESIAN_POINT ( 'NONE',  ( 125.1059481442452750, -8.166667518702819706, -8.995218007635861213 ) ) ;
#5344 = EDGE_CURVE ( 'NONE', #13081, #33790, #4117, .T. ) ;
#5345 = CARTESIAN_POINT ( 'NONE',  ( 89.40092984481313465, -26.60966817898065884, -11.90521360603286816 ) ) ;
#5346 = CARTESIAN_POINT ( 'NONE',  ( 121.1325173109119788, -9.289237151508434209, -11.05642687123711276 ) ) ;
#5347 = CARTESIAN_POINT ( 'NONE',  ( 136.0826545884683583, -0.7358842820514963634, -17.64142694063895433 ) ) ;
#5348 = CARTESIAN_POINT ( 'NONE',  ( 109.5796765045248122, -2.791137627527939813, -8.388885654883777576 ) ) ;
#5349 = CONICAL_SURFACE ( 'NONE', #9004, 1.610000000000000986, 0.9599310885968765916 ) ;
#5350 = CARTESIAN_POINT ( 'NONE',  ( 90.71204046351577688, -10.71075648645643774, -13.24321520033830879 ) ) ;
#5351 = DIRECTION ( 'NONE',  ( -0.07634843047859724008, -0.9970811988817435134, 0.000000000000000000 ) ) ;
#5352 = CARTESIAN_POINT ( 'NONE',  ( 119.0929214775786278, -4.153390946401325223, -8.397313243818185668 ) ) ;
#5353 = CARTESIAN_POINT ( 'NONE',  ( 124.9357681442453014, -1.834011780172310813, -8.268836392978581529 ) ) ;
#5354 = CARTESIAN_POINT ( 'NONE',  ( 64.92272412734682518, -13.29087679925527254, -15.14070786268923285 ) ) ;
#5355 = EDGE_LOOP ( 'NONE', ( #44589, #10268, #23473, #9664 ) ) ;
#5356 = CARTESIAN_POINT ( 'NONE',  ( 116.7365233795247832, -8.399532701772287169, -16.92874910627105223 ) ) ;
#5357 = CARTESIAN_POINT ( 'NONE',  ( 110.7603796295247918, -4.863998795839590272, -8.388885654883775800 ) ) ;
#5358 = CARTESIAN_POINT ( 'NONE',  ( 117.6747548109119919, -7.643976991954077427, -18.09477374809248928 ) ) ;
#5359 = DIRECTION ( 'NONE',  ( 0.000000000000000000, -0.9242245927363028635, -0.3818493186865930533 ) ) ;
#5360 = CARTESIAN_POINT ( 'NONE',  ( 67.43171844381110702, -0.1877862098377165168, -10.39321520033831625 ) ) ;
#5361 = CARTESIAN_POINT ( 'NONE',  ( -2.501350073892645298, -7.035121566246528069, -19.26840662495741796 ) ) ;
#5363 = CARTESIAN_POINT ( 'NONE',  ( 123.4041481442452834, -10.30919188438810075, -12.61870101168855918 ) ) ;
#5362 = CARTESIAN_POINT ( 'NONE',  ( 94.20708369096698220, -26.42437990495228917, -14.12788525418686270 ) ) ;
#5364 = CARTESIAN_POINT ( 'NONE',  ( 121.4754414775786131, -1.833838273342659697, -17.42832698103878286 ) ) ;
#5365 = ORIENTED_EDGE ( 'NONE', *, *, #25199, .T. ) ;
#5366 = CARTESIAN_POINT ( 'NONE',  ( 114.4222457829843762, 0.6362173239733635022, -14.64321520033831447 ) ) ;
#5367 = CARTESIAN_POINT ( 'NONE',  ( 124.9357681442453014, -1.834011780172310813, -8.268836392978581529 ) ) ;
#5368 = CARTESIAN_POINT ( 'NONE',  ( 109.0935046295247872, -4.863998795839590272, -18.39754474579285315 ) ) ;
#5369 = CARTESIAN_POINT ( 'NONE',  ( 120.7947214775786193, -0.8288870151387760510, -10.36305467784173118 ) ) ;
#5371 = CARTESIAN_POINT ( 'NONE',  ( 120.1140014775786398, -7.894159318335828068, -9.358103419637847864 ) ) ;
#5370 = AXIS2_PLACEMENT_3D ( 'NONE', #21196, #35073, #24841 ) ;
#5372 = CARTESIAN_POINT ( 'NONE',  ( 124.6565730087442745, 2.573342726250678059, -15.84738921862590288 ) ) ;
#5373 = CARTESIAN_POINT ( 'NONE',  ( 108.6073327545248048, -2.477300249445798297, -19.15521520033831138 ) ) ;
#5374 = CARTESIAN_POINT ( 'NONE',  ( 70.19189222814998175, -52.97765562947117957, -34.39388673445118627 ) ) ;
#5375 = DIRECTION ( 'NONE',  ( 0.000000000000000000, 0.000000000000000000, -1.000000000000000000 ) ) ;
#5376 = LINE ( 'NONE', #36374, #8066 ) ;
#5377 = CARTESIAN_POINT ( 'NONE',  ( 112.9134265045247645, -7.250697342233347165, -19.15521520033831138 ) ) ;
#5378 = CARTESIAN_POINT ( 'NONE',  ( -13.54490672864917045, -3.903797476764282681, -18.73945354926143736 ) ) ;
#5379 = CARTESIAN_POINT ( 'NONE',  ( 83.16394245587648015, -30.76310523276723785, -21.89321520033831447 ) ) ;
#5380 = CARTESIAN_POINT ( 'NONE',  ( 119.3765548109119834, 0.9020085738987339008, -11.91225656197089222 ) ) ;
#5381 = CARTESIAN_POINT ( 'NONE',  ( 123.7445081442452874, -1.561330072975668948, -17.79121239304076951 ) ) ;
#5382 = CARTESIAN_POINT ( 'NONE',  ( 151.2860562277021472, -2.520019956603805511, -15.26558354049377009 ) ) ;
#5383 = CARTESIAN_POINT ( 'NONE',  ( 118.2987481442453088, -1.561330072975668504, -17.79121239304076951 ) ) ;
#5384 = CARTESIAN_POINT ( 'NONE',  ( 72.30589087944665039, -69.86246063582763099, -43.34095636271326413 ) ) ;
#5385 = ORIENTED_EDGE ( 'NONE', *, *, #12196, .F. ) ;
#5386 = DIRECTION ( 'NONE',  ( 0.000000000000000000, -0.9242245927363029745, -0.3818493186865929978 ) ) ;
#5387 = AXIS2_PLACEMENT_3D ( 'NONE', #43261, #26833, #26151 ) ;
#5388 = CARTESIAN_POINT ( 'NONE',  ( 124.4252281442452812, -9.261995988541697145, -16.69588392320189030 ) ) ;
#5389 = CARTESIAN_POINT ( 'NONE',  ( 121.5321681442453183, -9.988377603198976828, -10.36322818467138340 ) ) ;
#5390 = CARTESIAN_POINT ( 'NONE',  ( 125.5597614775786326, -7.894159318335828068, -9.358103419637847864 ) ) ;
#5391 = CARTESIAN_POINT ( 'NONE',  ( 115.0086014775786509, -5.574606645277164318, -18.38911715685844683 ) ) ;
#5392 = CARTESIAN_POINT ( 'NONE',  ( 123.8012348109119642, 0.2603800115204892296, -16.42320221600525088 ) ) ;
#5393 = CARTESIAN_POINT ( 'NONE',  ( 110.2047546295247855, -4.863998795839590272, -7.631215200338315796 ) ) ;
#5394 = EDGE_CURVE ( 'NONE', #30461, #33992, #23480, .T. ) ;
#5395 = CARTESIAN_POINT ( 'NONE',  ( 118.6391081442452986, -5.574606645277164318, -18.38911715685844683 ) ) ;
#5396 = DIRECTION ( 'NONE',  ( 0.2407039305251456596, -0.3604685577742790525, 0.9011792478113757054 ) ) ;
#5397 = CARTESIAN_POINT ( 'NONE',  ( 90.45092582798827152, -24.14644159042263993, -12.62951656296512937 ) ) ;
#5398 = ORIENTED_EDGE ( 'NONE', *, *, #17508, .F. ) ;
#5399 = CARTESIAN_POINT ( 'NONE',  ( 122.1743141859119817, -8.321307733199551748, -9.223433127585318303 ) ) ;
#5400 = CARTESIAN_POINT ( 'NONE',  ( 122.3830681442452857, -8.166667518702819706, -8.995218007635861213 ) ) ;
#5401 = CARTESIAN_POINT ( 'NONE',  ( 113.5385046295247804, -4.863998795839541422, -18.39754474579285315 ) ) ;
#5402 = CARTESIAN_POINT ( 'NONE',  ( 62.10612082415807578, -3.658631476800715099, -7.496619392082022770 ) ) ;
#5403 = DIRECTION ( 'NONE',  ( -0.000000000000000000, -0.9284778069183718952, -0.3713878862591649677 ) ) ;
#5404 = CARTESIAN_POINT ( 'NONE',  ( 117.8449348109119938, -1.833838273342659253, -17.42832698103878286 ) ) ;
#5405 = DIRECTION ( 'NONE',  ( -0.8636456077245088236, 0.5040994586965589219, 0.000000000000000000 ) ) ;
#5406 = CARTESIAN_POINT ( 'NONE',  ( 119.7434548109119703, -4.863998795839242995, -13.39321520033831447 ) ) ;
#5407 = CARTESIAN_POINT ( 'NONE',  ( 123.0070614775786169, -10.15424416112533912, -14.75197769757731336 ) ) ;
#5408 = CARTESIAN_POINT ( 'NONE',  ( 116.4642898793805443, -2.191907684172563986, -18.20049396185734025 ) ) ;
#5409 = CARTESIAN_POINT ( 'NONE',  ( 124.9357681442453014, -7.643976991954077427, -18.09477374809248928 ) ) ;
#5410 = CARTESIAN_POINT ( 'NONE',  ( 110.2184548109119788, -2.211393927326565922, -15.67656524173425403 ) ) ;
#5411 = EDGE_CURVE ( 'NONE', #20823, #24368, #45125, .T. ) ;
#5412 = CARTESIAN_POINT ( 'NONE',  ( 122.0427081442452817, 0.5811942927096110934, -14.16772938898807510 ) ) ;
#5413 = CARTESIAN_POINT ( 'NONE',  ( 116.3133148109120043, -2.084020599724406786, -8.691656652584148546 ) ) ;
#5414 = CARTESIAN_POINT ( 'NONE',  ( 122.9503348109119827, -9.859900752359378018, -12.68260735090039759 ) ) ;
#5415 = ORIENTED_EDGE ( 'NONE', *, *, #15561, .F. ) ;
#5416 = CARTESIAN_POINT ( 'NONE',  ( 121.4754414775786131, -8.166667518702819706, -8.995218007635861213 ) ) ;
#5417 = CARTESIAN_POINT ( 'NONE',  ( 114.7816948109119863, 0.5811942927096154232, -14.16772938898807155 ) ) ;
#5418 = CARTESIAN_POINT ( 'NONE',  ( 116.0388171295248014, 0.1403307496149613920, -13.39321520033831447 ) ) ;
#5419 = FACE_OUTER_BOUND ( 'NONE', #6364, .T. ) ;
#5420 = CARTESIAN_POINT ( 'NONE',  ( 123.5743281442453139, -2.084020599724406786, -8.691656652584148546 ) ) ;
#5421 = CARTESIAN_POINT ( 'NONE',  ( 123.0070614775786169, 0.9020085738987339008, -11.91225656197089222 ) ) ;
#5422 = CARTESIAN_POINT ( 'NONE',  ( 113.9552233795247815, -8.938348069036489818, -17.46756447353520159 ) ) ;
#5423 = CARTESIAN_POINT ( 'NONE',  ( 108.3295202545248657, 0.1403307496149616695, -11.32035403202665336 ) ) ;
#5424 = DIRECTION ( 'NONE',  ( 0.000000000000000000, 0.3818493186865927203, -0.9242245927363029745 ) ) ;
#5425 = CARTESIAN_POINT ( 'NONE',  ( 112.4559014775786778, -0.1624402480850797581, -16.17319339645315424 ) ) ;
#5426 = DIRECTION ( 'NONE',  ( 0.000000000000000000, -0.3818493186865927203, 0.9242245927363029745 ) ) ;
#5427 = CARTESIAN_POINT ( 'NONE',  ( 115.1359265045248605, -2.791137627527939813, -8.388885654883777576 ) ) ;
#5428 = ORIENTED_EDGE ( 'NONE', *, *, #29288, .F. ) ;
#5429 = CARTESIAN_POINT ( 'NONE',  ( 125.9568481442452850, -3.505236298600246325, -18.68346056562440793 ) ) ;
#5430 = CARTESIAN_POINT ( 'NONE',  ( 123.7022829359119811, -4.283928203966213211, -7.183505701512925334 ) ) ;
#5431 = CARTESIAN_POINT ( 'NONE',  ( 121.7575954359119805, -11.07370829466463569, -12.81314460846529002 ) ) ;
#5432 = FACE_OUTER_BOUND ( 'NONE', #37320, .T. ) ;
#5433 = CARTESIAN_POINT ( 'NONE',  ( 109.3018640045248304, 0.1403307496149616695, -15.46607636864997204 ) ) ;
#5434 = ORIENTED_EDGE ( 'NONE', *, *, #42931, .T. ) ;
#5435 = CARTESIAN_POINT ( 'NONE',  ( 120.1140014775786398, -1.561330072975668504, -17.79121239304076951 ) ) ;
#5436 = CARTESIAN_POINT ( 'NONE',  ( 123.9146881442452894, -10.15424416112533912, -14.75197769757731336 ) ) ;
#5437 = CARTESIAN_POINT ( 'NONE',  ( 113.5904348109119866, -2.084020599724406786, -8.691656652584148546 ) ) ;
#5438 = DIRECTION ( 'NONE',  ( 0.07634843047859418697, 0.9970811988817437355, 0.000000000000000000 ) ) ;
#5439 = CARTESIAN_POINT ( 'NONE',  ( 74.69189222814998175, -41.76310523276723785, -47.71602681600972318 ) ) ;
#5440 = CARTESIAN_POINT ( 'NONE',  ( 116.1998614775786507, -10.63000616557722466, -14.87417383870573495 ) ) ;
#5441 = CARTESIAN_POINT ( 'NONE',  ( 112.4272546295247821, -4.863998795839590272, -18.39754474579285315 ) ) ;
#5442 = CARTESIAN_POINT ( 'NONE',  ( 125.5597614775786326, -1.561330072975669392, -17.79121239304076951 ) ) ;
#5443 = ORIENTED_EDGE ( 'NONE', *, *, #40728, .F. ) ;
#5444 = CARTESIAN_POINT ( 'NONE',  ( 113.0231681442453322, 0.9020085738987339008, -11.91225656197089222 ) ) ;
#5445 = CARTESIAN_POINT ( 'NONE',  ( 114.8384214775786489, -10.15424416112533912, -14.75197769757731336 ) ) ;
#5446 = PLANE ( 'NONE',  #10384 ) ;
#5447 = CARTESIAN_POINT ( 'NONE',  ( 126.2404814775786264, -0.8288870151387760510, -10.36305467784173118 ) ) ;
#5448 = VERTEX_POINT ( 'NONE', #2940 ) ;
#5449 = CARTESIAN_POINT ( 'NONE',  ( 120.3976348109119812, -1.834011780172310813, -8.268836392978581529 ) ) ;
#5450 = CARTESIAN_POINT ( 'NONE',  ( 70.19189222814998175, -61.33395589173655793, -37.73637771078311687 ) ) ;
#5451 = CARTESIAN_POINT ( 'NONE',  ( 120.0875454359120056, -10.25250061710389105, -12.88985647778275911 ) ) ;
#5452 = CARTESIAN_POINT ( 'NONE',  ( 115.3484820646196880, 0.6269505268395592079, -14.64321520033831447 ) ) ;
#5453 = LINE ( 'NONE', #19373, #38178 ) ;
#5454 = VECTOR ( 'NONE', #17973, 1000.000000000000227 ) ;
#5455 = CARTESIAN_POINT ( 'NONE',  ( 115.5191414775786569, -6.222761293078241884, -8.102969835052219238 ) ) ;
#5456 = DIRECTION ( 'NONE',  ( 0.9609149988134837450, -0.1028163501681639419, 0.2570431154366518145 ) ) ;
#5457 = CARTESIAN_POINT ( 'NONE',  ( 125.3319029555670312, -2.398109642850332790, -20.05449063107751684 ) ) ;
#5458 = CARTESIAN_POINT ( 'NONE',  ( 113.0798948109119948, -8.899110576539710493, -16.42337572283490132 ) ) ;
#5459 = CARTESIAN_POINT ( 'NONE',  ( 126.0135748109119902, -1.833838273342660141, -17.42832698103878286 ) ) ;
#5460 = CARTESIAN_POINT ( 'NONE',  ( 121.2714235609119697, -9.645473719204776586, -14.86997237629376656 ) ) ;
#5461 = CARTESIAN_POINT ( 'NONE',  ( 112.7395348109119766, -5.638512984488999180, -18.83840828888717311 ) ) ;
#5462 = CARTESIAN_POINT ( 'NONE',  ( 116.6536748109119941, -10.15424416112533912, -14.75197769757731336 ) ) ;
#5463 = CARTESIAN_POINT ( 'NONE',  ( 123.5176014775786228, -9.261995988541697145, -16.69588392320189030 ) ) ;
#5464 = CARTESIAN_POINT ( 'NONE',  ( 120.7947214775786193, -9.261995988541697145, -16.69588392320189030 ) ) ;
#5465 = ORIENTED_EDGE ( 'NONE', *, *, #10853, .T. ) ;
#5466 = CARTESIAN_POINT ( 'NONE',  ( 126.5010429760476995, -8.564733770033562621, -16.96217817777857917 ) ) ;
#5467 = CARTESIAN_POINT ( 'NONE',  ( 109.7185827545247889, -2.477300249445798297, -19.15521520033831138 ) ) ;
#5468 = CARTESIAN_POINT ( 'NONE',  ( 108.1906140045248463, 0.1403307496149616695, -15.46607636864997204 ) ) ;
#5469 = CARTESIAN_POINT ( 'NONE',  ( 109.9269421295247753, -9.868328341294093420, -13.39321520033831447 ) ) ;
#5470 = CARTESIAN_POINT ( 'NONE',  ( 126.4915402333597001, -9.824595045050944719, -12.06033286554019135 ) ) ;
#5471 = CARTESIAN_POINT ( 'NONE',  ( 119.3198281442452924, 0.5811942927096110934, -14.16772938898807510 ) ) ;
#5472 = ORIENTED_EDGE ( 'NONE', *, *, #37008, .T. ) ;
#5473 = CARTESIAN_POINT ( 'NONE',  ( 125.1645598511810817, -9.397726027288767270, -19.25909742224127186 ) ) ;
#5474 = CARTESIAN_POINT ( 'NONE',  ( 2.384484203314607420, -10.01861149699890063, -17.89321520033831447 ) ) ;
#5475 = CARTESIAN_POINT ( 'NONE',  ( 124.6329298793804981, -2.191907684172563986, -18.20049396185734025 ) ) ;
#5476 = CARTESIAN_POINT ( 'NONE',  ( 114.1577014775786552, -3.505236298600246325, -18.68346056562440793 ) ) ;
#5477 = EDGE_CURVE ( 'NONE', #15102, #32667, #17093, .T. ) ;
#5478 = CARTESIAN_POINT ( 'NONE',  ( 119.0929214775786278, -5.638512984488999180, -18.83840828888717311 ) ) ;
#5479 = CARTESIAN_POINT ( 'NONE',  ( 108.3989733795248753, -8.938348069036489818, -17.46756447353520159 ) ) ;
#5480 = CARTESIAN_POINT ( 'NONE',  ( 119.3437409388149462, -2.287189184988710267, -18.07361239780447448 ) ) ;
#5481 = AXIS2_PLACEMENT_3D ( 'NONE', #3668, #41768, #27637 ) ;
#5482 = ORIENTED_EDGE ( 'NONE', *, *, #3588, .T. ) ;
#5483 = CARTESIAN_POINT ( 'NONE',  ( 120.7947214775786193, -0.8288870151387742746, -10.36305467784173473 ) ) ;
#5484 = CARTESIAN_POINT ( 'NONE',  ( 121.0216281442452981, -7.894159318335828068, -9.358103419637847864 ) ) ;
#5485 = CARTESIAN_POINT ( 'NONE',  ( 120.2274548109119934, 0.5811942927096110934, -14.16772938898807510 ) ) ;
#5486 = CARTESIAN_POINT ( 'NONE',  ( 90.15753105894957287, -11.66076665495339348, -14.14321520033831625 ) ) ;
#5487 = CARTESIAN_POINT ( 'NONE',  ( 113.8740681442453138, 0.5811942927096154232, -14.16772938898807155 ) ) ;
#5488 = CARTESIAN_POINT ( 'NONE',  ( 136.4689272580752686, -7.050714571525749541, -18.72418924296322729 ) ) ;
#5489 = CARTESIAN_POINT ( 'NONE',  ( 124.1415948109119540, -3.505236298600246325, -18.68346056562440793 ) ) ;
#5490 = CARTESIAN_POINT ( 'NONE',  ( 118.6391081442452986, -5.574606645277164318, -18.38911715685844683 ) ) ;
#5491 = ORIENTED_EDGE ( 'NONE', *, *, #35754, .T. ) ;
#5492 = CARTESIAN_POINT ( 'NONE',  ( 123.3550173109119612, 0.2312338769422704887, -16.08380026872395874 ) ) ;
#5493 = CARTESIAN_POINT ( 'NONE',  ( 114.3846081442453197, -10.63000616557722466, -14.87417383870573495 ) ) ;
#5494 = CARTESIAN_POINT ( 'NONE',  ( 122.6667014775786413, -2.084020599724406786, -8.691656652584148546 ) ) ;
#5495 = VERTEX_POINT ( 'NONE', #2712 ) ;
#5496 = CARTESIAN_POINT ( 'NONE',  ( 121.4797829359119987, -5.367793381288652910, -18.78638297431638904 ) ) ;
#5497 = CARTESIAN_POINT ( 'NONE',  ( 119.0929214775786278, -5.638512984488999180, -18.83840828888717311 ) ) ;
#5498 = CARTESIAN_POINT ( 'NONE',  ( 112.9134265045247645, -7.250697342233347165, -19.15521520033831138 ) ) ;
#5499 = CARTESIAN_POINT ( 'NONE',  ( 116.2565881442453133, -0.8288870151387760510, -10.36305467784173118 ) ) ;
#5500 = EDGE_CURVE ( 'NONE', #36439, #7248, #13445, .T. ) ;
#5501 = ORIENTED_EDGE ( 'NONE', *, *, #32837, .T. ) ;
#5502 = ORIENTED_EDGE ( 'NONE', *, *, #2742, .T. ) ;
#5503 = CARTESIAN_POINT ( 'NONE',  ( 120.8514481442452961, -2.084020599724406786, -8.691656652584148546 ) ) ;
#5504 = CARTESIAN_POINT ( 'NONE',  ( 122.1561614775786353, -8.899110576539710493, -16.42337572283490132 ) ) ;
#5505 =( BOUNDED_SURFACE ( )  B_SPLINE_SURFACE ( 1, 2, ( 
 ( #5855, #16136, #43954, #19328, #19778, #40534, #33660, #23662, #44638, #13403, #16360, #37548, #16595, #12950, #40997, #40759, #6088 ),
 ( #41222, #23433, #30488, #13174, #27076, #6321, #2895, #27305, #9980, #6996, #24762, #3124, #38217, #17048, #20908, #41668, #28416 ) ),
 .UNSPECIFIED., .F., .F., .F. ) 
 B_SPLINE_SURFACE_WITH_KNOTS ( ( 2, 2 ),
 ( 3, 2, 2, 2, 2, 2, 2, 2, 3 ),
 ( 0.000000000000000000, 1.000000000000000000 ),
 ( 0.000000000000000000, 0.1250000000000000000, 0.2500000000000000000, 0.3750000000000000000, 0.5000000000000000000, 0.6250000000000000000, 0.7500000000000000000, 0.8750000000000000000, 1.000000000000000000 ),
 .UNSPECIFIED. ) 
 GEOMETRIC_REPRESENTATION_ITEM ( )  RATIONAL_B_SPLINE_SURFACE ( (
 ( 1.000000000000000000, 0.9238795325112869605, 1.000000000000000000, 0.9238795325112869605, 1.000000000000000000, 0.9238795325112869605, 1.000000000000000000, 0.9238795325112869605, 1.000000000000000000, 0.9238795325112869605, 1.000000000000000000, 0.9238795325112869605, 1.000000000000000000, 0.9238795325112869605, 1.000000000000000000, 0.9238795325112869605, 1.000000000000000000),
 ( 1.000000000000000000, 0.9238795325112869605, 1.000000000000000000, 0.9238795325112869605, 1.000000000000000000, 0.9238795325112869605, 1.000000000000000000, 0.9238795325112869605, 1.000000000000000000, 0.9238795325112869605, 1.000000000000000000, 0.9238795325112869605, 1.000000000000000000, 0.9238795325112869605, 1.000000000000000000, 0.9238795325112869605, 1.000000000000000000) ) ) 
 REPRESENTATION_ITEM ( '' )  SURFACE ( )  );
#5506 = CARTESIAN_POINT ( 'NONE',  ( 65.62646388487864613, -15.45076938567549263, -16.39321520033831447 ) ) ;
#5507 = ADVANCED_FACE ( 'NONE', ( #9338 ), #30760, .T. ) ;
#5508 = CARTESIAN_POINT ( 'NONE',  ( 71.02242295334774269, -59.90284381096115851, -40.26874551563744831 ) ) ;
#5509 = EDGE_CURVE ( 'NONE', #7030, #25472, #20059, .T. ) ;
#5510 = CARTESIAN_POINT ( 'NONE',  ( 118.2420214775786320, -3.383040157471821630, -19.15922257007629170 ) ) ;
#5511 = DIRECTION ( 'NONE',  ( -0.2768435750659241079, -0.3568721902840695792, 0.8921882507333129819 ) ) ;
#5512 = CARTESIAN_POINT ( 'NONE',  ( 116.4834948109119779, -1.561330072975668504, -17.79121239304076951 ) ) ;
#5514 = CARTESIAN_POINT ( 'NONE',  ( 116.8805814775786445, -3.505236298600246325, -18.68346056562440793 ) ) ;
#5513 = CARTESIAN_POINT ( 'NONE',  ( 115.6893214775786447, 0.5811942927096154232, -14.16772938898807155 ) ) ;
#5515 = CARTESIAN_POINT ( 'NONE',  ( 121.3619881442452879, -5.574606645277164318, -18.38911715685844683 ) ) ;
#5516 = CARTESIAN_POINT ( 'NONE',  ( 112.6828081442453282, -7.893985811506177619, -18.51759400769804742 ) ) ;
#5517 = VERTEX_POINT ( 'NONE', #31203 ) ;
#5518 = VECTOR ( 'NONE', #6984, 1000.000000000000114 ) ;
#5519 = CARTESIAN_POINT ( 'NONE',  ( 124.1983214775786166, -1.833838273342659697, -17.42832698103878286 ) ) ;
#5520 = EDGE_CURVE ( 'NONE', #24697, #25472, #15787, .T. ) ;
#5521 = CARTESIAN_POINT ( 'NONE',  ( 113.9371133359170614, -2.311015703046748193, -18.04188382666269064 ) ) ;
#5522 = CARTESIAN_POINT ( 'NONE',  ( 112.2188952545247531, 0.8980012041604421569, -11.00651665394454071 ) ) ;
#5523 = CARTESIAN_POINT ( 'NONE',  ( 114.9275671295247889, 0.1403307496149613920, -13.39321520033831447 ) ) ;
#5524 = CARTESIAN_POINT ( 'NONE',  ( 113.4690515045247992, -2.477300249445798297, -7.631215200338321125 ) ) ;
#5525 = CARTESIAN_POINT ( 'NONE',  ( 118.1852948109119836, -5.638512984488999180, -18.83840828888717311 ) ) ;
#5526 = VERTEX_POINT ( 'NONE', #34609 ) ;
#5527 = EDGE_CURVE ( 'NONE', #11850, #27501, #44454, .T. ) ;
#5528 = CARTESIAN_POINT ( 'NONE',  ( 122.6667014775786413, -7.893985811506177619, -18.51759400769804742 ) ) ;
#5529 = CARTESIAN_POINT ( 'NONE',  ( 70.19189222814998175, -56.12358456014947450, -35.65224734057483857 ) ) ;
#5530 = CARTESIAN_POINT ( 'NONE',  ( 108.2600671295247992, -10.62599879583958540, -13.39321520033831447 ) ) ;
#5531 = CARTESIAN_POINT ( 'NONE',  ( 120.9649014775786355, -3.383040157471821630, -19.15922257007629170 ) ) ;
#5532 = EDGE_CURVE ( 'NONE', #574, #1124, #41996, .T. ) ;
#5533 = EDGE_CURVE ( 'NONE', #10907, #22858, #17264, .T. ) ;
#5534 = CARTESIAN_POINT ( 'NONE',  ( 116.0296814775786345, -8.166667518702817929, -8.995218007635861213 ) ) ;
#5535 = CARTESIAN_POINT ( 'NONE',  ( 64.28574602589941378, -2.825497480247340043, -18.75418257877172934 ) ) ;
#5536 = CARTESIAN_POINT ( 'NONE',  ( 116.9293938463531219, -11.59383920986051919, -5.945542079317219120 ) ) ;
#5537 = ORIENTED_EDGE ( 'NONE', *, *, #18972, .F. ) ;
#5538 = CARTESIAN_POINT ( 'NONE',  ( -2.556913038227175416, -7.051771562855549291, -7.494178442794038553 ) ) ;
#5539 = CARTESIAN_POINT ( 'NONE',  ( 109.2294825911599645, -9.927280692135916240, -15.47594509028579779 ) ) ;
#5540 = CARTESIAN_POINT ( 'NONE',  ( 125.4463081442452932, -4.153390946401325223, -8.397313243818185668 ) ) ;
#5541 = AXIS2_PLACEMENT_3D ( 'NONE', #18284, #7567, #10778 ) ;
#5542 = CARTESIAN_POINT ( 'NONE',  ( 113.5385046295247804, -4.863998795839590272, -18.39754474579285315 ) ) ;
#5543 = CARTESIAN_POINT ( 'NONE',  ( 109.1629577545248395, -2.791137627527939813, -18.39754474579286025 ) ) ;
#5544 = CARTESIAN_POINT ( 'NONE',  ( 119.6601881442453106, -1.833838273342659253, -17.42832698103878286 ) ) ;
#5545 = PLANE ( 'NONE',  #17569 ) ;
#5546 = CARTESIAN_POINT ( 'NONE',  ( 70.92670879693453401, -25.79851902929913976, -5.473826388607135662 ) ) ;
#5547 = CARTESIAN_POINT ( 'NONE',  ( 114.2711548109119803, -0.1624402480850797581, -16.17319339645315424 ) ) ;
#5548 = CARTESIAN_POINT ( 'NONE',  ( 124.4819548109119722, -7.893985811506177619, -18.51759400769804742 ) ) ;
#5549 = ORIENTED_EDGE ( 'NONE', *, *, #5598, .F. ) ;
#5550 = AXIS2_PLACEMENT_3D ( 'NONE', #36411, #32984, #26168 ) ;
#5551 = CARTESIAN_POINT ( 'NONE',  ( 120.7379948109119709, 0.4262465694468514643, -12.03445270309931736 ) ) ;
#5552 = CARTESIAN_POINT ( 'NONE',  ( 113.5904348109119866, -7.893985811506177619, -18.51759400769804742 ) ) ;
#5553 = CARTESIAN_POINT ( 'NONE',  ( 120.7947214775786193, -9.261995988541697145, -16.69588392320189030 ) ) ;
#5554 = CARTESIAN_POINT ( 'NONE',  ( 123.4608748109119745, 0.4262465694468514643, -12.03445270309931736 ) ) ;
#5555 = ORIENTED_EDGE ( 'NONE', *, *, #11905, .T. ) ;
#5556 = DIRECTION ( 'NONE',  ( -0.2768435750659241079, -0.3568721902840695792, 0.8921882507333129819 ) ) ;
#5557 = AXIS2_PLACEMENT_3D ( 'NONE', #16641, #22622, #25606 ) ;
#5558 = CARTESIAN_POINT ( 'NONE',  ( 124.8790414775786246, -0.4660016031367893996, -10.09054647747474043 ) ) ;
#5559 = CARTESIAN_POINT ( 'NONE',  ( 125.1433143116104389, -7.968577257696042970, -6.639574498171168848 ) ) ;
#5560 = CARTESIAN_POINT ( 'NONE',  ( 111.5482748109120053, -0.1624402480850797581, -16.17319339645315424 ) ) ;
#5561 = CARTESIAN_POINT ( 'NONE',  ( 107.7044421295247929, 0.8980012041604618078, -13.39321520033831447 ) ) ;
#5562 = CARTESIAN_POINT ( 'NONE',  ( 120.8547048109119686, -2.527210466738041728, -8.967976844669124148 ) ) ;
#5563 = CARTESIAN_POINT ( 'NONE',  ( 127.9028083230502375, -3.116567687765117167, -14.47105017736742205 ) ) ;
#5564 = CARTESIAN_POINT ( 'NONE',  ( 109.6491296295247793, -4.863998795839590272, -8.388885654883775800 ) ) ;
#5565 = AXIS2_PLACEMENT_3D ( 'NONE', #34275, #2819, #9907 ) ;
#5566 = CARTESIAN_POINT ( 'NONE',  ( 120.6812681442452941, 0.1319031606808879209, -14.10382304977623669 ) ) ;
#5567 = CARTESIAN_POINT ( 'NONE',  ( 125.4463081442452932, -5.638512984488999180, -18.83840828888717311 ) ) ;
#5568 = CARTESIAN_POINT ( 'NONE',  ( 126.3965902706515578, -6.074779341511876041, -18.33615407855781854 ) ) ;
#5569 = ORIENTED_EDGE ( 'NONE', *, *, #37271, .T. ) ;
#5570 = CARTESIAN_POINT ( 'NONE',  ( 116.1777233795247781, -1.325403438956436419, -9.854619843455211026 ) ) ;
#5571 = CARTESIAN_POINT ( 'NONE',  ( 117.9583881442453048, 0.1319031606808879209, -14.10382304977623669 ) ) ;
#5572 = DIRECTION ( 'NONE',  ( 0.5735764363510498232, -0.3127926500124802445, 0.7570804645221007600 ) ) ;
#5573 = EDGE_CURVE ( 'NONE', #40242, #25201, #37817, .T. ) ;
#5574 = CIRCLE ( 'NONE', #38355, 1.199999999999999512 ) ;
#5575 = CARTESIAN_POINT ( 'NONE',  ( 67.52182966331936598, -0.2245269270738840806, -10.39321520033831980 ) ) ;
#5576 = CARTESIAN_POINT ( 'NONE',  ( 124.1407619144190306, -1.220279397241718966, -16.99638242193886484 ) ) ;
#5577 = CARTESIAN_POINT ( 'NONE',  ( 123.1772414775786189, -4.089484607189486809, -7.948022111789456723 ) ) ;
#5578 = CARTESIAN_POINT ( 'NONE',  ( 123.2339681442453241, -3.505236298600246325, -18.68346056562440793 ) ) ;
#5579 = ORIENTED_EDGE ( 'NONE', *, *, #42493, .T. ) ;
#5580 = CARTESIAN_POINT ( 'NONE',  ( 110.3436454522301915, 0.1168444861213632779, -14.64321520033833934 ) ) ;
#5581 = CARTESIAN_POINT ( 'NONE',  ( 126.3230600034192292, 0.06859183521943734707, -14.48755961147212368 ) ) ;
#5582 = CARTESIAN_POINT ( 'NONE',  ( 108.3989733795247759, -1.325403438956436419, -9.854619843455211026 ) ) ;
#5583 = ADVANCED_FACE ( 'NONE', ( #19825 ), #33713, .F. ) ;
#5584 = CARTESIAN_POINT ( 'NONE',  ( 122.1561614775786353, -8.899110576539710493, -16.42337572283490132 ) ) ;
#5585 = VECTOR ( 'NONE', #23015, 1000.000000000000227 ) ;
#5586 = CARTESIAN_POINT ( 'NONE',  ( 120.1707281442453166, -9.565557343593413364, -10.61323700422348004 ) ) ;
#5587 = CARTESIAN_POINT ( 'NONE',  ( 125.1028739313169496, 1.212150000717685305, -17.73793242834041095 ) ) ;
#5588 = CARTESIAN_POINT ( 'NONE',  ( 113.7468640045248236, 0.1403307496149616695, -15.46607636864997204 ) ) ;
#5589 = DIRECTION ( 'NONE',  ( 0.000000000000000000, 0.000000000000000000, 1.000000000000000000 ) ) ;
#5590 = CARTESIAN_POINT ( 'NONE',  ( 71.02242295334774269, -50.61806574177743556, -36.55486665304579930 ) ) ;
#5591 = DIRECTION ( 'NONE',  ( -0.2407039305251456596, 0.3604685577742790525, -0.9011792478113757054 ) ) ;
#5592 = CARTESIAN_POINT ( 'NONE',  ( 109.2324108795247923, -8.938348069036489818, -9.318865927141430916 ) ) ;
#5593 = CARTESIAN_POINT ( 'NONE',  ( -13.53629081928688649, -4.821193161180528541, -18.04471655251912665 ) ) ;
#5594 = CARTESIAN_POINT ( 'NONE',  ( 115.6915515045247531, -2.477300249445798297, -7.631215200338321125 ) ) ;
#5595 = CARTESIAN_POINT ( 'NONE',  ( 121.9292548109119849, -1.561330072975668948, -17.79121239304076951 ) ) ;
#5596 = CARTESIAN_POINT ( 'NONE',  ( 121.3619881442452879, -4.089484607189486809, -7.948022111789456723 ) ) ;
#5597 = CARTESIAN_POINT ( 'NONE',  ( 108.3989733795248753, -8.938348069036489818, -17.46756447353520159 ) ) ;
#5598 = EDGE_CURVE ( 'NONE', #38815, #28999, #16638, .T. ) ;
#5599 = CARTESIAN_POINT ( 'NONE',  ( 115.4056881442453459, -7.893985811506177619, -18.51759400769804742 ) ) ;
#5600 = CARTESIAN_POINT ( 'NONE',  ( 113.8740681442453138, 0.5811942927096154232, -14.16772938898807155 ) ) ;
#5601 = ORIENTED_EDGE ( 'NONE', *, *, #10985, .T. ) ;
#5602 = DIRECTION ( 'NONE',  ( -0.000000000000000000, -0.9284778069183721172, -0.3713878862591650232 ) ) ;
#5603 = CARTESIAN_POINT ( 'NONE',  ( 123.1205148109119563, -1.834011780172310813, -8.268836392978581529 ) ) ;
#5604 = CARTESIAN_POINT ( 'NONE',  ( 120.2841814775786276, 0.9020085738987339008, -11.91225656197089222 ) ) ;
#5605 = CARTESIAN_POINT ( 'NONE',  ( 125.7299414775786346, -10.15424416112533912, -14.75197769757731336 ) ) ;
#5606 = AXIS2_PLACEMENT_3D ( 'NONE', #14939, #20888, #34766 ) ;
#5607 = CARTESIAN_POINT ( 'NONE',  ( 112.1722681442453222, -8.899110576539710493, -16.42337572283490132 ) ) ;
#5608 = CARTESIAN_POINT ( 'NONE',  ( 115.8027748109119841, -8.899110576539710493, -16.42337572283490132 ) ) ;
#5609 = CARTESIAN_POINT ( 'NONE',  ( 124.4252281442452812, -9.261995988541697145, -16.69588392320189030 ) ) ;
#5610 = CIRCLE ( 'NONE', #19454, 2.000000000000000444 ) ;
#5611 = CARTESIAN_POINT ( 'NONE',  ( 110.2742077545248094, -7.250697342233347165, -7.631215200338321125 ) ) ;
#5612 = CARTESIAN_POINT ( 'NONE',  ( 120.9649014775786355, -6.222761293078241884, -8.102969835052219238 ) ) ;
#5613 = CARTESIAN_POINT ( 'NONE',  ( 110.2047546295247855, -4.863998795839590272, -7.631215200338315796 ) ) ;
#5614 = DIRECTION ( 'NONE',  ( 1.000000000000000000, 0.000000000000000000, -0.000000000000000000 ) ) ;
#5615 = ORIENTED_EDGE ( 'NONE', *, *, #38993, .F. ) ;
#5616 = VECTOR ( 'NONE', #33420, 1000.000000000000000 ) ;
#5617 = CARTESIAN_POINT ( 'NONE',  ( 121.0024232127138504, -2.191907684172563986, -18.20049396185734025 ) ) ;
#5618 = CARTESIAN_POINT ( 'NONE',  ( 123.1772414775786189, -4.089484607189486809, -7.948022111789456723 ) ) ;
#5619 = DIRECTION ( 'NONE',  ( -0.9609149988134837450, 0.1028163501681639419, -0.2570431154366518145 ) ) ;
#5620 = CARTESIAN_POINT ( 'NONE',  ( 125.3303382280792846, 2.061758691653259312, -11.74840549411501556 ) ) ;
#5621 = CARTESIAN_POINT ( 'NONE',  ( 115.3446837908067835, 0.5115630086001619059, -12.14321520033831625 ) ) ;
#5622 = CARTESIAN_POINT ( 'NONE',  ( 66.99801899372408798, -0.07922336130813037447, -16.39321520033831447 ) ) ;
#5623 = DIRECTION ( 'NONE',  ( 1.000000000000000000, 0.000000000000000000, -0.000000000000000000 ) ) ;
#5624 = CARTESIAN_POINT ( 'NONE',  ( 122.9503348109119827, -9.859900752359378018, -12.68260735090039759 ) ) ;
#5625 = ADVANCED_FACE ( 'NONE', ( #12993 ), #26889, .T. ) ;
#5626 = CARTESIAN_POINT ( 'NONE',  ( 121.8270485609119760, -10.36940331770107093, -15.09355782777061350 ) ) ;
#5627 = CARTESIAN_POINT ( 'NONE',  ( 123.3474214775786209, -0.1624402480850797581, -16.17319339645315424 ) ) ;
#5628 = CARTESIAN_POINT ( 'NONE',  ( 125.2572271076672905, -11.54560042640431838, -16.20890238838691744 ) ) ;
#5630 = CARTESIAN_POINT ( 'NONE',  ( 125.6732148109119862, 0.5811942927096110934, -14.16772938898807510 ) ) ;
#5629 = AXIS2_PLACEMENT_3D ( 'NONE', #31599, #592, #42326 ) ;
#5631 = CARTESIAN_POINT ( 'NONE',  ( 117.0507614775786465, 0.1319031606808879209, -14.10382304977623669 ) ) ;
#5632 = CARTESIAN_POINT ( 'NONE',  ( 119.7434548109119703, -6.019411175499098654, -18.97193101650639591 ) ) ;
#5633 = ORIENTED_EDGE ( 'NONE', *, *, #8889, .F. ) ;
#5634 = CARTESIAN_POINT ( 'NONE',  ( 122.8368814775786291, -1.561330072975668948, -17.79121239304076951 ) ) ;
#5635 = CARTESIAN_POINT ( 'NONE',  ( 117.2776681442452968, -5.638512984488999180, -18.83840828888717311 ) ) ;
#5636 = CARTESIAN_POINT ( 'NONE',  ( 114.0246765045248196, -2.791137627527939813, -8.388885654883777576 ) ) ;
#5637 = DIRECTION ( 'NONE',  ( 1.000000000000000000, 0.000000000000000000, 0.000000000000000000 ) ) ;
#5638 = CARTESIAN_POINT ( 'NONE',  ( 122.7234281442452755, -4.153390946401325223, -8.397313243818185668 ) ) ;
#5639 = CARTESIAN_POINT ( 'NONE',  ( 123.1205148109119563, -1.834011780172310813, -8.268836392978581529 ) ) ;
#5640 = CARTESIAN_POINT ( 'NONE',  ( 115.0664733795247798, -8.938348069036489818, -17.46756447353520159 ) ) ;
#5641 = CARTESIAN_POINT ( 'NONE',  ( 108.6073327545248048, -6.936859964151250502, -8.388885654883777576 ) ) ;
#5642 = FACE_OUTER_BOUND ( 'NONE', #15688, .T. ) ;
#5643 = CARTESIAN_POINT ( 'NONE',  ( 112.2289948109119848, -7.643976991954077427, -18.09477374809248928 ) ) ;
#5644 = CARTESIAN_POINT ( 'NONE',  ( 117.7882081442453170, -3.505236298600246325, -18.68346056562440793 ) ) ;
#5645 = EDGE_CURVE ( 'NONE', #11206, #31913, #30339, .T. ) ;
#5646 = CARTESIAN_POINT ( 'NONE',  ( 135.3184548109119874, -1.889072916127989776, -18.60376373290417362 ) ) ;
#5647 = CARTESIAN_POINT ( 'NONE',  ( 111.4549108795247747, -1.325403438956436419, -16.93181055722141792 ) ) ;
#5648 = VERTEX_POINT ( 'NONE', #9565 ) ;
#5649 = CARTESIAN_POINT ( 'NONE',  ( 123.6877814775786533, -6.222761293078241884, -8.102969835052219238 ) ) ;
#5650 = CARTESIAN_POINT ( 'NONE',  ( 119.9518141859119851, -8.321307733199551748, -9.223433127585318303 ) ) ;
#5651 = CARTESIAN_POINT ( 'NONE',  ( 122.5910329359119970, -4.283928203966213211, -7.183505701512925334 ) ) ;
#5652 = ORIENTED_EDGE ( 'NONE', *, *, #40774, .F. ) ;
#5653 = CIRCLE ( 'NONE', #11500, 4.999999999999998224 ) ;
#5654 = LINE ( 'NONE', #33452, #2053 ) ;
#5655 = CARTESIAN_POINT ( 'NONE',  ( 84.49707967414211396, -27.84333996136784961, -14.15691383771150136 ) ) ;
#5656 = ORIENTED_EDGE ( 'NONE', *, *, #3397, .F. ) ;
#5657 = CARTESIAN_POINT ( 'NONE',  ( 118.6958348109119754, -6.344957434206665248, -7.627207830600338134 ) ) ;
#5658 = CARTESIAN_POINT ( 'NONE',  ( 125.4463081442452932, -4.153390946401325223, -8.397313243818185668 ) ) ;
#5659 = CARTESIAN_POINT ( 'NONE',  ( 114.4980614775786734, -2.084020599724406786, -8.691656652584148546 ) ) ;
#5660 =( LENGTH_UNIT ( ) NAMED_UNIT ( * ) SI_UNIT ( .MILLI., .METRE. ) );
#5661 = DIRECTION ( 'NONE',  ( 0.000000000000000000, -0.9284778069183722282, -0.3713878862591645791 ) ) ;
#5662 = CARTESIAN_POINT ( 'NONE',  ( 71.62231439647737830, -24.74987456741813929, -4.893215200338314474 ) ) ;
#5663 = CARTESIAN_POINT ( 'NONE',  ( 116.3133148109119759, -7.893985811506177619, -18.51759400769804742 ) ) ;
#5664 = CARTESIAN_POINT ( 'NONE',  ( 110.9687390045248350, -9.868328341294098749, -11.32035403202665869 ) ) ;
#5665 = VECTOR ( 'NONE', #35917, 1000.000000000000000 ) ;
#5666 = CARTESIAN_POINT ( 'NONE',  ( 123.1205148109119563, -1.834011780172310813, -8.268836392978581529 ) ) ;
#5667 = B_SPLINE_CURVE_WITH_KNOTS ( 'NONE', 3,
 ( #3734, #20856, #17657, #39073, #11267, #38604, #3957, #7380, #4415, #14234 ),
 .UNSPECIFIED., .F., .F.,
 ( 4, 3, 3, 4 ),
 ( 0.000000000000000000, 0.0002476487219222909880, 0.0004952974148303589856, 0.0009534114850261710648 ),
 .UNSPECIFIED. ) ;
#5668 = CARTESIAN_POINT ( 'NONE',  ( 86.75477599865929790, -25.99489077589524300, -13.39321520033831625 ) ) ;
#5669 = ORIENTED_EDGE ( 'NONE', *, *, #16988, .F. ) ;
#5670 = CARTESIAN_POINT ( 'NONE',  ( 115.4624148109119943, -5.638512984488999180, -18.83840828888717311 ) ) ;
#5671 = CARTESIAN_POINT ( 'NONE',  ( 114.6115148109119986, -6.222761293078241884, -8.102969835052219238 ) ) ;
#5672 = CARTESIAN_POINT ( 'NONE',  ( 126.3243314201013305, -5.189031759765639684, -18.43570266033291460 ) ) ;
#5673 = CARTESIAN_POINT ( 'NONE',  ( 112.0588148109119828, 0.5811942927096154232, -14.16772938898807155 ) ) ;
#5674 = EDGE_LOOP ( 'NONE', ( #31624, #17050, #3212, #38793, #42386, #13562, #29152 ) ) ;
#5675 = CARTESIAN_POINT ( 'NONE',  ( 120.1140014775786398, -1.561330072975668504, -17.79121239304076951 ) ) ;
#5676 = CARTESIAN_POINT ( 'NONE',  ( 69.36136150295220659, -101.1685209014307674, -50.56525720990386219 ) ) ;
#5677 = CARTESIAN_POINT ( 'NONE',  ( 115.8935686996681937, -1.172797794773246416, -17.05961127468924587 ) ) ;
#5678 = CARTESIAN_POINT ( 'NONE',  ( 112.1721994132789320, -8.900630651041904429, -16.42135045828372597 ) ) ;
#5679 = CARTESIAN_POINT ( 'NONE',  ( 136.5935259641903201, -2.727577936221012855, -8.099885892359873552 ) ) ;
#5680 = CARTESIAN_POINT ( 'NONE',  ( 113.7038881442453402, -6.222761293078241884, -8.102969835052219238 ) ) ;
#5681 = DIRECTION ( 'NONE',  ( 0.9609149988134843001, -0.1028163501681632064, 0.2570431154366505933 ) ) ;
#5682 = CARTESIAN_POINT ( 'NONE',  ( 125.3562121110092846, -2.843430562235182535, -20.14166698885114926 ) ) ;
#5683 = CARTESIAN_POINT ( 'NONE',  ( 117.0507614775786465, 0.1319031606808879209, -14.10382304977623669 ) ) ;
#5684 = CARTESIAN_POINT ( 'NONE',  ( 112.7962614775786676, -3.383040157471821630, -19.15922257007629170 ) ) ;
#5685 = CARTESIAN_POINT ( 'NONE',  ( 124.3968141859119783, -8.321307733199551748, -9.223433127585318303 ) ) ;
#5686 = CARTESIAN_POINT ( 'NONE',  ( 125.9568481442452850, -3.505236298600246325, -18.68346056562440793 ) ) ;
#5687 = CARTESIAN_POINT ( 'NONE',  ( 117.1642148109119859, -0.8288870151387760510, -10.36305467784173118 ) ) ;
#5688 = CARTESIAN_POINT ( 'NONE',  ( 122.8936081442453059, 0.2603800115204892296, -16.42320221600525088 ) ) ;
#5689 = CARTESIAN_POINT ( 'NONE',  ( 122.1561614775786353, -0.4660016031367893996, -10.09054647747474043 ) ) ;
#5690 = ORIENTED_EDGE ( 'NONE', *, *, #18587, .F. ) ;
#5691 = CARTESIAN_POINT ( 'NONE',  ( 115.0086014775786509, -4.089484607189486809, -7.948022111789456723 ) ) ;
#5692 = CARTESIAN_POINT ( 'NONE',  ( 111.2465515045248168, -2.477300249445798297, -7.631215200338321125 ) ) ;
#5693 = CARTESIAN_POINT ( 'NONE',  ( 112.2883483795247770, -8.402594152722688392, -16.93181055722141792 ) ) ;
#5694 = CARTESIAN_POINT ( 'NONE',  ( 108.1211608795247798, -1.325403438956436419, -16.93181055722141792 ) ) ;
#5695 = EDGE_CURVE ( 'NONE', #12923, #25838, #41270, .T. ) ;
#5696 = AXIS2_PLACEMENT_3D ( 'NONE', #25511, #36207, #36873 ) ;
#5697 = CARTESIAN_POINT ( 'NONE',  ( 109.8368621053768948, 0.3967854368540359999, -16.28112951403850772 ) ) ;
#5698 = CARTESIAN_POINT ( 'NONE',  ( 118.0151148109119816, -10.63000616557722466, -14.87417383870573495 ) ) ;
#5699 = ORIENTED_EDGE ( 'NONE', *, *, #41219, .F. ) ;
#5700 = CARTESIAN_POINT ( 'NONE',  ( 71.02242295334774269, -55.26045477636929348, -38.41180608434162025 ) ) ;
#5701 = PLANE ( 'NONE',  #40124 ) ;
#5702 = CARTESIAN_POINT ( 'NONE',  ( 120.6646509814547130, -2.395992375830759524, -17.92872468182853396 ) ) ;
#5703 = CARTESIAN_POINT ( 'NONE',  ( 113.5904348109119866, -2.084020599724406786, -8.691656652584148546 ) ) ;
#5704 = CARTESIAN_POINT ( 'NONE',  ( 106.7320983795247855, -8.402594152722688392, -16.93181055722141792 ) ) ;
#5705 = CARTESIAN_POINT ( 'NONE',  ( 118.3554748109119998, 0.2603800115204892296, -16.42320221600525088 ) ) ;
#5706 = CARTESIAN_POINT ( 'NONE',  ( 107.2877233795247776, -8.938348069036489818, -17.46756447353520159 ) ) ;
#5707 = DIRECTION ( 'NONE',  ( -1.387778780781445478E-15, -1.000000000000000000, 0.000000000000000000 ) ) ;
#5708 = ORIENTED_EDGE ( 'NONE', *, *, #1349, .F. ) ;
#5709 = CARTESIAN_POINT ( 'NONE',  ( 61.76986277844709861, -39.32091226840162079, -4.893215200338314474 ) ) ;
#5710 = CARTESIAN_POINT ( 'NONE',  ( 121.9859814775786333, -9.565557343593413364, -10.61323700422348004 ) ) ;
#5711 = CARTESIAN_POINT ( 'NONE',  ( 119.2063748109119814, -1.561330072975668504, -17.79121239304076951 ) ) ;
#5712 = CARTESIAN_POINT ( 'NONE',  ( 113.5337081442453240, -0.8288870151387760510, -10.36305467784173118 ) ) ;
#5713 = CARTESIAN_POINT ( 'NONE',  ( 116.4267681442453153, -3.383040157471821630, -19.15922257007629170 ) ) ;
#5714 = CARTESIAN_POINT ( 'NONE',  ( 125.3328548109119964, -9.261995988541029234, -16.69588392320277848 ) ) ;
#5715 = CARTESIAN_POINT ( 'NONE',  ( 122.6099748109119929, -0.8288870151387760510, -10.36305467784173118 ) ) ;
#5716 = CARTESIAN_POINT ( 'NONE',  ( 119.8870948109119752, -0.8288870151387760510, -10.36305467784173118 ) ) ;
#5717 = ORIENTED_EDGE ( 'NONE', *, *, #23481, .T. ) ;
#5718 = CARTESIAN_POINT ( 'NONE',  ( 123.4939235609119663, 0.6414057260225851653, -11.69287257290600657 ) ) ;
#5719 = CARTESIAN_POINT ( 'NONE',  ( 114.4413348109119823, -9.261995988541697145, -16.69588392320189030 ) ) ;
#5720 = CARTESIAN_POINT ( 'NONE',  ( 122.4397948109119767, -0.1624402480850797581, -16.17319339645315424 ) ) ;
#5721 = ORIENTED_EDGE ( 'NONE', *, *, #22277, .T. ) ;
#5722 = CARTESIAN_POINT ( 'NONE',  ( 120.9241579359119925, -4.360204210389833968, -8.000047426360245240 ) ) ;
#5723 = CARTESIAN_POINT ( 'NONE',  ( 118.6958348109119754, -6.344957434206665248, -7.627207830600338134 ) ) ;
#5724 = CARTESIAN_POINT ( 'NONE',  ( 112.8439733795247832, -8.938348069036489818, -17.46756447353520159 ) ) ;
#5725 = CARTESIAN_POINT ( 'NONE',  ( 115.0653281442453277, -3.505236298600246325, -18.68346056562440793 ) ) ;
#5726 = ORIENTED_EDGE ( 'NONE', *, *, #13331, .T. ) ;
#5727 = ORIENTED_EDGE ( 'NONE', *, *, #36629, .T. ) ;
#5728 = CARTESIAN_POINT ( 'NONE',  ( 125.0492214775786266, -3.505236298600246325, -18.68346056562440793 ) ) ;
#5729 = CARTESIAN_POINT ( 'NONE',  ( 119.7169148109119874, -0.1624402480850797581, -16.17319339645315424 ) ) ;
#5730 = DIRECTION ( 'NONE',  ( 0.000000000000000000, 0.000000000000000000, 1.000000000000000000 ) ) ;
#5731 = B_SPLINE_CURVE_WITH_KNOTS ( 'NONE', 3,
 ( #26165, #8615, #33210, #19324, #40069, #29584, #22513, #30258, #2203, #43949 ),
 .UNSPECIFIED., .F., .F.,
 ( 4, 3, 3, 4 ),
 ( 0.000000000000000000, 0.0002476486447138780394, 0.0004952972925464190672, 0.0009604418836934719428 ),
 .UNSPECIFIED. ) ;
#5732 = DIRECTION ( 'NONE',  ( 4.295035233247849253E-16, 0.3713878862591650232, -0.9284778069183718952 ) ) ;
#5733 = CARTESIAN_POINT ( 'NONE',  ( 119.6034614775786196, -6.344957434206665248, -7.627207830600338134 ) ) ;
#5734 = CARTESIAN_POINT ( 'NONE',  ( 105.9681140045248355, -10.62599879583958717, -11.00651665394454604 ) ) ;
#5735 = CARTESIAN_POINT ( 'NONE',  ( 117.3911214775786505, -1.561330072975668504, -17.79121239304076951 ) ) ;
#5737 = CARTESIAN_POINT ( 'NONE',  ( 116.1431348109119881, 0.1319031606808879209, -14.10382304977623669 ) ) ;
#5736 = CARTESIAN_POINT ( 'NONE',  ( 116.8805814775786445, -6.344957434206662583, -7.627207830600332805 ) ) ;
#5738 = CARTESIAN_POINT ( 'NONE',  ( 123.6310548109119765, -4.153390946401325223, -8.397313243818185668 ) ) ;
#5739 = CARTESIAN_POINT ( 'NONE',  ( 111.9645664091100912, -0.9924539043446216624, -17.29976612834909133 ) ) ;
#5740 = ORIENTED_EDGE ( 'NONE', *, *, #19748, .F. ) ;
#5741 = CARTESIAN_POINT ( 'NONE',  ( 124.4819548109119722, -2.084020599724406786, -8.691656652584148546 ) ) ;
#5742 = DIRECTION ( 'NONE',  ( 0.000000000000000000, 0.000000000000000000, 1.000000000000000000 ) ) ;
#5743 = CARTESIAN_POINT ( 'NONE',  ( 114.4413952545248350, 0.8980012041604421569, -11.00651665394454071 ) ) ;
#5744 = CARTESIAN_POINT ( 'NONE',  ( 112.9134265045247645, -2.791137627527939813, -8.388885654883777576 ) ) ;
#5745 = CARTESIAN_POINT ( 'NONE',  ( 113.9552233795247815, -8.938348069036489818, -17.46756447353520159 ) ) ;
#5746 = CARTESIAN_POINT ( 'NONE',  ( 120.6245414775786458, -9.988377603198976828, -10.36322818467138340 ) ) ;
#5747 = B_SPLINE_CURVE_WITH_KNOTS ( 'NONE', 3,
 ( #11472, #26042, #1194, #11915, #32421, #1630, #42480, #29237, #12139, #15107 ),
 .UNSPECIFIED., .F., .F.,
 ( 4, 3, 3, 4 ),
 ( 0.000000000000000000, 0.0001671877560958109985, 0.0003343755126086570017, 0.0006438490228505480001 ),
 .UNSPECIFIED. ) ;
#5748 = ORIENTED_EDGE ( 'NONE', *, *, #7032, .T. ) ;
#5749 = CARTESIAN_POINT ( 'NONE',  ( 120.5110881442453206, -6.344957434206665248, -7.627207830600338134 ) ) ;
#5750 = CARTESIAN_POINT ( 'NONE',  ( 112.3991748109119868, -1.833838273342658809, -17.42832698103878286 ) ) ;
#5751 = FACE_OUTER_BOUND ( 'NONE', #15622, .T. ) ;
#5752 = CARTESIAN_POINT ( 'NONE',  ( 118.9227414775786400, -10.63000616557722466, -14.87417383870573495 ) ) ;
#5753 = CARTESIAN_POINT ( 'NONE',  ( 121.1350814775786233, 0.5811942927096110934, -14.16772938898807510 ) ) ;
#5754 = CARTESIAN_POINT ( 'NONE',  ( 62.61854009670715726, -3.462514682154532952, -19.20073182371810461 ) ) ;
#5755 = CARTESIAN_POINT ( 'NONE',  ( 116.2659068881580708, -12.01880880694303855, -6.893215200338315363 ) ) ;
#5756 = CARTESIAN_POINT ( 'NONE',  ( 121.1325173109119788, -9.289237151508434209, -11.05642687123711276 ) ) ;
#5757 = ADVANCED_FACE ( 'NONE', ( #34389 ), #22331, .T. ) ;
#5758 = ORIENTED_EDGE ( 'NONE', *, *, #21801, .T. ) ;
#5759 = CARTESIAN_POINT ( 'NONE',  ( 151.2860562277021472, -4.863998795839242995, -13.39321520033831447 ) ) ;
#5760 = CARTESIAN_POINT ( 'NONE',  ( 112.7395348109119766, -4.153390946401321671, -8.397313243818183892 ) ) ;
#5761 = CARTESIAN_POINT ( 'NONE',  ( 124.0848681442452772, -5.574606645277164318, -18.38911715685844683 ) ) ;
#5762 = CARTESIAN_POINT ( 'NONE',  ( 116.1777233795247781, -8.938348069036489818, -17.46756447353520159 ) ) ;
#5763 = CARTESIAN_POINT ( 'NONE',  ( 111.4549108795247747, -1.325403438956436419, -16.93181055722141792 ) ) ;
#5765 = CIRCLE ( 'NONE', #37804, 20.00000000000000355 ) ;
#5764 = CARTESIAN_POINT ( 'NONE',  ( 118.8092881442453290, -0.1624402480850797581, -16.17319339645315424 ) ) ;
#5766 = CARTESIAN_POINT ( 'NONE',  ( 82.47484345711939113, -31.70193537549793916, -22.53651891743845681 ) ) ;
#5767 = CARTESIAN_POINT ( 'NONE',  ( 68.97151291332768608, -25.95882592635068420, -5.893215200338315363 ) ) ;
#5768 = CARTESIAN_POINT ( 'NONE',  ( 111.7751814775786556, -2.084020599724406786, -8.691656652584148546 ) ) ;
#5769 = CARTESIAN_POINT ( 'NONE',  ( 125.2761281442453054, -10.63000616557722466, -14.87417383870573495 ) ) ;
#5770 = VERTEX_POINT ( 'NONE', #42150 ) ;
#5771 = EDGE_CURVE ( 'NONE', #9951, #34537, #42595, .T. ) ;
#5772 = CARTESIAN_POINT ( 'NONE',  ( 120.6812681442452941, 0.1319031606808879209, -14.10382304977623669 ) ) ;
#5773 = CARTESIAN_POINT ( 'NONE',  ( 113.5337081442453240, -9.261995988541697145, -16.69588392320189030 ) ) ;
#5774 = CARTESIAN_POINT ( 'NONE',  ( 125.1626748109119802, -9.988377603198980381, -10.36322818467138518 ) ) ;
#5775 = CARTESIAN_POINT ( 'NONE',  ( 123.4041481442452834, 0.1319031606808879209, -14.10382304977623669 ) ) ;
#5776 = ORIENTED_EDGE ( 'NONE', *, *, #31902, .T. ) ;
#5777 = CARTESIAN_POINT ( 'NONE',  ( 61.69084222814998242, 7.836001204160461420, -14.64321520033831447 ) ) ;
#5778 =( BOUNDED_SURFACE ( )  B_SPLINE_SURFACE ( 1, 2, ( 
 ( #20486, #34365, #12970, #29660, #26866, #40781, #23454, #3147, #29212, #43122, #11891, #25793, #39702, #8467, #8686, #5034, #36266, #26020, #32838, #15527, #29433, #12117, #39926, #38022, #17946, #41902, #21591, #7676, #163, #38236, #35016, #28438, #3369, #38455, #14525, #35247, #24349, #42351, #25012, #10221, #34585, #24570, #24130, #20707, #11110, #45099, #27771, #7226, #14302, #13856, #38905, #31179, #35478, #31394, #7016, #17068, #14079, #6798, #21140, #389, #44884, #38678, #10667, #3796, #17722, #30960, #13641, #41684, #20926, #17288, #31620, #28220, #42127, #31845, #27550, #7444, #10445, #17495, #10887, #34800, #3584, #27997, #24786, #21364, #4024, #614, #41462, #4926, #18840, #39818, #29554, #43015, #25913, #39598, #1506, #25691, #35707, #32732, #32513, #15426, #18623, #22708, #12011, #32951, #4252, #1728, #1061, #18169, #29331, #8359, #40038, #42570, #8804, #32066, #11333, #834, #1288, #15650, #36157, #22263, #8585, #19067, #15200, #22485, #4703, #43471, #22041, #8140, #14976, #36379, #43245, #5150, #12237, #26134, #14753, #28666, #25244, #39142, #11562, #7907, #39373, #11784, #21814, #4483, #29104, #18404, #32296, #28889, #42801, #25469, #35935, #41187, #9947, #27043, #40501, #40960, #13139, #9037, #26588, #9262, #44377, #12689, #26815, #44154, #36827, #1953, #6049, #26363, #12462, #22934, #5596, #19520, #23172, #16562, #30004, #29776, #23628, #40726, #5822, #37051, #34093, #19742, #40270, #12919, #19972, #19298, #9715, #30232, #9483, #23396, #13368, #36606, #33397, #43920, #43687, #16330, #37282, #33860, #37514, #44605, #6287, #2171, #33626, #2629, #16101, #2402, #30457, #20208, #2859, #16790, #30686, #27273, #5381, #33176, #15879, #3973, #17448, #337, #14030, #21085, #117, #10171, #7175, #6965, #24517, #38188, #42295, #31568, #7396, #23861, #21314, #20656, #37747, #3750, #27944, #14474, #17016, #28382, #6517, #30907, #20432, #20872, #35197, #10614, #41854, #14250, #38619, #34750, #28166, #24301, #17895, #41636, #27721, #34533, #42076, #38402, #34962 ),
 ( #31792, #564, #17672, #3532, #10392, #31343, #10834, #24731, #34316, #17234, #3089, #44829, #13587, #27497, #41417, #3311, #24078, #37971, #31125, #6747, #45050, #13810, #1452, #21987, #32013, #11956, #35876, #15595, #1672, #39317, #32239, #29054, #22432, #42522, #32461, #8530, #29276, #18346, #36325, #19010, #4201, #29498, #15372, #14926, #43192, #32682, #28613, #1010, #28837, #18793, #42747, #1236, #18569, #11283, #21538, #25642, #776, #14699, #25191, #39089, #7858, #11512, #36104, #4430, #18119, #25854, #15148, #5095, #21764, #32896, #25416, #8085, #11057, #4647, #35657, #42962, #39545, #38856, #39760, #11728, #8306, #22208, #24960, #7624, #4875, #35425, #5325, #23117, #33573, #26765, #44329, #6235, #19921, #19241, #43868, #2349, #1893, #36551, #33344, #2117, #40446, #9208, #33124, #16280, #44100, #12865, #33807, #23580, #36994, #2578, #30182, #40674, #19686, #29720, #9426, #26536, #23340, #12640, #16736, #5998, #26987, #43412, #40906, #40216, #12179, #37224, #16508, #34040, #15821, #2809, #26080, #43633, #39984, #5764, #9660, #30407, #13088, #37462, #20157, #8750, #22655, #12408, #26308, #16047, #29953, #8981, #22879, #36773, #5544, #19461, #3486, #34699, #3922, #10562, #31514, #37917, #21262, #20605, #38139, #286, #20820, #41584, #31291, #14197, #44548, #24247, #13312, #17402, #35142, #27670, #65, #6910, #10342, #28114, #16962, #30633, #3702, #41805, #27219, #17184, #3040, #13977, #31074, #34911, #42018, #3259, #45001, #27890, #41137, #24459, #38351, #7127, #21038, #24027, #10783, #17621, #24679, #10124, #34480, #9896, #38567, #7344, #20379, #23808, #30856, #37696, #6469, #44779, #34266, #13538, #27446, #41368, #6694, #13761, #15314, #22379, #29004, #28560, #24905, #36275, #35822, #25137, #28329, #4146, #25802, #11230, #17841, #31739, #35369, #42690, #42912, #11675, #25363, #39712, #39486, #11458, #42466, #22157, #1181, #4595, #39032, #4818, #28783, #8250, #955, #25584, #1398, #32632, #15094, #14872, #35597, #4370, #39258, #18289, #36050, #7803, #18741 ) ),
 .UNSPECIFIED., .F., .F., .F. ) 
 B_SPLINE_SURFACE_WITH_KNOTS ( ( 2, 2 ),
 ( 3, 2, 2, 2, 2, 2, 2, 2, 2, 2, 2, 2, 2, 2, 2, 2, 2, 2, 2, 2, 2, 2, 2, 2, 2, 2, 2, 2, 2, 2, 2, 2, 2, 2, 2, 2, 2, 2, 2, 2, 2, 2, 2, 2, 2, 2, 2, 2, 2, 2, 2, 2, 2, 2, 2, 2, 2, 2, 2, 2, 2, 2, 2, 2, 2, 2, 2, 2, 2, 2, 2, 2, 2, 2, 2, 2, 2, 2, 2, 2, 2, 2, 2, 2, 2, 2, 2, 2, 2, 2, 2, 2, 2, 2, 2, 2, 2, 2, 2, 2, 2, 2, 2, 2, 2, 2, 2, 2, 2, 2, 2, 2, 2, 2, 2, 2, 2, 2, 2, 2, 2, 2, 2, 2, 2, 2, 2, 2, 3 ),
 ( 0.000000000000000000, 1.000000000000000000 ),
 ( 0.000000000000000000, 0.007812500000000000000, 0.01562500000000000000, 0.02343750000000000000, 0.03125000000000000000, 0.03906250000000000000, 0.04687500000000000000, 0.05468750000000000000, 0.06250000000000000000, 0.07031250000000000000, 0.07812500000000000000, 0.08593750000000000000, 0.09375000000000000000, 0.1015625000000000000, 0.1093750000000000000, 0.1171875000000000000, 0.1250000000000000000, 0.1328125000000000000, 0.1406250000000000000, 0.1484375000000000000, 0.1562500000000000000, 0.1640625000000000000, 0.1718750000000000000, 0.1796875000000000000, 0.1875000000000000000, 0.1953125000000000000, 0.2031250000000000000, 0.2109375000000000000, 0.2187500000000000000, 0.2265625000000000000, 0.2343750000000000000, 0.2421875000000000000, 0.2500000000000000000, 0.2578125000000000000, 0.2656250000000000000, 0.2734375000000000000, 0.2812500000000000000, 0.2890625000000000000, 0.2968750000000000000, 0.3046875000000000000, 0.3125000000000000000, 0.3203125000000000000, 0.3281250000000000000, 0.3359375000000000000, 0.3437500000000000000, 0.3515625000000000000, 0.3593750000000000000, 0.3671875000000000000, 0.3750000000000000000, 0.3828125000000000000, 0.3906250000000000000, 0.3984375000000000000, 0.4062500000000000000, 0.4140625000000000000, 0.4218750000000000000, 0.4296875000000000000, 0.4375000000000000000, 0.4453125000000000000, 0.4531250000000000000, 0.4609375000000000000, 0.4687500000000000000, 0.4765625000000000000, 0.4843750000000000000, 0.4921875000000000000, 0.5000000000000000000, 0.5078125000000000000, 0.5156250000000000000, 0.5234375000000000000, 0.5312500000000000000, 0.5390625000000000000, 0.5468750000000000000, 0.5546875000000000000, 0.5625000000000000000, 0.5703125000000000000, 0.5781250000000000000, 0.5859375000000000000, 0.5937500000000000000, 0.6015625000000000000, 0.6093750000000000000, 0.6171875000000000000, 0.6250000000000000000, 0.6328125000000000000, 0.6406250000000000000, 0.6484375000000000000, 0.6562500000000000000, 0.6640625000000000000, 0.6718750000000000000, 0.6796875000000000000, 0.6875000000000000000, 0.6953125000000000000, 0.7031250000000000000, 0.7109375000000000000, 0.7187500000000000000, 0.7265625000000000000, 0.7343750000000000000, 0.7421875000000000000, 0.7500000000000000000, 0.7578125000000000000, 0.7656250000000000000, 0.7734375000000000000, 0.7812500000000000000, 0.7890625000000000000, 0.7968750000000000000, 0.8046875000000000000, 0.8125000000000000000, 0.8203125000000000000, 0.8281250000000000000, 0.8359375000000000000, 0.8437500000000000000, 0.8515625000000000000, 0.8593750000000000000, 0.8671875000000000000, 0.8750000000000000000, 0.8828125000000000000, 0.8906250000000000000, 0.8984375000000000000, 0.9062500000000000000, 0.9140625000000000000, 0.9218750000000000000, 0.9296875000000000000, 0.9375000000000000000, 0.9453125000000000000, 0.9531250000000000000, 0.9609375000000000000, 0.9687500000000000000, 0.9765625000000000000, 0.9843750000000000000, 0.9921875000000000000, 1.000000000000000000 ),
 .UNSPECIFIED. ) 
 GEOMETRIC_REPRESENTATION_ITEM ( )  RATIONAL_B_SPLINE_SURFACE ( (
 ( 1.000000000000000000, 0.9238795325112869605, 1.000000000000000000, 0.9238795325112869605, 1.000000000000000000, 0.9238795325112869605, 1.000000000000000000, 0.9238795325112869605, 1.000000000000000000, 0.9238795325112869605, 1.000000000000000000, 0.9238795325112869605, 1.000000000000000000, 0.9238795325112869605, 1.000000000000000000, 0.9238795325112869605, 1.000000000000000000, 0.9238795325112869605, 1.000000000000000000, 0.9238795325112869605, 1.000000000000000000, 0.9238795325112869605, 1.000000000000000000, 0.9238795325112869605, 1.000000000000000000, 0.9238795325112869605, 1.000000000000000000, 0.9238795325112869605, 1.000000000000000000, 0.9238795325112869605, 1.000000000000000000, 0.9238795325112869605, 1.000000000000000000, 0.9238795325112869605, 1.000000000000000000, 0.9238795325112869605, 1.000000000000000000, 0.9238795325112869605, 1.000000000000000000, 0.9238795325112869605, 1.000000000000000000, 0.9238795325112869605, 1.000000000000000000, 0.9238795325112869605, 1.000000000000000000, 0.9238795325112869605, 1.000000000000000000, 0.9238795325112869605, 1.000000000000000000, 0.9238795325112869605, 1.000000000000000000, 0.9238795325112869605, 1.000000000000000000, 0.9238795325112869605, 1.000000000000000000, 0.9238795325112869605, 1.000000000000000000, 0.9238795325112869605, 1.000000000000000000, 0.9238795325112869605, 1.000000000000000000, 0.9238795325112869605, 1.000000000000000000, 0.9238795325112869605, 1.000000000000000000, 0.9238795325112869605, 1.000000000000000000, 0.9238795325112869605, 1.000000000000000000, 0.9238795325112869605, 1.000000000000000000, 0.9238795325112869605, 1.000000000000000000, 0.9238795325112869605, 1.000000000000000000, 0.9238795325112869605, 1.000000000000000000, 0.9238795325112869605, 1.000000000000000000, 0.9238795325112869605, 1.000000000000000000, 0.9238795325112869605, 1.000000000000000000, 0.9238795325112869605, 1.000000000000000000, 0.9238795325112869605, 1.000000000000000000, 0.9238795325112869605, 1.000000000000000000, 0.9238795325112869605, 1.000000000000000000, 0.9238795325112869605, 1.000000000000000000, 0.9238795325112869605, 1.000000000000000000, 0.9238795325112869605, 1.000000000000000000, 0.9238795325112869605, 1.000000000000000000, 0.9238795325112869605, 1.000000000000000000, 0.9238795325112869605, 1.000000000000000000, 0.9238795325112869605, 1.000000000000000000, 0.9238795325112869605, 1.000000000000000000, 0.9238795325112869605, 1.000000000000000000, 0.9238795325112869605, 1.000000000000000000, 0.9238795325112869605, 1.000000000000000000, 0.9238795325112869605, 1.000000000000000000, 0.9238795325112869605, 1.000000000000000000, 0.9238795325112869605, 1.000000000000000000, 0.9238795325112869605, 1.000000000000000000, 0.9238795325112869605, 1.000000000000000000, 0.9238795325112869605, 1.000000000000000000, 0.9238795325112869605, 1.000000000000000000, 0.9238795325112869605, 1.000000000000000000, 0.9238795325112869605, 1.000000000000000000, 0.9238795325112869605, 1.000000000000000000, 0.9238795325112869605, 1.000000000000000000, 0.9238795325112869605, 1.000000000000000000, 0.9238795325112869605, 1.000000000000000000, 0.9238795325112869605, 1.000000000000000000, 0.9238795325112869605, 1.000000000000000000, 0.9238795325112869605, 1.000000000000000000, 0.9238795325112869605, 1.000000000000000000, 0.9238795325112869605, 1.000000000000000000, 0.9238795325112869605, 1.000000000000000000, 0.9238795325112869605, 1.000000000000000000, 0.9238795325112869605, 1.000000000000000000, 0.9238795325112869605, 1.000000000000000000, 0.9238795325112869605, 1.000000000000000000, 0.9238795325112869605, 1.000000000000000000, 0.9238795325112869605, 1.000000000000000000, 0.9238795325112869605, 1.000000000000000000, 0.9238795325112869605, 1.000000000000000000, 0.9238795325112869605, 1.000000000000000000, 0.9238795325112869605, 1.000000000000000000, 0.9238795325112869605, 1.000000000000000000, 0.9238795325112869605, 1.000000000000000000, 0.9238795325112869605, 1.000000000000000000, 0.9238795325112869605, 1.000000000000000000, 0.9238795325112869605, 1.000000000000000000, 0.9238795325112869605, 1.000000000000000000, 0.9238795325112869605, 1.000000000000000000, 0.9238795325112869605, 1.000000000000000000, 0.9238795325112869605, 1.000000000000000000, 0.9238795325112869605, 1.000000000000000000, 0.9238795325112869605, 1.000000000000000000, 0.9238795325112869605, 1.000000000000000000, 0.9238795325112869605, 1.000000000000000000, 0.9238795325112869605, 1.000000000000000000, 0.9238795325112869605, 1.000000000000000000, 0.9238795325112869605, 1.000000000000000000, 0.9238795325112869605, 1.000000000000000000, 0.9238795325112869605, 1.000000000000000000, 0.9238795325112869605, 1.000000000000000000, 0.9238795325112869605, 1.000000000000000000, 0.9238795325112869605, 1.000000000000000000, 0.9238795325112869605, 1.000000000000000000, 0.9238795325112869605, 1.000000000000000000, 0.9238795325112869605, 1.000000000000000000, 0.9238795325112869605, 1.000000000000000000, 0.9238795325112869605, 1.000000000000000000, 0.9238795325112869605, 1.000000000000000000, 0.9238795325112869605, 1.000000000000000000, 0.9238795325112869605, 1.000000000000000000, 0.9238795325112869605, 1.000000000000000000, 0.9238795325112869605, 1.000000000000000000, 0.9238795325112869605, 1.000000000000000000, 0.9238795325112869605, 1.000000000000000000, 0.9238795325112869605, 1.000000000000000000, 0.9238795325112869605, 1.000000000000000000, 0.9238795325112869605, 1.000000000000000000, 0.9238795325112869605, 1.000000000000000000, 0.9238795325112869605, 1.000000000000000000, 0.9238795325112869605, 1.000000000000000000, 0.9238795325112869605, 1.000000000000000000, 0.9238795325112869605, 1.000000000000000000, 0.9238795325112869605, 1.000000000000000000, 0.9238795325112869605, 1.000000000000000000),
 ( 1.000000000000000000, 0.9238795325112869605, 1.000000000000000000, 0.9238795325112869605, 1.000000000000000000, 0.9238795325112869605, 1.000000000000000000, 0.9238795325112869605, 1.000000000000000000, 0.9238795325112869605, 1.000000000000000000, 0.9238795325112869605, 1.000000000000000000, 0.9238795325112869605, 1.000000000000000000, 0.9238795325112869605, 1.000000000000000000, 0.9238795325112869605, 1.000000000000000000, 0.9238795325112869605, 1.000000000000000000, 0.9238795325112869605, 1.000000000000000000, 0.9238795325112869605, 1.000000000000000000, 0.9238795325112869605, 1.000000000000000000, 0.9238795325112869605, 1.000000000000000000, 0.9238795325112869605, 1.000000000000000000, 0.9238795325112869605, 1.000000000000000000, 0.9238795325112869605, 1.000000000000000000, 0.9238795325112869605, 1.000000000000000000, 0.9238795325112869605, 1.000000000000000000, 0.9238795325112869605, 1.000000000000000000, 0.9238795325112869605, 1.000000000000000000, 0.9238795325112869605, 1.000000000000000000, 0.9238795325112869605, 1.000000000000000000, 0.9238795325112869605, 1.000000000000000000, 0.9238795325112869605, 1.000000000000000000, 0.9238795325112869605, 1.000000000000000000, 0.9238795325112869605, 1.000000000000000000, 0.9238795325112869605, 1.000000000000000000, 0.9238795325112869605, 1.000000000000000000, 0.9238795325112869605, 1.000000000000000000, 0.9238795325112869605, 1.000000000000000000, 0.9238795325112869605, 1.000000000000000000, 0.9238795325112869605, 1.000000000000000000, 0.9238795325112869605, 1.000000000000000000, 0.9238795325112869605, 1.000000000000000000, 0.9238795325112869605, 1.000000000000000000, 0.9238795325112869605, 1.000000000000000000, 0.9238795325112869605, 1.000000000000000000, 0.9238795325112869605, 1.000000000000000000, 0.9238795325112869605, 1.000000000000000000, 0.9238795325112869605, 1.000000000000000000, 0.9238795325112869605, 1.000000000000000000, 0.9238795325112869605, 1.000000000000000000, 0.9238795325112869605, 1.000000000000000000, 0.9238795325112869605, 1.000000000000000000, 0.9238795325112869605, 1.000000000000000000, 0.9238795325112869605, 1.000000000000000000, 0.9238795325112869605, 1.000000000000000000, 0.9238795325112869605, 1.000000000000000000, 0.9238795325112869605, 1.000000000000000000, 0.9238795325112869605, 1.000000000000000000, 0.9238795325112869605, 1.000000000000000000, 0.9238795325112869605, 1.000000000000000000, 0.9238795325112869605, 1.000000000000000000, 0.9238795325112869605, 1.000000000000000000, 0.9238795325112869605, 1.000000000000000000, 0.9238795325112869605, 1.000000000000000000, 0.9238795325112869605, 1.000000000000000000, 0.9238795325112869605, 1.000000000000000000, 0.9238795325112869605, 1.000000000000000000, 0.9238795325112869605, 1.000000000000000000, 0.9238795325112869605, 1.000000000000000000, 0.9238795325112869605, 1.000000000000000000, 0.9238795325112869605, 1.000000000000000000, 0.9238795325112869605, 1.000000000000000000, 0.9238795325112869605, 1.000000000000000000, 0.9238795325112869605, 1.000000000000000000, 0.9238795325112869605, 1.000000000000000000, 0.9238795325112869605, 1.000000000000000000, 0.9238795325112869605, 1.000000000000000000, 0.9238795325112869605, 1.000000000000000000, 0.9238795325112869605, 1.000000000000000000, 0.9238795325112869605, 1.000000000000000000, 0.9238795325112869605, 1.000000000000000000, 0.9238795325112869605, 1.000000000000000000, 0.9238795325112869605, 1.000000000000000000, 0.9238795325112869605, 1.000000000000000000, 0.9238795325112869605, 1.000000000000000000, 0.9238795325112869605, 1.000000000000000000, 0.9238795325112869605, 1.000000000000000000, 0.9238795325112869605, 1.000000000000000000, 0.9238795325112869605, 1.000000000000000000, 0.9238795325112869605, 1.000000000000000000, 0.9238795325112869605, 1.000000000000000000, 0.9238795325112869605, 1.000000000000000000, 0.9238795325112869605, 1.000000000000000000, 0.9238795325112869605, 1.000000000000000000, 0.9238795325112869605, 1.000000000000000000, 0.9238795325112869605, 1.000000000000000000, 0.9238795325112869605, 1.000000000000000000, 0.9238795325112869605, 1.000000000000000000, 0.9238795325112869605, 1.000000000000000000, 0.9238795325112869605, 1.000000000000000000, 0.9238795325112869605, 1.000000000000000000, 0.9238795325112869605, 1.000000000000000000, 0.9238795325112869605, 1.000000000000000000, 0.9238795325112869605, 1.000000000000000000, 0.9238795325112869605, 1.000000000000000000, 0.9238795325112869605, 1.000000000000000000, 0.9238795325112869605, 1.000000000000000000, 0.9238795325112869605, 1.000000000000000000, 0.9238795325112869605, 1.000000000000000000, 0.9238795325112869605, 1.000000000000000000, 0.9238795325112869605, 1.000000000000000000, 0.9238795325112869605, 1.000000000000000000, 0.9238795325112869605, 1.000000000000000000, 0.9238795325112869605, 1.000000000000000000, 0.9238795325112869605, 1.000000000000000000, 0.9238795325112869605, 1.000000000000000000, 0.9238795325112869605, 1.000000000000000000, 0.9238795325112869605, 1.000000000000000000, 0.9238795325112869605, 1.000000000000000000, 0.9238795325112869605, 1.000000000000000000, 0.9238795325112869605, 1.000000000000000000, 0.9238795325112869605, 1.000000000000000000, 0.9238795325112869605, 1.000000000000000000, 0.9238795325112869605, 1.000000000000000000, 0.9238795325112869605, 1.000000000000000000, 0.9238795325112869605, 1.000000000000000000, 0.9238795325112869605, 1.000000000000000000, 0.9238795325112869605, 1.000000000000000000, 0.9238795325112869605, 1.000000000000000000, 0.9238795325112869605, 1.000000000000000000, 0.9238795325112869605, 1.000000000000000000, 0.9238795325112869605, 1.000000000000000000, 0.9238795325112869605, 1.000000000000000000, 0.9238795325112869605, 1.000000000000000000, 0.9238795325112869605, 1.000000000000000000) ) ) 
 REPRESENTATION_ITEM ( '' )  SURFACE ( )  );
#5779 = CARTESIAN_POINT ( 'NONE',  ( 123.6310548109119765, -5.638512984488999180, -18.83840828888717311 ) ) ;
#5780 = CARTESIAN_POINT ( 'NONE',  ( 114.1009748109119784, -5.574606645277164318, -18.38911715685844683 ) ) ;
#5781 = CARTESIAN_POINT ( 'NONE',  ( 125.7866681442452688, -0.4660016031367893996, -10.09054647747474043 ) ) ;
#5782 = ADVANCED_FACE ( 'NONE', ( #41926 ), #4839, .T. ) ;
#5783 = CARTESIAN_POINT ( 'NONE',  ( 107.0099108795247815, -8.938348069036489818, -9.318865927141430916 ) ) ;
#5784 = EDGE_CURVE ( 'NONE', #11292, #6949, #1942, .T. ) ;
#5785 = EDGE_CURVE ( 'NONE', #26941, #12518, #36144, .T. ) ;
#5786 = CARTESIAN_POINT ( 'NONE',  ( 66.58723489636778936, -20.14619392353143112, -19.39321520033831447 ) ) ;
#5787 = ORIENTED_EDGE ( 'NONE', *, *, #23104, .T. ) ;
#5788 = DIRECTION ( 'NONE',  ( 1.000000000000000000, 0.000000000000000000, 0.000000000000000000 ) ) ;
#5789 = CARTESIAN_POINT ( 'NONE',  ( 109.9269421295247753, -9.868328341294093420, -13.39321520033831447 ) ) ;
#5790 = AXIS2_PLACEMENT_3D ( 'NONE', #42439, #10315, #38108 ) ;
#5791 = CYLINDRICAL_SURFACE ( 'NONE', #40144, 0.8718221387495478369 ) ;
#5792 = CARTESIAN_POINT ( 'NONE',  ( 120.2841814775786276, -10.15424416112533912, -14.75197769757731336 ) ) ;
#5793 = CARTESIAN_POINT ( 'NONE',  ( 115.5191414775786569, -6.222761293078241884, -8.102969835052219238 ) ) ;
#5794 = CARTESIAN_POINT ( 'NONE',  ( 126.2687745536026398, -5.836013449744841708, -18.32348129158890870 ) ) ;
#5795 = ORIENTED_EDGE ( 'NONE', *, *, #4690, .F. ) ;
#5796 = DIRECTION ( 'NONE',  ( 0.000000000000000000, 0.000000000000000000, 1.000000000000000000 ) ) ;
#5797 = CARTESIAN_POINT ( 'NONE',  ( 116.4834948109119779, -7.894159318335828068, -9.358103419637847864 ) ) ;
#5798 = DIRECTION ( 'NONE',  ( 0.9609149988134837450, -0.1028163501681639419, 0.2570431154366518145 ) ) ;
#5799 = AXIS2_PLACEMENT_3D ( 'NONE', #2855, #20428, #16786 ) ;
#5800 = CARTESIAN_POINT ( 'NONE',  ( 67.42381492657879960, -0.1846631707194854588, -10.39321520033831625 ) ) ;
#5801 = CARTESIAN_POINT ( 'NONE',  ( 122.8176765460471813, -2.191907684172563986, -18.20049396185734025 ) ) ;
#5803 = CARTESIAN_POINT ( 'NONE',  ( 122.1561614775786353, -0.4660016031367893996, -10.09054647747474043 ) ) ;
#5802 = DIRECTION ( 'NONE',  ( 0.8636456077245088236, -0.5040994586965589219, 0.000000000000000000 ) ) ;
#5804 = CARTESIAN_POINT ( 'NONE',  ( 124.2550481442452792, -0.1624402480850797581, -16.17319339645315424 ) ) ;
#5805 = VERTEX_POINT ( 'NONE', #24811 ) ;
#5806 = VECTOR ( 'NONE', #23882, 1000.000000000000000 ) ;
#5807 = CARTESIAN_POINT ( 'NONE',  ( 73.07463722459043254, -51.06865355621575731, -32.73578466827673594 ) ) ;
#5808 = CARTESIAN_POINT ( 'NONE',  ( 126.4915402333596575, 0.09659745337240860374, -14.72609753513648201 ) ) ;
#5809 = CARTESIAN_POINT ( 'NONE',  ( 111.2465515045248168, -6.936859964151250502, -18.39754474579286025 ) ) ;
#5810 = CARTESIAN_POINT ( 'NONE',  ( 124.8790414775786246, -8.899110576539710493, -16.42337572283490132 ) ) ;
#5811 = CARTESIAN_POINT ( 'NONE',  ( 119.4900081442453086, -7.643976991954077427, -18.09477374809248928 ) ) ;
#5812 = CARTESIAN_POINT ( 'NONE',  ( 124.9542645564618653, 2.335564274171338273, -15.89604958949715829 ) ) ;
#5813 = CARTESIAN_POINT ( 'NONE',  ( 112.6356140045247827, 0.1403307496149616695, -15.46607636864997204 ) ) ;
#5814 = ADVANCED_FACE ( 'NONE', ( #38929 ), #185, .T. ) ;
#5815 = CARTESIAN_POINT ( 'NONE',  ( 116.8238548109119819, -4.089484607189483256, -7.948022111789462052 ) ) ;
#5816 = CARTESIAN_POINT ( 'NONE',  ( 90.33554924625337890, -24.14644159042263993, -12.62951656296512937 ) ) ;
#5817 = CARTESIAN_POINT ( 'NONE',  ( 114.5547881442453217, -4.153390946401321671, -8.397313243818183892 ) ) ;
#5818 = CARTESIAN_POINT ( 'NONE',  ( 109.5102233795247884, -8.938348069036489818, -17.46756447353520159 ) ) ;
#5819 = CARTESIAN_POINT ( 'NONE',  ( -13.88591660730176436, -4.361019060476756692, -18.21192235134802928 ) ) ;
#5820 = CARTESIAN_POINT ( 'NONE',  ( 115.4831921295247952, 0.8980012041604618078, -13.39321520033831447 ) ) ;
#5821 = CARTESIAN_POINT ( 'NONE',  ( 120.1707281442453166, 0.2603800115204892296, -16.42320221600525088 ) ) ;
#5822 = CARTESIAN_POINT ( 'NONE',  ( 121.8158014775786171, -5.638512984488999180, -18.83840828888717311 ) ) ;
#5823 = CARTESIAN_POINT ( 'NONE',  ( 119.7736414775786358, 0.1319031606808853119, -14.10382304977625800 ) ) ;
#5824 = CARTESIAN_POINT ( 'NONE',  ( 116.6536748109119941, 0.9020085738987339008, -11.91225656197089222 ) ) ;
#5825 = CARTESIAN_POINT ( 'NONE',  ( 113.0798948109119948, -0.4660016031367893996, -10.09054647747474043 ) ) ;
#5826 = ORIENTED_EDGE ( 'NONE', *, *, #25693, .T. ) ;
#5827 = CARTESIAN_POINT ( 'NONE',  ( 114.8951481442453115, -8.899110576539710493, -16.42337572283490132 ) ) ;
#5828 = EDGE_CURVE ( 'NONE', #30808, #29459, #22551, .T. ) ;
#5829 = CARTESIAN_POINT ( 'NONE',  ( 125.9568481442452850, -6.344957434206665248, -7.627207830600338134 ) ) ;
#5830 = CARTESIAN_POINT ( 'NONE',  ( 119.7169148109119874, -9.988377603198976828, -10.36322818467138340 ) ) ;
#5831 = AXIS2_PLACEMENT_3D ( 'NONE', #15067, #36249, #39910 ) ;
#5832 = CARTESIAN_POINT ( 'NONE',  ( 125.2194014775786286, 0.1319031606808879209, -14.10382304977623669 ) ) ;
#5833 = CARTESIAN_POINT ( 'NONE',  ( 111.5482748109120053, -0.1624402480850797581, -16.17319339645315424 ) ) ;
#5834 = ORIENTED_EDGE ( 'NONE', *, *, #7475, .T. ) ;
#5835 = CARTESIAN_POINT ( 'NONE',  ( 118.1285681442453068, -2.084020599724406786, -8.691656652584148546 ) ) ;
#5836 = CARTESIAN_POINT ( 'NONE',  ( 125.0492214775786266, -6.344957434206665248, -7.627207830600338134 ) ) ;
#5837 = CARTESIAN_POINT ( 'NONE',  ( 108.4684265045247997, -7.250697342233347165, -19.15521520033831138 ) ) ;
#5838 = CARTESIAN_POINT ( 'NONE',  ( 120.8514481442452961, -2.084020599724406786, -8.691656652584148546 ) ) ;
#5839 = CARTESIAN_POINT ( 'NONE',  ( 110.0658483795247804, -0.7896495226426338832, -9.318865927141436245 ) ) ;
#5840 = CARTESIAN_POINT ( 'NONE',  ( 70.19189222814998175, -61.90193818873174791, -37.96356864969668266 ) ) ;
#5841 = ORIENTED_EDGE ( 'NONE', *, *, #24435, .T. ) ;
#5842 = VECTOR ( 'NONE', #42208, 1000.000000000000000 ) ;
#5843 = EDGE_CURVE ( 'NONE', #9192, #28442, #20904, .T. ) ;
#5844 = CARTESIAN_POINT ( 'NONE',  ( 121.6186891859119896, -1.406689858478933353, -17.56299727309130887 ) ) ;
#5845 = CARTESIAN_POINT ( 'NONE',  ( 123.1205148109119563, -1.834011780172310813, -8.268836392978581529 ) ) ;
#5846 = CARTESIAN_POINT ( 'NONE',  ( 112.7491510812576934, -0.01829820670803256055, -12.14321520033831625 ) ) ;
#5847 = CARTESIAN_POINT ( 'NONE',  ( 67.84197459855160162, -53.65469605205331050, -35.39387355951068059 ) ) ;
#5848 = CARTESIAN_POINT ( 'NONE',  ( 112.4559014775786494, -9.988377603198976828, -10.36322818467138340 ) ) ;
#5849 = ADVANCED_FACE ( 'NONE', ( #7700 ), #7928, .F. ) ;
#5850 = FACE_OUTER_BOUND ( 'NONE', #13015, .T. ) ;
#5851 = CARTESIAN_POINT ( 'NONE',  ( 109.2324108795247923, -1.325403438956436419, -16.93181055722141792 ) ) ;
#5852 = DIRECTION ( 'NONE',  ( 0.000000000000000000, -0.9242245927363029745, -0.3818493186865927758 ) ) ;
#5853 = CIRCLE ( 'NONE', #35701, 2.000000000000000444 ) ;
#5854 = CARTESIAN_POINT ( 'NONE',  ( 125.0929224177872783, -2.472073928853079305, -17.82741071888329643 ) ) ;
#5855 = CARTESIAN_POINT ( 'NONE',  ( 123.6360048109119703, -7.198765429287139916, -17.81462501705270540 ) ) ;
#5856 =( BOUNDED_CURVE ( )  B_SPLINE_CURVE ( 2, ( #42876, #467, #34876, #687, #21001, #41982, #11634, #14836, #35558, #10747, #17583, #3664, #42205, #10967, #4102, #24869, #25097 ),
 .UNSPECIFIED., .F., .T. ) 
 B_SPLINE_CURVE_WITH_KNOTS ( ( 3, 2, 2, 2, 2, 2, 2, 2, 3 ),
 ( 0.5795046674808920217, 0.5859375000000000000, 0.5937500000000000000, 0.6015625000000000000, 0.6093750000000000000, 0.6171875000000000000, 0.6250000000000000000, 0.6328125000000000000, 0.6392453325190590174 ),
 .UNSPECIFIED. ) 
 CURVE ( )  GEOMETRIC_REPRESENTATION_ITEM ( )  RATIONAL_B_SPLINE_CURVE ( ( 0.9778625265006459788, 0.9373222120152210346, 1.000000000000000000, 0.9238795325112869605, 1.000000000000000000, 0.9238795325112869605, 1.000000000000000000, 0.9238795325112869605, 1.000000000000000000, 0.9238795325112869605, 1.000000000000000000, 0.9238795325112869605, 1.000000000000000000, 0.9238795325112869605, 1.000000000000000000, 0.9373222120157009840, 0.9778625265000250311 ) ) 
 REPRESENTATION_ITEM ( '' )  );
#5857 = CARTESIAN_POINT ( 'NONE',  ( 118.8660148109119774, 0.1319031606808879209, -14.10382304977623669 ) ) ;
#5858 = DIRECTION ( 'NONE',  ( -1.000000000000000000, 0.000000000000000000, 0.000000000000000000 ) ) ;
#5859 = ORIENTED_EDGE ( 'NONE', *, *, #35036, .T. ) ;
#5860 = CARTESIAN_POINT ( 'NONE',  ( 121.5321681442453183, -9.988377603198976828, -10.36322818467138340 ) ) ;
#5861 = CARTESIAN_POINT ( 'NONE',  ( 114.4413348109119823, -9.261995988541697145, -16.69588392320189030 ) ) ;
#5862 = CARTESIAN_POINT ( 'NONE',  ( 116.1777233795247781, -1.325403438956436419, -9.854619843455211026 ) ) ;
#5863 = CARTESIAN_POINT ( 'NONE',  ( 112.9664414775786412, -9.859900752359374465, -12.68260735090039404 ) ) ;
#5864 = CARTESIAN_POINT ( 'NONE',  ( 124.9924948109119924, -5.574606645277164318, -18.38911715685844683 ) ) ;
#5865 = CARTESIAN_POINT ( 'NONE',  ( 125.8433948109119456, -1.834011780172310813, -8.268836392978581529 ) ) ;
#5866 = CARTESIAN_POINT ( 'NONE',  ( 116.1082702545247827, -10.62599879583958717, -15.77991374673208469 ) ) ;
#5867 = CARTESIAN_POINT ( 'NONE',  ( 110.8992858795247827, -8.402594152722688392, -9.854619843455216355 ) ) ;
#5868 = CARTESIAN_POINT ( 'NONE',  ( 124.6989476299233530, -12.60226495975998517, -14.43526558578360053 ) ) ;
#5869 = CARTESIAN_POINT ( 'NONE',  ( 117.5613014775786525, -10.15424416112533912, -14.75197769757731336 ) ) ;
#5870 = AXIS2_PLACEMENT_3D ( 'NONE', #5151, #8141, #35936 ) ;
#5871 = CARTESIAN_POINT ( 'NONE',  ( 117.9583881442453048, 0.1319031606808879209, -14.10382304977623669 ) ) ;
#5872 = CARTESIAN_POINT ( 'NONE',  ( 113.2987212410415765, 0.7607806665037644134, -12.14321520033829493 ) ) ;
#5873 = CARTESIAN_POINT ( 'NONE',  ( 112.8439733795247832, -1.325403438956436419, -9.854619843455211026 ) ) ;
#5874 = VERTEX_POINT ( 'NONE', #17969 ) ;
#5875 = AXIS2_PLACEMENT_3D ( 'NONE', #16189, #26219, #12545 ) ;
#5876 = CARTESIAN_POINT ( 'NONE',  ( 123.0070614775786311, -10.15424416112535155, -14.75197769757726185 ) ) ;
#5877 = CARTESIAN_POINT ( 'NONE',  ( 126.6942948109119840, -8.899110576539710493, -16.42337572283490132 ) ) ;
#5878 = CARTESIAN_POINT ( 'NONE',  ( 119.4656423109119743, -0.4387604401700512802, -15.73000352943951619 ) ) ;
#5879 = CARTESIAN_POINT ( 'NONE',  ( 120.6463454359119822, 0.5291689781388270175, -13.89700978578772705 ) ) ;
#5880 = ORIENTED_EDGE ( 'NONE', *, *, #4755, .T. ) ;
#5881 = CARTESIAN_POINT ( 'NONE',  ( 138.2184548109119930, -1.191816558809784876, -8.648209655763537285 ) ) ;
#5882 = CARTESIAN_POINT ( 'NONE',  ( 116.5287898038745169, -11.91700341232977500, -21.13838130341561339 ) ) ;
#5883 = EDGE_LOOP ( 'NONE', ( #20444, #11131, #27403, #31731 ) ) ;
#5884 = CARTESIAN_POINT ( 'NONE',  ( 117.1642148109119859, -9.261995988541697145, -16.69588392320189030 ) ) ;
#5885 = CARTESIAN_POINT ( 'NONE',  ( 123.6877814775786533, -6.222761293078241884, -8.102969835052219238 ) ) ;
#5886 = CARTESIAN_POINT ( 'NONE',  ( 113.6471614775786492, -4.153390946401321671, -8.397313243818183892 ) ) ;
#5887 = DIRECTION ( 'NONE',  ( 0.000000000000000000, 0.3713878862591638574, -0.9284778069183724503 ) ) ;
#5888 = CARTESIAN_POINT ( 'NONE',  ( 122.8368814775786291, -1.561330072975668948, -17.79121239304076951 ) ) ;
#5889 = CARTESIAN_POINT ( 'NONE',  ( 114.4413348109119823, -9.261995988541697145, -16.69588392320189030 ) ) ;
#5890 = EDGE_CURVE ( 'NONE', #8490, #25201, #43460, .T. ) ;
#5891 = CARTESIAN_POINT ( 'NONE',  ( 110.4131140045248287, 0.1403307496149616695, -15.46607636864997204 ) ) ;
#5892 = AXIS2_PLACEMENT_3D ( 'NONE', #38720, #42616, #38952 ) ;
#5893 = CARTESIAN_POINT ( 'NONE',  ( 124.9924948109119924, -4.089484607189486809, -7.948022111789456723 ) ) ;
#5894 = PRESENTATION_STYLE_ASSIGNMENT (( #19137 ) ) ;
#5895 = VERTEX_POINT ( 'NONE', #39164 ) ;
#5896 = CARTESIAN_POINT ( 'NONE',  ( 113.5337081442453240, -9.261995988541697145, -16.69588392320189030 ) ) ;
#5897 = CARTESIAN_POINT ( 'NONE',  ( 113.6471614775786492, -4.153390946401321671, -8.397313243818183892 ) ) ;
#5898 = CARTESIAN_POINT ( 'NONE',  ( 73.07463722459043254, -57.56799820464436834, -35.33549987209089238 ) ) ;
#5899 = CARTESIAN_POINT ( 'NONE',  ( 125.9568481442452850, -3.505236298600246325, -18.68346056562440793 ) ) ;
#5900 = EDGE_LOOP ( 'NONE', ( #21914, #10512, #19218, #30353 ) ) ;
#5901 = AXIS2_PLACEMENT_3D ( 'NONE', #3429, #24187, #41525 ) ;
#5902 = CARTESIAN_POINT ( 'NONE',  ( 121.5321681442453183, -9.988377603198976828, -10.36322818467138340 ) ) ;
#5903 = DIRECTION ( 'NONE',  ( 0.000000000000000000, 0.000000000000000000, 1.000000000000000000 ) ) ;
#5904 = EDGE_CURVE ( 'NONE', #39007, #39913, #15654, .T. ) ;
#5905 = CARTESIAN_POINT ( 'NONE',  ( 120.0180923109119675, -9.285408612553503360, -11.05844856689016886 ) ) ;
#5906 = CIRCLE ( 'NONE', #13116, 6.000000000000000888 ) ;
#5907 = CARTESIAN_POINT ( 'NONE',  ( 77.67538405296900805, -57.05391890152773726, -1.450191271579374774 ) ) ;
#5908 = CARTESIAN_POINT ( 'NONE',  ( 117.7882081442453170, -3.505236298600246325, -18.68346056562440793 ) ) ;
#5909 = CARTESIAN_POINT ( 'NONE',  ( 123.4801383079017967, -4.061106116276376632, -15.71137846253180292 ) ) ;
#5910 = CARTESIAN_POINT ( 'NONE',  ( 115.1220548109119761, -1.833838273342658809, -17.42832698103878286 ) ) ;
#5911 = DIRECTION ( 'NONE',  ( -0.000000000000000000, -0.9284778069183721172, -0.3713878862591650232 ) ) ;
#5912 = DIRECTION ( 'NONE',  ( -0.000000000000000000, -0.9284778069183720062, -0.3713878862591650232 ) ) ;
#5913 = CARTESIAN_POINT ( 'NONE',  ( 114.7816948109119863, -9.859900752359374465, -12.68260735090039404 ) ) ;
#5914 = CARTESIAN_POINT ( 'NONE',  ( 117.1642148109119859, -9.261995988541697145, -16.69588392320189030 ) ) ;
#5915 = CARTESIAN_POINT ( 'NONE',  ( 124.3273610609119686, -6.340755971794695078, -8.611740276972781771 ) ) ;
#5916 = CARTESIAN_POINT ( 'NONE',  ( 126.1837548109119496, 0.4262465694468514643, -12.03445270309931736 ) ) ;
#5917 = CARTESIAN_POINT ( 'NONE',  ( 115.5191414775786569, -6.222761293078241884, -8.102969835052219238 ) ) ;
#5918 = CARTESIAN_POINT ( 'NONE',  ( 124.9357681442453014, -1.834011780172310813, -8.268836392978581529 ) ) ;
#5919 = CARTESIAN_POINT ( 'NONE',  ( 120.5678148109119832, -8.166667518702819706, -8.995218007635861213 ) ) ;
#5920 = VERTEX_POINT ( 'NONE', #42373 ) ;
#5921 = CARTESIAN_POINT ( 'NONE',  ( 113.3635281442453504, -9.988377603198976828, -10.36322818467138340 ) ) ;
#5922 = CARTESIAN_POINT ( 'NONE',  ( 113.2606921295247702, 0.8980012041604618078, -13.39321520033831447 ) ) ;
#5923 = FACE_OUTER_BOUND ( 'NONE', #16201, .T. ) ;
#5924 = LINE ( 'NONE', #19847, #28365 ) ;
#5925 = TOROIDAL_SURFACE ( 'NONE', #24873, 12.50000000000000000, 1.500000000000000000 ) ;
#5926 = CARTESIAN_POINT ( 'NONE',  ( 109.4407702545248355, -10.62599879583953388, -15.77991374673210601 ) ) ;
#5927 = CARTESIAN_POINT ( 'NONE',  ( 118.4689281442453392, 0.9020085738987339008, -11.91225656197089222 ) ) ;
#5928 = ORIENTED_EDGE ( 'NONE', *, *, #616, .T. ) ;
#5929 = CARTESIAN_POINT ( 'NONE',  ( 124.8790414775786246, -0.4660016031367893996, -10.09054647747474043 ) ) ;
#5930 = DIRECTION ( 'NONE',  ( -0.9387755102040817867, 0.3445294493088593701, 0.000000000000000000 ) ) ;
#5931 = CARTESIAN_POINT ( 'NONE',  ( 112.9664414775786412, -9.859900752359374465, -12.68260735090039404 ) ) ;
#5932 = CARTESIAN_POINT ( 'NONE',  ( 105.4819421295248247, -9.868328341294093420, -13.39321520033831447 ) ) ;
#5933 = CARTESIAN_POINT ( 'NONE',  ( 120.2841814775786276, 0.9020085738987339008, -11.91225656197089222 ) ) ;
#5934 = CARTESIAN_POINT ( 'NONE',  ( 114.7886608795247696, -1.325403438956436419, -16.93181055722141792 ) ) ;
#5935 = DIRECTION ( 'NONE',  ( 0.000000000000000000, 0.9284778069183721172, 0.3713878862591650232 ) ) ;
#5936 = ORIENTED_EDGE ( 'NONE', *, *, #21941, .T. ) ;
#5937 = DIRECTION ( 'NONE',  ( 0.8636456077245086016, -0.5040994586965593660, 0.000000000000000000 ) ) ;
#5938 = AXIS2_PLACEMENT_3D ( 'NONE', #6094, #3129, #34131 ) ;
#5939 = CARTESIAN_POINT ( 'NONE',  ( 123.5743281442453139, -2.084020599724406786, -8.691656652584148546 ) ) ;
#5940 = CARTESIAN_POINT ( 'NONE',  ( 119.7736414775786358, -10.30919188438810075, -12.61870101168855918 ) ) ;
#5941 = CARTESIAN_POINT ( 'NONE',  ( 114.6115148109119986, -6.222761293078241884, -8.102969835052219238 ) ) ;
#5942 = CARTESIAN_POINT ( 'NONE',  ( 114.1009748109119784, -4.089484607189486809, -7.948022111789456723 ) ) ;
#5943 = DIRECTION ( 'NONE',  ( 1.000000000000000000, 0.000000000000000000, 0.000000000000000000 ) ) ;
#5944 = FACE_OUTER_BOUND ( 'NONE', #36058, .T. ) ;
#5945 = CARTESIAN_POINT ( 'NONE',  ( 120.0572748109119772, -6.222761293078241884, -8.102969835052219238 ) ) ;
#5946 = ORIENTED_EDGE ( 'NONE', *, *, #24219, .T. ) ;
#5947 = CARTESIAN_POINT ( 'NONE',  ( 121.8965016859119856, -9.665098340737509730, -17.37397104707595474 ) ) ;
#5948 = CARTESIAN_POINT ( 'NONE',  ( 112.9097148109120070, 0.2603800115204892296, -16.42320221600525088 ) ) ;
#5949 = CARTESIAN_POINT ( 'NONE',  ( 120.6245414775786458, -0.1624402480850797581, -16.17319339645315424 ) ) ;
#5950 = VERTEX_POINT ( 'NONE', #14328 ) ;
#5951 = CARTESIAN_POINT ( 'NONE',  ( 124.3968141859119783, -8.321307733199551748, -9.223433127585318303 ) ) ;
#5952 = CARTESIAN_POINT ( 'NONE',  ( 117.7882081442453170, -6.344957434206665248, -7.627207830600338134 ) ) ;
#5953 = CARTESIAN_POINT ( 'NONE',  ( 110.9687390045248350, 0.8980012041604421569, -15.77991374673208469 ) ) ;
#5954 = CARTESIAN_POINT ( 'NONE',  ( 117.6747548109119919, -7.643976991954077427, -18.09477374809248928 ) ) ;
#5955 = VERTEX_POINT ( 'NONE', #11134 ) ;
#5956 = EDGE_LOOP ( 'NONE', ( #41567, #44425, #31308, #25867 ) ) ;
#5957 = CARTESIAN_POINT ( 'NONE',  ( 125.2761281442453054, 0.4262465694468514643, -12.03445270309931736 ) ) ;
#5958 = EDGE_CURVE ( 'NONE', #40637, #10734, #39999, .T. ) ;
#5959 = CARTESIAN_POINT ( 'NONE',  ( 119.8870948109119752, -0.8288870151387760510, -10.36305467784173118 ) ) ;
#5960 = DIRECTION ( 'NONE',  ( -1.224775218828352108E-16, 0.9242245927363028635, 0.3818493186865928313 ) ) ;
#5961 = CARTESIAN_POINT ( 'NONE',  ( 76.56645223742121686, 1.201885453592819397, -10.39321520033831625 ) ) ;
#5962 = CARTESIAN_POINT ( 'NONE',  ( 119.0929214775786278, -5.638512984488999180, -18.83840828888717311 ) ) ;
#5963 = CARTESIAN_POINT ( 'NONE',  ( 106.1070202545248407, -10.62599879583958717, -15.77991374673208469 ) ) ;
#5964 = CIRCLE ( 'NONE', #30751, 4.999999999999997335 ) ;
#5965 = CARTESIAN_POINT ( 'NONE',  ( 118.9227414775786400, -10.63000616557722466, -14.87417383870573495 ) ) ;
#5967 = CARTESIAN_POINT ( 'NONE',  ( 121.1350814775786233, -9.859900752359378018, -12.68260735090039759 ) ) ;
#5966 = CARTESIAN_POINT ( 'NONE',  ( 115.4624148109119943, -5.638512984488999180, -18.83840828888717311 ) ) ;
#5968 = CARTESIAN_POINT ( 'NONE',  ( 123.7445081442452874, -7.894159318335828068, -9.358103419637847864 ) ) ;
#5969 = CARTESIAN_POINT ( 'NONE',  ( 112.1845001386228944, -1.125321370491271677, -17.12283323191015683 ) ) ;
#5970 = VERTEX_POINT ( 'NONE', #32975 ) ;
#5971 = CARTESIAN_POINT ( 'NONE',  ( 124.7088614775786226, -9.565557343593413364, -10.61323700422348004 ) ) ;
#5972 = CARTESIAN_POINT ( 'NONE',  ( 123.6310548109119765, -5.638512984488995627, -18.83840828888717311 ) ) ;
#5973 = CARTESIAN_POINT ( 'NONE',  ( 67.08264006073221708, -20.21382323020432992, -10.89321520033831447 ) ) ;
#5974 = CARTESIAN_POINT ( 'NONE',  ( 108.1906140045248463, -10.62599879583958717, -11.00651665394454604 ) ) ;
#5975 = CARTESIAN_POINT ( 'NONE',  ( 111.3854577545248645, -2.791137627527939813, -18.39754474579286025 ) ) ;
#5976 = CARTESIAN_POINT ( 'NONE',  ( 112.9828796295247884, -4.863998795839590272, -19.15521520033831493 ) ) ;
#5977 = B_SPLINE_CURVE_WITH_KNOTS ( 'NONE', 3,
 ( #32777, #28934, #11602, #25513, #22091, #39417, #1550, #15472, #33000, #16376, #30278, #44654, #26410, #5646 ),
 .UNSPECIFIED., .F., .F.,
 ( 4, 2, 2, 2, 2, 2, 4 ),
 ( 0.000000000000000000, 0.1250000000000003331, 0.2500000000000006661, 0.3750000000000009992, 0.5000000000000013323, 0.7500000000000006661, 1.000000000000000000 ),
 .UNSPECIFIED. ) ;
#5978 = CARTESIAN_POINT ( 'NONE',  ( 122.6099748109119929, -9.261995988541697145, -16.69588392320189030 ) ) ;
#5979 = CARTESIAN_POINT ( 'NONE',  ( 123.7445081442452874, -7.894159318335828068, -9.358103419637847864 ) ) ;
#5980 = VERTEX_POINT ( 'NONE', #1085 ) ;
#5981 = CARTESIAN_POINT ( 'NONE',  ( 124.8223148109119762, 0.9020085738987339008, -11.91225656197089222 ) ) ;
#5982 = CARTESIAN_POINT ( 'NONE',  ( 113.6471614775786492, -4.153390946401321671, -8.397313243818183892 ) ) ;
#5983 = CARTESIAN_POINT ( 'NONE',  ( 83.44708369096697709, -25.99489077589524300, -13.39321520033831625 ) ) ;
#5984 = CARTESIAN_POINT ( 'NONE',  ( 118.9794681442453026, -9.261995988541697145, -16.69588392320189030 ) ) ;
#5985 = CARTESIAN_POINT ( 'NONE',  ( 119.5467348109119712, -4.089484607189486809, -7.948022111789456723 ) ) ;
#5986 = CARTESIAN_POINT ( 'NONE',  ( 123.5812993874819909, -6.063848558940142297, -18.38516058545102183 ) ) ;
#5987 = CARTESIAN_POINT ( 'NONE',  ( 123.5176014775786228, -0.8288870151387760510, -10.36305467784173118 ) ) ;
#5988 = CIRCLE ( 'NONE', #27124, 1.200000000000000844 ) ;
#5989 = DIRECTION ( 'NONE',  ( 0.000000000000000000, 0.000000000000000000, -1.000000000000000000 ) ) ;
#5990 = CARTESIAN_POINT ( 'NONE',  ( 123.4939235609119663, -9.645473719204776586, -14.86997237629376656 ) ) ;
#5991 = EDGE_LOOP ( 'NONE', ( #15098, #6340 ) ) ;
#5992 = DIRECTION ( 'NONE',  ( -0.8949343913984423304, 0.1703803081152067689, -0.4123869368673877545 ) ) ;
#5993 = FACE_OUTER_BOUND ( 'NONE', #38949, .T. ) ;
#5994 = VECTOR ( 'NONE', #14852, 1000.000000000000000 ) ;
#5995 = CARTESIAN_POINT ( 'NONE',  ( 122.3263414775786373, -3.505236298600246325, -18.68346056562440793 ) ) ;
#5996 = CARTESIAN_POINT ( 'NONE',  ( 106.8710046295248759, -4.863998795839590272, -18.39754474579285315 ) ) ;
#5997 = CARTESIAN_POINT ( 'NONE',  ( 111.1770983795247787, -8.402594152722688392, -16.93181055722141792 ) ) ;
#5998 = CARTESIAN_POINT ( 'NONE',  ( 118.0151148109119816, 0.4262465694468514643, -12.03445270309931736 ) ) ;
#5999 = CARTESIAN_POINT ( 'NONE',  ( 70.98136983621358809, -24.64626890834123785, -5.214987668974215396 ) ) ;
#6000 = CARTESIAN_POINT ( 'NONE',  ( 117.2209414775786485, -2.084020599724406786, -8.691656652584148546 ) ) ;
#6001 = CARTESIAN_POINT ( 'NONE',  ( 121.7590748109119687, -7.893985811506177619, -18.51759400769804742 ) ) ;
#6002 = EDGE_LOOP ( 'NONE', ( #30080, #44932, #35837, #33008, #14618 ) ) ;
#6003 = CARTESIAN_POINT ( 'NONE',  ( 120.5678148109119832, -1.833838273342659253, -17.42832698103878286 ) ) ;
#6004 = CIRCLE ( 'NONE', #9666, 4.500000000000000888 ) ;
#6005 = CARTESIAN_POINT ( 'NONE',  ( 118.1285681442453068, -7.893985811506177619, -18.51759400769804742 ) ) ;
#6006 = CARTESIAN_POINT ( 'NONE',  ( 123.4608748109119745, -10.63000616557722466, -14.87417383870573495 ) ) ;
#6007 = CARTESIAN_POINT ( 'NONE',  ( 123.9146881442452894, -10.15424416112533912, -14.75197769757731336 ) ) ;
#6008 = ORIENTED_EDGE ( 'NONE', *, *, #43865, .F. ) ;
#6009 = CARTESIAN_POINT ( 'NONE',  ( 120.6463454359119822, 0.5291689781388270175, -13.89700978578772705 ) ) ;
#6010 = CARTESIAN_POINT ( 'NONE',  ( 122.4397948109119767, -9.988377603198976828, -10.36322818467138340 ) ) ;
#6011 = CARTESIAN_POINT ( 'NONE',  ( 115.8595014775786609, -7.643976991954077427, -18.09477374809248928 ) ) ;
#6012 = CARTESIAN_POINT ( 'NONE',  ( 124.0848681442452772, -4.089484607189486809, -7.948022111789456723 ) ) ;
#6013 = CARTESIAN_POINT ( 'NONE',  ( 107.3571765045248299, -7.250697342233347165, -19.15521520033831138 ) ) ;
#6014 = CARTESIAN_POINT ( 'NONE',  ( 121.5492360609119800, -3.387241619883791355, -18.17469012370385073 ) ) ;
#6015 = ORIENTED_EDGE ( 'NONE', *, *, #23687, .F. ) ;
#6016 = CONICAL_SURFACE ( 'NONE', #8208, 2.541999999999999371, 1.047197551196596299 ) ;
#6017 = CARTESIAN_POINT ( 'NONE',  ( 72.65915383727740107, -67.60605966022829705, -40.90420006524065144 ) ) ;
#6018 = CARTESIAN_POINT ( 'NONE',  ( 107.7738952545248310, -9.868328341294098749, -15.46607636864997204 ) ) ;
#6019 = CIRCLE ( 'NONE', #35137, 1.610000000000000986 ) ;
#6020 = CARTESIAN_POINT ( 'NONE',  ( 115.4831921295247952, -9.868328341294093420, -13.39321520033836066 ) ) ;
#6021 = CARTESIAN_POINT ( 'NONE',  ( 120.0572748109119772, -6.222761293078241884, -8.102969835052219238 ) ) ;
#6022 = CARTESIAN_POINT ( 'NONE',  ( 115.7460481442453357, -10.15424416112533912, -14.75197769757731336 ) ) ;
#6023 = CARTESIAN_POINT ( 'NONE',  ( 126.4915402333614480, -0.4138374118321233586, -10.82803409125247107 ) ) ;
#6024 = ORIENTED_EDGE ( 'NONE', *, *, #28670, .F. ) ;
#6025 = CARTESIAN_POINT ( 'NONE',  ( 60.53937939559665438, -4.256997083809236138, -8.893215200338314474 ) ) ;
#6026 = CARTESIAN_POINT ( 'NONE',  ( 118.1852948109119836, -4.153390946401325223, -8.397313243818185668 ) ) ;
#6027 = CARTESIAN_POINT ( 'NONE',  ( 113.3068014775786594, -1.833838273342658809, -17.42832698103878286 ) ) ;
#6028 = CIRCLE ( 'NONE', #41288, 4.999999999999998224 ) ;
#6029 = CARTESIAN_POINT ( 'NONE',  ( 66.93334766501303079, -0.07218023934172421163, -10.39321520033831803 ) ) ;
#6030 = CARTESIAN_POINT ( 'NONE',  ( 111.3886348109119808, -3.517672760959766887, -18.63504008191830508 ) ) ;
#6032 = CARTESIAN_POINT ( 'NONE',  ( 121.6456214775786293, -10.63000616557722466, -14.87417383870573495 ) ) ;
#6031 = CARTESIAN_POINT ( 'NONE',  ( 71.27025657587988405, -26.62083706768503077, -5.176427355402450914 ) ) ;
#6033 = CARTESIAN_POINT ( 'NONE',  ( 112.7395348109119766, -5.638512984488999180, -18.83840828888717311 ) ) ;
#6034 = ORIENTED_EDGE ( 'NONE', *, *, #26253, .T. ) ;
#6035 = FACE_BOUND ( 'NONE', #28332, .T. ) ;
#6036 = DIRECTION ( 'NONE',  ( 0.000000000000000000, -0.3818493186865927203, 0.9242245927363029745 ) ) ;
#6037 = CARTESIAN_POINT ( 'NONE',  ( 116.3166296295247832, -4.863998795839590272, -19.15521520033831493 ) ) ;
#6038 = CARTESIAN_POINT ( 'NONE',  ( 126.3539348109119800, -4.153390946401325223, -8.397313243818185668 ) ) ;
#6039 = CARTESIAN_POINT ( 'NONE',  ( 119.3198281442452924, -9.859900752359374465, -12.68260735090039404 ) ) ;
#6040 = CARTESIAN_POINT ( 'NONE',  ( 82.31000308962319423, -13.76004065658516673, -16.89321520033831447 ) ) ;
#6041 = CARTESIAN_POINT ( 'NONE',  ( 115.8999108795247821, -1.325403438956436419, -16.93181055722141792 ) ) ;
#6042 = CARTESIAN_POINT ( 'NONE',  ( 116.9940348109119697, -9.988377603198960841, -10.36322818467135853 ) ) ;
#6043 = CARTESIAN_POINT ( 'NONE',  ( 64.73784058450603140, -41.08681216603740438, -7.393215200338315363 ) ) ;
#6044 = CARTESIAN_POINT ( 'NONE',  ( 114.7249681442453237, -9.565557343593413364, -10.61323700422348004 ) ) ;
#6045 = CARTESIAN_POINT ( 'NONE',  ( 111.6632702545248605, -10.62599879583958717, -15.77991374673208469 ) ) ;
#6046 = CARTESIAN_POINT ( 'NONE',  ( 88.22708560785949317, -3.622631779710408395, -8.143215200338314474 ) ) ;
#6047 = CARTESIAN_POINT ( 'NONE',  ( 112.9134265045247645, -7.250697342233347165, -19.15521520033831138 ) ) ;
#6048 = CARTESIAN_POINT ( 'NONE',  ( 124.9357681442453014, -1.834011780172310813, -8.268836392978581529 ) ) ;
#6049 = CARTESIAN_POINT ( 'NONE',  ( 121.1350814775786233, 0.5811942927096110934, -14.16772938898807510 ) ) ;
#6050 = CARTESIAN_POINT ( 'NONE',  ( 91.77400275106518279, -25.23119213852205789, -15.24166438581092109 ) ) ;
#6051 =( BOUNDED_CURVE ( )  B_SPLINE_CURVE ( 2, ( #19908, #34028, #26971, #13297, #2796, #16723, #44535, #41123, #9882, #17826, #941, #28769, #21024, #31500, #31277, #3908, #14406 ),
 .UNSPECIFIED., .F., .T. ) 
 B_SPLINE_CURVE_WITH_KNOTS ( ( 3, 2, 2, 2, 2, 2, 2, 2, 3 ),
 ( 0.7046282416568590001, 0.7109375000000000000, 0.7187500000000000000, 0.7265625000000000000, 0.7343750000000000000, 0.7421875000000000000, 0.7500000000000000000, 0.7578125000000000000, 0.7641217583431409999 ),
 .UNSPECIFIED. ) 
 CURVE ( )  GEOMETRIC_REPRESENTATION_ITEM ( )  RATIONAL_B_SPLINE_CURVE ( ( 0.9763430640195970289, 0.9385262470928680267, 1.000000000000000000, 0.9238795325112869605, 1.000000000000000000, 0.9238795325112869605, 1.000000000000000000, 0.9238795325112869605, 1.000000000000000000, 0.9238795325112869605, 1.000000000000000000, 0.9238795325112869605, 1.000000000000000000, 0.9238795325112869605, 1.000000000000000000, 0.9385262470928670275, 0.9763430640195980281 ) ) 
 REPRESENTATION_ITEM ( '' )  );
#6052 = CARTESIAN_POINT ( 'NONE',  ( 116.1431348109119881, -10.30919188438810075, -12.61870101168855918 ) ) ;
#6053 = EDGE_CURVE ( 'NONE', #29144, #10520, #23820, .T. ) ;
#6054 = CARTESIAN_POINT ( 'NONE',  ( 113.9307948109119906, 0.9020085738987339008, -11.91225656197089222 ) ) ;
#6055 = ORIENTED_EDGE ( 'NONE', *, *, #39358, .F. ) ;
#6056 = CARTESIAN_POINT ( 'NONE',  ( 114.1577014775786552, -3.505236298600246325, -18.68346056562440793 ) ) ;
#6057 = AXIS2_PLACEMENT_3D ( 'NONE', #16541, #16310, #39793 ) ;
#6058 = CARTESIAN_POINT ( 'NONE',  ( 125.1059481442452750, -8.166667518702819706, -8.995218007635861213 ) ) ;
#6059 = CARTESIAN_POINT ( 'NONE',  ( 119.2063748109119814, -1.561330072975668504, -17.79121239304076951 ) ) ;
#6060 = CARTESIAN_POINT ( 'NONE',  ( 115.1787814775786387, -9.988377603198976828, -10.36322818467138340 ) ) ;
#6061 = CONTEXT_DEPENDENT_SHAPE_REPRESENTATION ( #37262, #39444 ) ;
#6062 = CARTESIAN_POINT ( 'NONE',  ( 112.8529881442453160, -7.894159318335828068, -9.358103419637847864 ) ) ;
#6063 = VERTEX_POINT ( 'NONE', #12035 ) ;
#6064 = CARTESIAN_POINT ( 'NONE',  ( 118.0718414775786442, -0.8288870151387760510, -10.36305467784173118 ) ) ;
#6065 = CARTESIAN_POINT ( 'NONE',  ( 113.0231681442453180, -10.15424416112533912, -14.75197769757731336 ) ) ;
#6066 = CARTESIAN_POINT ( 'NONE',  ( 110.6214733795247867, -8.938348069036489818, -17.46756447353520159 ) ) ;
#6067 = AXIS2_PLACEMENT_3D ( 'NONE', #27342, #3162, #30976 ) ;
#6068 = CARTESIAN_POINT ( 'NONE',  ( 111.8716296295247901, -4.863998795839590272, -8.388885654883775800 ) ) ;
#6069 = CARTESIAN_POINT ( 'NONE',  ( 121.8725281442453223, -6.222761293078241884, -8.102969835052219238 ) ) ;
#6070 = CARTESIAN_POINT ( 'NONE',  ( 116.8250374321000606, -1.625910394394186609, -17.50100589979427568 ) ) ;
#6071 = CARTESIAN_POINT ( 'NONE',  ( 116.2471765045247594, -7.250697342233347165, -19.15521520033831138 ) ) ;
#6072 = VERTEX_POINT ( 'NONE', #43040 ) ;
#6073 = CARTESIAN_POINT ( 'NONE',  ( 123.0772048109119652, -2.527210466738041728, -8.967976844669124148 ) ) ;
#6074 = CARTESIAN_POINT ( 'NONE',  ( 121.5888948109119809, -10.30919188438810075, -12.61870101168855918 ) ) ;
#6075 = ADVANCED_FACE ( 'NONE', ( #29804 ), #12487, .T. ) ;
#6076 = FACE_OUTER_BOUND ( 'NONE', #21053, .T. ) ;
#6077 = CARTESIAN_POINT ( 'NONE',  ( 112.3991748109119868, -8.166667518702817929, -8.995218007635859436 ) ) ;
#6078 = CARTESIAN_POINT ( 'NONE',  ( 116.8014327639767771, 1.999291220100584354, -5.886126520694280551 ) ) ;
#6079 = CARTESIAN_POINT ( 'NONE',  ( 67.30914723170953096, -53.95817989580823593, -35.68060091436646530 ) ) ;
#6080 = ADVANCED_FACE ( 'NONE', ( #26158 ), #32539, .T. ) ;
#6081 = CARTESIAN_POINT ( 'NONE',  ( 109.3713171295247832, 0.1403307496149613920, -13.39321520033831447 ) ) ;
#6082 = CARTESIAN_POINT ( 'NONE',  ( 120.9451081739443055, -4.756192495830076084, -19.39047411591439385 ) ) ;
#6083 = AXIS2_PLACEMENT_3D ( 'NONE', #32583, #39442, #4092 ) ;
#6084 = CARTESIAN_POINT ( 'NONE',  ( 135.8491221887209690, -4.131696503738900184, -19.29954514867480597 ) ) ;
#6085 = EDGE_CURVE ( 'NONE', #25838, #873, #43269, .T. ) ;
#6086 = VECTOR ( 'NONE', #5317, 1000.000000000000000 ) ;
#6087 = CARTESIAN_POINT ( 'NONE',  ( 115.7628276191212819, 0.4261359969231631739, -12.14321520033831625 ) ) ;
#6088 = CARTESIAN_POINT ( 'NONE',  ( 124.7472548109119828, -7.198765429287139916, -17.81462501705270540 ) ) ;
#6089 = CARTESIAN_POINT ( 'NONE',  ( 122.2128881442453263, -7.643976991954077427, -18.09477374809248928 ) ) ;
#6090 = CARTESIAN_POINT ( 'NONE',  ( 119.7434548109119845, 0.3713923125418727711, -14.33547248937080631 ) ) ;
#6091 = ORIENTED_EDGE ( 'NONE', *, *, #44122, .F. ) ;
#6092 = CARTESIAN_POINT ( 'NONE',  ( 122.4965214775786251, -10.30919188438810075, -12.61870101168855918 ) ) ;
#6093 = CARTESIAN_POINT ( 'NONE',  ( 120.6812681442452941, -10.30919188438810075, -12.61870101168855918 ) ) ;
#6094 = CARTESIAN_POINT ( 'NONE',  ( 70.19189222814998175, -54.83461124330791847, -35.13666250696951465 ) ) ;
#6095 = CARTESIAN_POINT ( 'NONE',  ( 113.8173414775786512, -9.565557343593413364, -10.61323700422348004 ) ) ;
#6096 = CARTESIAN_POINT ( 'NONE',  ( 113.7038881442453402, -3.383040157471821630, -19.15922257007629170 ) ) ;
#6097 = EDGE_CURVE ( 'NONE', #44451, #30461, #1974, .T. ) ;
#6098 = CARTESIAN_POINT ( 'NONE',  ( 124.0848681442452772, -4.089484607189486809, -7.948022111789456723 ) ) ;
#6099 = CARTESIAN_POINT ( 'NONE',  ( 111.4549108795247747, -8.938348069036489818, -9.318865927141430916 ) ) ;
#6100 = CARTESIAN_POINT ( 'NONE',  ( 90.04708369096697140, -26.19154317501883611, -12.91723953507911915 ) ) ;
#6101 = CARTESIAN_POINT ( 'NONE',  ( 116.1082702545247827, -10.62599879583958717, -15.77991374673208469 ) ) ;
#6102 = CIRCLE ( 'NONE', #280, 2.999999999999999556 ) ;
#6103 = CARTESIAN_POINT ( 'NONE',  ( 117.2776681442452968, -4.153390946401321671, -8.397313243818183892 ) ) ;
#6104 = CARTESIAN_POINT ( 'NONE',  ( 118.1285681442453068, -2.084020599724406786, -8.691656652584148546 ) ) ;
#6105 = CARTESIAN_POINT ( 'NONE',  ( 79.05243529145373316, 4.793396140045460108, -5.736853407927685389 ) ) ;
#6106 = CARTESIAN_POINT ( 'NONE',  ( 113.3995983795247895, -8.402594152722688392, -16.93181055722141792 ) ) ;
#6107 = VERTEX_POINT ( 'NONE', #1979 ) ;
#6108 = ADVANCED_FACE ( 'NONE', ( #15450 ), #25715, .T. ) ;
#6109 = CARTESIAN_POINT ( 'NONE',  ( 109.2294421295247275, -1.212886387410460065, -16.83921471868269393 ) ) ;
#6110 = CARTESIAN_POINT ( 'NONE',  ( 114.9518748109119883, -1.834011780172310813, -8.268836392978581529 ) ) ;
#6111 = CARTESIAN_POINT ( 'NONE',  ( 113.2858169107182249, -2.467220198592768199, -17.83387418641523325 ) ) ;
#6112 = CARTESIAN_POINT ( 'NONE',  ( 121.0630641859119976, -8.321307733199551748, -9.223433127585318303 ) ) ;
#6113 = CARTESIAN_POINT ( 'NONE',  ( 121.8965016859119856, -0.6942167230862511529, -9.935906262978006609 ) ) ;
#6114 = EDGE_CURVE ( 'NONE', #41341, #2056, #43717, .T. ) ;
#6115 = EDGE_CURVE ( 'NONE', #43568, #27006, #10016, .T. ) ;
#6116 = ORIENTED_EDGE ( 'NONE', *, *, #1366, .T. ) ;
#6117 = CARTESIAN_POINT ( 'NONE',  ( 123.2687479366341421, -2.335067861339664486, -15.51187490787343215 ) ) ;
#6118 = CARTESIAN_POINT ( 'NONE',  ( 116.2659068881580708, -12.01880880694303855, -20.89321520033831447 ) ) ;
#6119 = VERTEX_POINT ( 'NONE', #39396 ) ;
#6120 = CARTESIAN_POINT ( 'NONE',  ( 117.9016614775786280, -9.988377603198976828, -10.36322818467138340 ) ) ;
#6121 = CARTESIAN_POINT ( 'NONE',  ( 126.0703014775786102, -0.1624402480850797581, -16.17319339645315424 ) ) ;
#6122 = CARTESIAN_POINT ( 'NONE',  ( 118.1285681442453068, -2.084020599724406786, -8.691656652584148546 ) ) ;
#6123 = DIRECTION ( 'NONE',  ( -0.1352586133457944206, -0.9908103287288505534, 0.000000000000000000 ) ) ;
#6124 = CARTESIAN_POINT ( 'NONE',  ( 122.7801548109119665, -3.383040157471821630, -19.15922257007629170 ) ) ;
#6125 = CARTESIAN_POINT ( 'NONE',  ( 112.9097148109120070, 0.2603800115204892296, -16.42320221600525088 ) ) ;
#6126 = AXIS2_PLACEMENT_3D ( 'NONE', #30820, #17585, #44968 ) ;
#6127 = CARTESIAN_POINT ( 'NONE',  ( 110.5520202545248054, 0.1403307496149616695, -11.32035403202665336 ) ) ;
#6128 = CARTESIAN_POINT ( 'NONE',  ( 111.8886348109120092, -6.222761293078241884, -8.102969835052219238 ) ) ;
#6129 = SURFACE_STYLE_FILL_AREA ( #36672 ) ;
#6130 = EDGE_LOOP ( 'NONE', ( #34269, #15670, #30579, #3332 ) ) ;
#6131 = CARTESIAN_POINT ( 'NONE',  ( 118.4122014775786340, 0.5811942927096110934, -14.16772938898807510 ) ) ;
#6132 = MANIFOLD_SOLID_BREP ( 'NONE', #43263 ) ;
#6133 = CARTESIAN_POINT ( 'NONE',  ( 114.8951481442453115, -8.899110576539710493, -16.42337572283490132 ) ) ;
#6134 = DIRECTION ( 'NONE',  ( 0.000000000000000000, 0.000000000000000000, -1.000000000000000000 ) ) ;
#6135 = CARTESIAN_POINT ( 'NONE',  ( 113.0231681442453322, 0.9020085738987339008, -11.91225656197089222 ) ) ;
#6136 = ORIENTED_EDGE ( 'NONE', *, *, #33165, .T. ) ;
#6137 = CARTESIAN_POINT ( 'NONE',  ( 120.1707281442453166, 0.2603800115204892296, -16.42320221600525088 ) ) ;
#6138 = DIRECTION ( 'NONE',  ( -1.000000000000000000, 0.000000000000000000, 0.000000000000000000 ) ) ;
#6139 = DIRECTION ( 'NONE',  ( 0.8636456077245080465, -0.5040994586965603652, 0.000000000000000000 ) ) ;
#6140 = CARTESIAN_POINT ( 'NONE',  ( 124.9698353663348342, -1.172797794773259072, -17.05961127468926719 ) ) ;
#6141 = FACE_OUTER_BOUND ( 'NONE', #35087, .T. ) ;
#6142 = CARTESIAN_POINT ( 'NONE',  ( 117.0507614775786465, 0.1319031606808879209, -14.10382304977623669 ) ) ;
#6143 = CARTESIAN_POINT ( 'NONE',  ( 112.6871514811013526, -2.280480477428480146, -18.08254604495227724 ) ) ;
#6144 = CARTESIAN_POINT ( 'NONE',  ( 118.3554748109119998, -9.565557343593413364, -10.61323700422348004 ) ) ;
#6145 = AXIS2_PLACEMENT_3D ( 'NONE', #34992, #38004, #27753 ) ;
#6146 = CARTESIAN_POINT ( 'NONE',  ( 65.38731723408255903, -64.53378536856919823, -40.50714483300358637 ) ) ;
#6147 = CARTESIAN_POINT ( 'NONE',  ( 117.2776681442452968, -4.153390946401325223, -8.397313243818185668 ) ) ;
#6148 = CARTESIAN_POINT ( 'NONE',  ( 113.8173414775786512, 0.2603800115204892296, -16.42320221600525088 ) ) ;
#6149 = CARTESIAN_POINT ( 'NONE',  ( 121.4103298109119748, -7.200787124940443817, -17.81845355600750835 ) ) ;
#6150 = CARTESIAN_POINT ( 'NONE',  ( 112.5126281442453120, -10.30919188438810075, -12.61870101168855918 ) ) ;
#6151 = CARTESIAN_POINT ( 'NONE',  ( 115.0086014775786509, -5.574606645277164318, -18.38911715685844683 ) ) ;
#6152 = CARTESIAN_POINT ( 'NONE',  ( 122.3830681442452857, -8.166667518702819706, -8.995218007635861213 ) ) ;
#6153 = AXIS2_PLACEMENT_3D ( 'NONE', #35103, #3886, #24209 ) ;
#6154 = CARTESIAN_POINT ( 'NONE',  ( 116.1431348109119881, 0.1319031606808879209, -14.10382304977623669 ) ) ;
#6155 = EDGE_LOOP ( 'NONE', ( #31973, #17966, #43756, #14319 ) ) ;
#6156 = CARTESIAN_POINT ( 'NONE',  ( 113.3068014775786594, -8.166667518702817929, -8.995218007635859436 ) ) ;
#6157 = EDGE_CURVE ( 'NONE', #19524, #35294, #4729, .T. ) ;
#6158 = CARTESIAN_POINT ( 'NONE',  ( 111.3160046295247838, -4.863998795839590272, -7.631215200338315796 ) ) ;
#6159 = CARTESIAN_POINT ( 'NONE',  ( 105.8292077545248446, -2.791137627527939813, -18.39754474579286025 ) ) ;
#6160 = CARTESIAN_POINT ( 'NONE',  ( 106.6626452545248611, -9.868328341294098749, -15.46607636864997204 ) ) ;
#6161 = CARTESIAN_POINT ( 'NONE',  ( 127.9787496859519393, -4.170178312457123226, -15.56602175589793191 ) ) ;
#6162 = CARTESIAN_POINT ( 'NONE',  ( 120.3976348109119812, -1.834011780172310813, -8.268836392978581529 ) ) ;
#6163 = ORIENTED_EDGE ( 'NONE', *, *, #26420, .T. ) ;
#6164 = CARTESIAN_POINT ( 'NONE',  ( 123.9584548109119737, -9.675291321254654520, -19.78473021908636298 ) ) ;
#6165 = DIRECTION ( 'NONE',  ( 0.000000000000000000, 0.6004852223388319477, -0.7996358532186282897 ) ) ;
#6166 = CARTESIAN_POINT ( 'NONE',  ( 113.0231681442453180, -10.15424416112533912, -14.75197769757731336 ) ) ;
#6167 = CARTESIAN_POINT ( 'NONE',  ( 123.3550173109119612, 0.2312338769422730977, -16.08380026872395163 ) ) ;
#6168 = CARTESIAN_POINT ( 'NONE',  ( 122.2696148109119889, -4.089484607189486809, -7.948022111789456723 ) ) ;
#6169 = CARTESIAN_POINT ( 'NONE',  ( 114.5108483795247878, -8.402594152722688392, -16.93181055722141792 ) ) ;
#6170 = CARTESIAN_POINT ( 'NONE',  ( 89.25356269854076174, -10.05861921418335392, -13.77344656902741526 ) ) ;
#6171 = ORIENTED_EDGE ( 'NONE', *, *, #20591, .F. ) ;
#6172 = CARTESIAN_POINT ( 'NONE',  ( 111.7184548109119788, -9.261995988541697145, -16.69588392320189030 ) ) ;
#6173 = CARTESIAN_POINT ( 'NONE',  ( 122.3830681442452857, -1.833838273342659697, -17.42832698103878286 ) ) ;
#6174 = CARTESIAN_POINT ( 'NONE',  ( 118.2420214775786320, -3.383040157471821630, -19.15922257007629170 ) ) ;
#6175 = CARTESIAN_POINT ( 'NONE',  ( 113.4202548109119846, 0.1319031606808879209, -14.10382304977623669 ) ) ;
#6176 = CARTESIAN_POINT ( 'NONE',  ( 116.8805814775786445, -6.344957434206662583, -7.627207830600332805 ) ) ;
#6177 = DIRECTION ( 'NONE',  ( -0.000000000000000000, -0.9284778069183718952, -0.3713878862591649677 ) ) ;
#6178 = EDGE_CURVE ( 'NONE', #13605, #2957, #41436, .T. ) ;
#6179 = CARTESIAN_POINT ( 'NONE',  ( 75.95778847736481509, -3.256761025687722189, -7.993215200338315007 ) ) ;
#6180 = CARTESIAN_POINT ( 'NONE',  ( 119.4332814775786318, -8.899110576539710493, -16.42337572283490132 ) ) ;
#6181 = VERTEX_POINT ( 'NONE', #34338 ) ;
#6182 = AXIS2_PLACEMENT_3D ( 'NONE', #38314, #6654, #41101 ) ;
#6183 = CARTESIAN_POINT ( 'NONE',  ( 122.7299391859119737, -8.844754642576884152, -8.592115655440050404 ) ) ;
#6184 = DIRECTION ( 'NONE',  ( -0.7871354856660162103, -0.4483307682966942709, -0.4235767337848251879 ) ) ;
#6185 = CARTESIAN_POINT ( 'NONE',  ( 122.8368814775786291, -7.894159318335828068, -9.358103419637847864 ) ) ;
#6186 = EDGE_LOOP ( 'NONE', ( #1401, #44303, #32862, #27899, #2709 ) ) ;
#6187 = CARTESIAN_POINT ( 'NONE',  ( 124.6746266859119743, -9.033780868592240054, -16.85052413769862056 ) ) ;
#6188 = CARTESIAN_POINT ( 'NONE',  ( 137.3930029278033658, -0.4326168857421066605, -10.81500932932321035 ) ) ;
#6189 = CARTESIAN_POINT ( 'NONE',  ( 119.3765548109119834, 0.9020085738987339008, -11.91225656197089222 ) ) ;
#6190 = CIRCLE ( 'NONE', #16385, 2.445500000000004448 ) ;
#6191 = CARTESIAN_POINT ( 'NONE',  ( 111.2465515045248168, -2.477300249445798297, -7.631215200338321125 ) ) ;
#6192 = CARTESIAN_POINT ( 'NONE',  ( 117.5613014775786525, -10.15424416112533912, -14.75197769757731336 ) ) ;
#6193 = ORIENTED_EDGE ( 'NONE', *, *, #24193, .T. ) ;
#6194 = ORIENTED_EDGE ( 'NONE', *, *, #10583, .T. ) ;
#6195 = CARTESIAN_POINT ( 'NONE',  ( 125.6732148109119862, -9.859900752359378018, -12.68260735090039759 ) ) ;
#6196 = CARTESIAN_POINT ( 'NONE',  ( 122.3263414775786373, -3.505236298600246325, -18.68346056562440793 ) ) ;
#6197 = FACE_BOUND ( 'NONE', #15997, .T. ) ;
#6198 = DIRECTION ( 'NONE',  ( 0.000000000000000000, 0.000000000000000000, -1.000000000000000000 ) ) ;
#6199 = CARTESIAN_POINT ( 'NONE',  ( 123.8012348109119642, 0.2603800115204892296, -16.42320221600525088 ) ) ;
#6200 = CARTESIAN_POINT ( 'NONE',  ( 112.1722337524184070, -8.900133558646924570, -16.42203216583235204 ) ) ;
#6201 = CARTESIAN_POINT ( 'NONE',  ( 120.1140014775786398, -1.561330072975668504, -17.79121239304076951 ) ) ;
#6203 = CARTESIAN_POINT ( 'NONE',  ( 118.1852948109119836, -4.153390946401325223, -8.397313243818185668 ) ) ;
#6202 = CARTESIAN_POINT ( 'NONE',  ( 118.2987481442453088, -1.561330072975668504, -17.79121239304076951 ) ) ;
#6204 = CARTESIAN_POINT ( 'NONE',  ( 70.19189222814998175, -52.04917782255280656, -34.02249884819201498 ) ) ;
#6205 = CARTESIAN_POINT ( 'NONE',  ( 112.1111981407226210, -1.081026697600516950, -17.18181821144401411 ) ) ;
#6206 = MANIFOLD_SOLID_BREP ( 'NONE', #17774 ) ;
#6207 = ORIENTED_EDGE ( 'NONE', *, *, #14497, .F. ) ;
#6208 = CARTESIAN_POINT ( 'NONE',  ( 123.8012348109119642, -9.565557343593413364, -10.61323700422348004 ) ) ;
#6209 = DIRECTION ( 'NONE',  ( 0.000000000000000000, 0.000000000000000000, -1.000000000000000000 ) ) ;
#6210 = CARTESIAN_POINT ( 'NONE',  ( 121.1899213555256409, -8.364211927971188842, -17.30190421972978143 ) ) ;
#6211 = VECTOR ( 'NONE', #19034, 1000.000000000000000 ) ;
#6212 = CARTESIAN_POINT ( 'NONE',  ( 109.4407702545248355, -10.62599879583958717, -15.77991374673208469 ) ) ;
#6213 = CARTESIAN_POINT ( 'NONE',  ( 114.4413952545248350, -9.868328341294098749, -15.46607636864997204 ) ) ;
#6214 = CARTESIAN_POINT ( 'NONE',  ( 105.7597546295248350, -4.863998795839590272, -7.631215200338315796 ) ) ;
#6215 = CARTESIAN_POINT ( 'NONE',  ( 123.9146881442452894, 0.9020085738987339008, -11.91225656197089222 ) ) ;
#6216 = CARTESIAN_POINT ( 'NONE',  ( 121.8158014775786171, -4.153390946401325223, -8.397313243818185668 ) ) ;
#6217 = VERTEX_POINT ( 'NONE', #16126 ) ;
#6218 = CARTESIAN_POINT ( 'NONE',  ( 123.4041481442452834, -10.30919188438810075, -12.61870101168855918 ) ) ;
#6219 = CARTESIAN_POINT ( 'NONE',  ( 112.4559014775786778, -0.1624402480850797581, -16.17319339645315424 ) ) ;
#6220 = CARTESIAN_POINT ( 'NONE',  ( 64.84865456828643460, -21.86021636429758530, -5.893215200338315363 ) ) ;
#6221 = CARTESIAN_POINT ( 'NONE',  ( 121.4754414775786131, -8.166667518702819706, -8.995218007635861213 ) ) ;
#6222 = CARTESIAN_POINT ( 'NONE',  ( 121.8725281442453223, -3.383040157471821630, -19.15922257007629170 ) ) ;
#6224 = AXIS2_PLACEMENT_3D ( 'NONE', #6025, #2605, #24055 ) ;
#6223 = DIRECTION ( 'NONE',  ( 0.000000000000000000, 0.4669533266896290780, 0.8842819633428518067 ) ) ;
#6225 = CARTESIAN_POINT ( 'NONE',  ( 114.3278814775786429, -10.30919188438810075, -12.61870101168855918 ) ) ;
#6226 = CARTESIAN_POINT ( 'NONE',  ( 115.9162281442453235, -4.089484607189486809, -7.948022111789456723 ) ) ;
#6227 = CARTESIAN_POINT ( 'NONE',  ( 59.62174278132244609, -14.86814543204979344, -18.19321520033831519 ) ) ;
#6228 = ORIENTED_EDGE ( 'NONE', *, *, #16934, .F. ) ;
#6229 = DIRECTION ( 'NONE',  ( 1.000000000000000000, 0.000000000000000000, -0.000000000000000000 ) ) ;
#6230 = DIRECTION ( 'NONE',  ( 0.000000000000000000, 0.6004852223388321697, -0.7996358532186279566 ) ) ;
#6231 = CARTESIAN_POINT ( 'NONE',  ( 124.9357681442453014, -7.643976991954077427, -18.09477374809248928 ) ) ;
#6232 = ADVANCED_FACE ( 'NONE', ( #34116 ), #6538, .F. ) ;
#6233 = CARTESIAN_POINT ( 'NONE',  ( 107.8433483795247838, -8.402594152722688392, -16.93181055722141792 ) ) ;
#6234 = CARTESIAN_POINT ( 'NONE',  ( 112.1494421295248003, -9.868328341294093420, -13.39321520033831447 ) ) ;
#6235 = CARTESIAN_POINT ( 'NONE',  ( 116.4267681442453153, -6.222761293078241884, -8.102969835052219238 ) ) ;
#6236 = CARTESIAN_POINT ( 'NONE',  ( 79.00611218289952831, -44.99489077589586827, -4.893215200338314474 ) ) ;
#6237 = CARTESIAN_POINT ( 'NONE',  ( 117.9016614775786280, -0.1624402480850797581, -16.17319339645315424 ) ) ;
#6238 = CARTESIAN_POINT ( 'NONE',  ( 124.3117748109119844, -10.30919188438810075, -12.61870101168855918 ) ) ;
#6239 = ORIENTED_EDGE ( 'NONE', *, *, #2158, .T. ) ;
#6240 = CARTESIAN_POINT ( 'NONE',  ( 124.0281414775786146, -7.643976991954077427, -18.09477374809248928 ) ) ;
#6241 = CARTESIAN_POINT ( 'NONE',  ( 119.0929214775786278, -5.638512984488999180, -18.83840828888717311 ) ) ;
#6242 = CARTESIAN_POINT ( 'NONE',  ( 125.4463081442452932, -5.638512984488999180, -18.83840828888717311 ) ) ;
#6243 = AXIS2_PLACEMENT_3D ( 'NONE', #30226, #12229, #5589 ) ;
#6244 = CARTESIAN_POINT ( 'NONE',  ( 122.7234281442452755, -4.153390946401325223, -8.397313243818185668 ) ) ;
#6245 = VERTEX_POINT ( 'NONE', #16584 ) ;
#6246 = CARTESIAN_POINT ( 'NONE',  ( 120.4379860609119675, -3.387241619883791355, -18.17469012370385073 ) ) ;
#6247 = VECTOR ( 'NONE', #6312, 1000.000000000000000 ) ;
#6248 = CARTESIAN_POINT ( 'NONE',  ( 124.4819548109119722, -7.893985811506177619, -18.51759400769804742 ) ) ;
#6249 = EDGE_CURVE ( 'NONE', #40888, #36261, #27486, .T. ) ;
#6250 = CARTESIAN_POINT ( 'NONE',  ( 113.4202548109119846, 0.1319031606808879209, -14.10382304977623669 ) ) ;
#6251 = CARTESIAN_POINT ( 'NONE',  ( 123.6877814775786533, -3.383040157471821630, -19.15922257007629170 ) ) ;
#6252 = CARTESIAN_POINT ( 'NONE',  ( 117.5284876054816152, -2.287189184988681401, -18.07361239780446738 ) ) ;
#6253 = VECTOR ( 'NONE', #27239, 1000.000000000000000 ) ;
#6254 = CARTESIAN_POINT ( 'NONE',  ( 124.4662673109119737, -9.289237151508434209, -11.05642687123711276 ) ) ;
#6255 = ORIENTED_EDGE ( 'NONE', *, *, #4687, .F. ) ;
#6256 = CARTESIAN_POINT ( 'NONE',  ( 78.93021946355167984, -3.662536865724447921, -12.39321520033831447 ) ) ;
#6257 = CARTESIAN_POINT ( 'NONE',  ( 109.2324108795247923, -1.325403438956436419, -16.93181055722141792 ) ) ;
#6258 = VECTOR ( 'NONE', #12751, 1000.000000000000000 ) ;
#6259 = CARTESIAN_POINT ( 'NONE',  ( 94.20708369096698220, -25.99489077589524300, -13.39321520033831447 ) ) ;
#6260 = CARTESIAN_POINT ( 'NONE',  ( 123.0070614775786169, -10.15424416112533912, -14.75197769757731336 ) ) ;
#6261 = CARTESIAN_POINT ( 'NONE',  ( 113.7038881442453402, -6.222761293078241884, -8.102969835052219238 ) ) ;
#6262 = CARTESIAN_POINT ( 'NONE',  ( 126.2640359059496973, -5.823073642834863506, -18.32360385354721544 ) ) ;
#6263 = ORIENTED_EDGE ( 'NONE', *, *, #1622, .F. ) ;
#6264 = CYLINDRICAL_SURFACE ( 'NONE', #38947, 5.132259260909266985 ) ;
#6265 = CARTESIAN_POINT ( 'NONE',  ( 120.5678148109119832, -1.833838273342659253, -17.42832698103878286 ) ) ;
#6266 = CARTESIAN_POINT ( 'NONE',  ( 114.0442481442453300, -7.643976991954077427, -18.09477374809248928 ) ) ;
#6267 = DIRECTION ( 'NONE',  ( 0.000000000000000000, 0.000000000000000000, -1.000000000000000000 ) ) ;
#6268 = FACE_OUTER_BOUND ( 'NONE', #37286, .T. ) ;
#6270 = DIRECTION ( 'NONE',  ( -1.000000000000000000, 0.000000000000000000, 0.000000000000000000 ) ) ;
#6269 = CARTESIAN_POINT ( 'NONE',  ( -7.923679509334008664, -5.078949698970065540, -8.893215200338314474 ) ) ;
#6271 = AXIS2_PLACEMENT_3D ( 'NONE', #43628, #43406, #1887 ) ;
#6272 = CARTESIAN_POINT ( 'NONE',  ( 112.0020881442453344, 0.2603800115204892296, -16.42320221600525088 ) ) ;
#6273 = ORIENTED_EDGE ( 'NONE', *, *, #13370, .T. ) ;
#6274 = CARTESIAN_POINT ( 'NONE',  ( 112.1155414775786454, 0.9020085738987339008, -11.91225656197089222 ) ) ;
#6275 = CARTESIAN_POINT ( 'NONE',  ( 127.7429221096626151, 0.4604311707933653741, -15.59844375728449073 ) ) ;
#6276 = CARTESIAN_POINT ( 'NONE',  ( 115.8304577545247582, -7.250697342233347165, -7.631215200338321125 ) ) ;
#6277 = CARTESIAN_POINT ( 'NONE',  ( 123.8579614775786126, -9.859900752359378018, -12.68260735090039759 ) ) ;
#6278 = CARTESIAN_POINT ( 'NONE',  ( 121.6456214775786293, 0.4262465694468514643, -12.03445270309931736 ) ) ;
#6279 = CARTESIAN_POINT ( 'NONE',  ( 0.04488520489200759078, -6.166763362545027327, -8.593215200338315540 ) ) ;
#6280 = CARTESIAN_POINT ( 'NONE',  ( 114.9275671295247889, 0.1403307496149613920, -13.39321520033831447 ) ) ;
#6281 = CARTESIAN_POINT ( 'NONE',  ( 111.4549108795247747, -8.938348069036489818, -9.318865927141430916 ) ) ;
#6282 = DIRECTION ( 'NONE',  ( -1.000000000000000000, 0.000000000000000000, 0.000000000000000000 ) ) ;
#6283 = CARTESIAN_POINT ( 'NONE',  ( 105.8292077545248446, -7.250697342233347165, -7.631215200338321125 ) ) ;
#6284 = CARTESIAN_POINT ( 'NONE',  ( 88.73939138327467901, -25.99489077589524300, -13.39321520033831625 ) ) ;
#6285 = CARTESIAN_POINT ( 'NONE',  ( 115.6220983795247861, -0.7896495226426338832, -9.318865927141430916 ) ) ;
#6286 = CARTESIAN_POINT ( 'NONE',  ( 125.1059481442452750, -8.166667518702819706, -8.995218007635861213 ) ) ;
#6287 = CARTESIAN_POINT ( 'NONE',  ( 123.0637881442452937, -0.4660016031367893996, -10.09054647747474043 ) ) ;
#6288 = CARTESIAN_POINT ( 'NONE',  ( 70.19189222814998175, -56.33107134722149567, -35.73524133214168330 ) ) ;
#6289 = CARTESIAN_POINT ( 'NONE',  ( 118.8660148109119774, -10.30919188438810075, -12.61870101168855918 ) ) ;
#6290 = CARTESIAN_POINT ( 'NONE',  ( 112.6260814775786514, -9.261995988541697145, -16.69588392320189030 ) ) ;
#6291 = VERTEX_POINT ( 'NONE', #37994 ) ;
#6292 = CARTESIAN_POINT ( 'NONE',  ( 109.4154010812577837, -0.01829820670803256055, -12.14321520033831625 ) ) ;
#6293 = AXIS2_PLACEMENT_3D ( 'NONE', #449, #10948, #39202 ) ;
#6294 = CARTESIAN_POINT ( 'NONE',  ( 111.6617281442453304, 0.4262465694468514643, -12.03445270309931736 ) ) ;
#6295 = CARTESIAN_POINT ( 'NONE',  ( 124.0848681442452772, -4.089484607189486809, -7.948022111789456723 ) ) ;
#6296 = CARTESIAN_POINT ( 'NONE',  ( 115.5758681442453053, -1.561330072975668060, -17.79121239304076951 ) ) ;
#6297 = APPLICATION_PROTOCOL_DEFINITION ( 'draft international standard', 'automotive_design', 1998, #2041 ) ;
#6298 = CARTESIAN_POINT ( 'NONE',  ( 112.2857214775786474, -5.574606645277164318, -18.38911715685844683 ) ) ;
#6299 = ORIENTED_EDGE ( 'NONE', *, *, #9249, .F. ) ;
#6300 = CARTESIAN_POINT ( 'NONE',  ( 117.8449348109119938, -1.833838273342659253, -17.42832698103878286 ) ) ;
#6301 = CARTESIAN_POINT ( 'NONE',  ( 111.7751814775786556, -7.893985811506177619, -18.51759400769804742 ) ) ;
#6302 = CARTESIAN_POINT ( 'NONE',  ( 108.8156921295247912, -9.868328341294093420, -13.39321520033831447 ) ) ;
#6303 = CARTESIAN_POINT ( 'NONE',  ( 124.3685014775786328, 0.4262465694468514643, -12.03445270309931736 ) ) ;
#6304 = LINE ( 'NONE', #37762, #44953 ) ;
#6305 = AXIS2_PLACEMENT_3D ( 'NONE', #27455, #37006, #5556 ) ;
#6306 = CARTESIAN_POINT ( 'NONE',  ( 113.6079577545248043, -7.250697342233347165, -7.631215200338321125 ) ) ;
#6307 = VERTEX_POINT ( 'NONE', #20456 ) ;
#6308 = DIRECTION ( 'NONE',  ( 0.9609149988134837450, -0.1028163501681639419, 0.2570431154366518145 ) ) ;
#6309 = CARTESIAN_POINT ( 'NONE',  ( 72.54180985774836188, -62.51387108299115170, -37.47916665824249804 ) ) ;
#6310 = FACE_OUTER_BOUND ( 'NONE', #20929, .T. ) ;
#6311 = CARTESIAN_POINT ( 'NONE',  ( 112.7395348109119766, -5.638512984488999180, -18.83840828888717311 ) ) ;
#6312 = DIRECTION ( 'NONE',  ( 0.000000000000000000, 0.000000000000000000, -1.000000000000000000 ) ) ;
#6313 = FACE_OUTER_BOUND ( 'NONE', #15783, .T. ) ;
#6314 = CARTESIAN_POINT ( 'NONE',  ( 108.1906140045248463, 0.1403307496149616695, -15.46607636864997204 ) ) ;
#6315 = EDGE_CURVE ( 'NONE', #30207, #26522, #15827, .T. ) ;
#6316 = CYLINDRICAL_SURFACE ( 'NONE', #37492, 1.999999999999998890 ) ;
#6317 = AXIS2_PLACEMENT_3D ( 'NONE', #3171, #27576, #41488 ) ;
#6318 = CARTESIAN_POINT ( 'NONE',  ( 119.3765548109119834, 0.9020085738987339008, -11.91225656197089222 ) ) ;
#6319 = CARTESIAN_POINT ( 'NONE',  ( 122.6150890224331675, -4.681800857092183854, -18.57451437749315559 ) ) ;
#6320 = FACE_OUTER_BOUND ( 'NONE', #12308, .T. ) ;
#6321 = CARTESIAN_POINT ( 'NONE',  ( 123.9800954359119771, 0.5291689781388532188, -13.89700978578742152 ) ) ;
#6322 = CARTESIAN_POINT ( 'NONE',  ( 122.7234281442452755, -4.153390946401325223, -8.397313243818185668 ) ) ;
#6323 = CARTESIAN_POINT ( 'NONE',  ( 119.7434548109119561, -4.722584480144054631, -19.03897489626359274 ) ) ;
#6324 = ORIENTED_EDGE ( 'NONE', *, *, #10043, .T. ) ;
#6325 = CARTESIAN_POINT ( 'NONE',  ( 75.14134903615895666, -42.50702760616825771, -10.89321520033831447 ) ) ;
#6326 = CARTESIAN_POINT ( 'NONE',  ( 119.8303681442453126, -10.63000616557722466, -14.87417383870573495 ) ) ;
#6327 = CARTESIAN_POINT ( 'NONE',  ( 89.40092984481313465, -25.99489077589524300, -13.39321520033831625 ) ) ;
#6328 = CARTESIAN_POINT ( 'NONE',  ( 115.5758681442453053, -7.894159318335828068, -9.358103419637847864 ) ) ;
#6329 =( BOUNDED_SURFACE ( )  B_SPLINE_SURFACE ( 1, 2, ( 
 ( #31972, #25595, #1410, #39501, #25150, #14656, #5056, #43370, #8263, #22168, #39274, #22393, #36288, #36062, #8037, #734, #4831, #39045, #15550, #18971, #32860, #29457, #21943, #35834, #18753, #7817, #39947, #8709, #43144, #4386, #18300, #15328, #4608, #36512, #32195, #5286, #968, #14885, #32642, #25814, #29914, #33080, #12595, #20111, #37422, #33530, #44056, #2308, #30584, #2082, #9617, #5725, #9166, #43594, #43828, #13268, #16238, #44288, #19643, #33997, #15780, #16462, #44505, #30141, #23762, #37181, #26267, #37652, #36954, #2768, #26940, #12822, #5499, #40174, #30366, #33307, #26498, #29683, #2536, #40406, #12367, #26720, #23070, #40629, #19420, #8939, #23537, #9386, #13041, #27174, #41095, #1852, #19202, #19879, #23296, #6192, #22842, #5954, #33767, #36734, #40864, #9854, #16692, #16006, #30813, #7086, #10517, #27401, #20779, #17362, #44737, #14377, #2993, #27625, #34869, #10082, #16919, #13718, #31250, #24865, #10742, #17800, #13496, #20995, #34438, #24641, #23985, #35096, #3217, #21220, #31694, #22, #42199, #24203, #3878, #38309, #41323, #6870, #17144, #10302, #44961, #3657, #6427, #462, #37873, #13935, #3443, #31030, #6649, #41539, #20337, #28290, #10960, #34658, #20557, #27847, #38094, #31470, #34220, #41757, #24419, #17578, #7301, #243, #14152, #28068, #41977, #38523, #18019, #11859, #11629, #25765, #28965, #911, #14600, #43316, #28741, #21442, #35328, #28520, #25541, #42646, #42425, #39448, #39671, #32143, #14831, #42872, #31917, #11414, #1576, #8210, #8435, #18698, #682, #25092, #39216, #11189, #4097, #22117, #12085, #38756, #25323, #7758, #35784, #7526, #38987, #7980, #21888, #1358, #43091, #36007, #15054, #21666, #29178, #4779, #35554, #36235, #29404, #4326, #18247, #4553, #18479, #15270, #32368, #22340, #1135, #15497, #32589, #5001, #18914, #32806, #25990, #33472, #2252, #16181, #12537, #2708, #26662, #22783, #23011, #16635, #26886, #5899, #36677, #19367, #36458, #40805, #5447, #33256, #36901, #29628, #8882, #39895, #2481, #16405, #19591 ),
 ( #29856, #2028, #12762, #44450, #23477, #22557, #5673, #30085, #15953, #5228, #43771, #8656, #9561, #30529, #9108, #19142, #43999, #26440, #19822, #37363, #33025, #40575, #1799, #6135, #26210, #15727, #40347, #20055, #9335, #43543, #44230, #23244, #12990, #37125, #33709, #12313, #40118, #30305, #33938, #9796, #34164, #31199, #3167, #16866, #13877, #181, #6589, #20506, #3390, #6368, #34385, #21160, #45121, #28015, #38253, #20279, #44681, #13663, #30757, #41040, #17309, #17742, #31638, #17089, #27347, #10242, #13217, #13442, #30980, #44906, #20945, #17517, #27788, #34605, #27116, #3602, #24367, #41267, #10686, #3818, #23706, #2936, #24150, #38042, #34819, #6818, #31414, #20725, #35037, #37598, #10026, #41701, #41484, #23933, #10466, #7035, #14098, #27572, #37814, #41920, #24588, #38471, #7247, #1305, #25488, #42369, #38925, #10906, #15217, #11130, #7695, #11352, #4043, #28461, #407, #22062, #35954, #25033, #29124, #25711, #14544, #43035, #36179, #14323, #21383, #25263, #39159, #4725, #42591, #18642, #7924, #8379, #42146, #28237, #21834, #28687, #24806, #35727, #4501, #18424, #32084, #22286, #1081, #21611, #32316, #4946, #11803, #39391, #35498, #4270, #38698, #39618, #18189, #853, #14995, #17965, #14772, #7466, #32535, #18859, #28908, #35266, #31864, #42817, #631, #11579, #8157, #19541, #39842, #33200, #29575, #36625, #26154, #33418, #6074, #30251, #29351, #12484, #29801, #43492, #43265, #15672, #32751, #16350, #37308, #15901, #25934, #26382, #5400, #12708, #44176, #23421, #40293, #1524, #33648, #32972, #22506, #1976, #12939, #12260, #12031, #5845, #5618, #19767, #22957, #40061, #8604, #15445, #22726, #36399, #5169, #19086, #2197, #19316, #1749, #16123, #2426, #8824, #43713, #36849, #9057, #30027, #40749, #43943, #26836, #26608, #40523, #9285, #23192, #37072, #9506, #10191, #24535, #38425, #9970, #34114, #17037, #19997, #37537, #23881, #37766, #27741, #24321, #24098, #41434, #33881, #10413, #31144, #37991, #27295, #40985, #2650, #6536, #16582, #30477, #9739, #6767 ) ),
 .UNSPECIFIED., .F., .F., .F. ) 
 B_SPLINE_SURFACE_WITH_KNOTS ( ( 2, 2 ),
 ( 3, 2, 2, 2, 2, 2, 2, 2, 2, 2, 2, 2, 2, 2, 2, 2, 2, 2, 2, 2, 2, 2, 2, 2, 2, 2, 2, 2, 2, 2, 2, 2, 2, 2, 2, 2, 2, 2, 2, 2, 2, 2, 2, 2, 2, 2, 2, 2, 2, 2, 2, 2, 2, 2, 2, 2, 2, 2, 2, 2, 2, 2, 2, 2, 2, 2, 2, 2, 2, 2, 2, 2, 2, 2, 2, 2, 2, 2, 2, 2, 2, 2, 2, 2, 2, 2, 2, 2, 2, 2, 2, 2, 2, 2, 2, 2, 2, 2, 2, 2, 2, 2, 2, 2, 2, 2, 2, 2, 2, 2, 2, 2, 2, 2, 2, 2, 2, 2, 2, 2, 2, 2, 2, 2, 2, 2, 2, 2, 3 ),
 ( 0.000000000000000000, 1.000000000000000000 ),
 ( 0.000000000000000000, 0.007812500000000000000, 0.01562500000000000000, 0.02343750000000000000, 0.03125000000000000000, 0.03906250000000000000, 0.04687500000000000000, 0.05468750000000000000, 0.06250000000000000000, 0.07031250000000000000, 0.07812500000000000000, 0.08593750000000000000, 0.09375000000000000000, 0.1015625000000000000, 0.1093750000000000000, 0.1171875000000000000, 0.1250000000000000000, 0.1328125000000000000, 0.1406250000000000000, 0.1484375000000000000, 0.1562500000000000000, 0.1640625000000000000, 0.1718750000000000000, 0.1796875000000000000, 0.1875000000000000000, 0.1953125000000000000, 0.2031250000000000000, 0.2109375000000000000, 0.2187500000000000000, 0.2265625000000000000, 0.2343750000000000000, 0.2421875000000000000, 0.2500000000000000000, 0.2578125000000000000, 0.2656250000000000000, 0.2734375000000000000, 0.2812500000000000000, 0.2890625000000000000, 0.2968750000000000000, 0.3046875000000000000, 0.3125000000000000000, 0.3203125000000000000, 0.3281250000000000000, 0.3359375000000000000, 0.3437500000000000000, 0.3515625000000000000, 0.3593750000000000000, 0.3671875000000000000, 0.3750000000000000000, 0.3828125000000000000, 0.3906250000000000000, 0.3984375000000000000, 0.4062500000000000000, 0.4140625000000000000, 0.4218750000000000000, 0.4296875000000000000, 0.4375000000000000000, 0.4453125000000000000, 0.4531250000000000000, 0.4609375000000000000, 0.4687500000000000000, 0.4765625000000000000, 0.4843750000000000000, 0.4921875000000000000, 0.5000000000000000000, 0.5078125000000000000, 0.5156250000000000000, 0.5234375000000000000, 0.5312500000000000000, 0.5390625000000000000, 0.5468750000000000000, 0.5546875000000000000, 0.5625000000000000000, 0.5703125000000000000, 0.5781250000000000000, 0.5859375000000000000, 0.5937500000000000000, 0.6015625000000000000, 0.6093750000000000000, 0.6171875000000000000, 0.6250000000000000000, 0.6328125000000000000, 0.6406250000000000000, 0.6484375000000000000, 0.6562500000000000000, 0.6640625000000000000, 0.6718750000000000000, 0.6796875000000000000, 0.6875000000000000000, 0.6953125000000000000, 0.7031250000000000000, 0.7109375000000000000, 0.7187500000000000000, 0.7265625000000000000, 0.7343750000000000000, 0.7421875000000000000, 0.7500000000000000000, 0.7578125000000000000, 0.7656250000000000000, 0.7734375000000000000, 0.7812500000000000000, 0.7890625000000000000, 0.7968750000000000000, 0.8046875000000000000, 0.8125000000000000000, 0.8203125000000000000, 0.8281250000000000000, 0.8359375000000000000, 0.8437500000000000000, 0.8515625000000000000, 0.8593750000000000000, 0.8671875000000000000, 0.8750000000000000000, 0.8828125000000000000, 0.8906250000000000000, 0.8984375000000000000, 0.9062500000000000000, 0.9140625000000000000, 0.9218750000000000000, 0.9296875000000000000, 0.9375000000000000000, 0.9453125000000000000, 0.9531250000000000000, 0.9609375000000000000, 0.9687500000000000000, 0.9765625000000000000, 0.9843750000000000000, 0.9921875000000000000, 1.000000000000000000 ),
 .UNSPECIFIED. ) 
 GEOMETRIC_REPRESENTATION_ITEM ( )  RATIONAL_B_SPLINE_SURFACE ( (
 ( 1.000000000000000000, 0.9238795325112869605, 1.000000000000000000, 0.9238795325112869605, 1.000000000000000000, 0.9238795325112869605, 1.000000000000000000, 0.9238795325112869605, 1.000000000000000000, 0.9238795325112869605, 1.000000000000000000, 0.9238795325112869605, 1.000000000000000000, 0.9238795325112869605, 1.000000000000000000, 0.9238795325112869605, 1.000000000000000000, 0.9238795325112869605, 1.000000000000000000, 0.9238795325112869605, 1.000000000000000000, 0.9238795325112869605, 1.000000000000000000, 0.9238795325112869605, 1.000000000000000000, 0.9238795325112869605, 1.000000000000000000, 0.9238795325112869605, 1.000000000000000000, 0.9238795325112869605, 1.000000000000000000, 0.9238795325112869605, 1.000000000000000000, 0.9238795325112869605, 1.000000000000000000, 0.9238795325112869605, 1.000000000000000000, 0.9238795325112869605, 1.000000000000000000, 0.9238795325112869605, 1.000000000000000000, 0.9238795325112869605, 1.000000000000000000, 0.9238795325112869605, 1.000000000000000000, 0.9238795325112869605, 1.000000000000000000, 0.9238795325112869605, 1.000000000000000000, 0.9238795325112869605, 1.000000000000000000, 0.9238795325112869605, 1.000000000000000000, 0.9238795325112869605, 1.000000000000000000, 0.9238795325112869605, 1.000000000000000000, 0.9238795325112869605, 1.000000000000000000, 0.9238795325112869605, 1.000000000000000000, 0.9238795325112869605, 1.000000000000000000, 0.9238795325112869605, 1.000000000000000000, 0.9238795325112869605, 1.000000000000000000, 0.9238795325112869605, 1.000000000000000000, 0.9238795325112869605, 1.000000000000000000, 0.9238795325112869605, 1.000000000000000000, 0.9238795325112869605, 1.000000000000000000, 0.9238795325112869605, 1.000000000000000000, 0.9238795325112869605, 1.000000000000000000, 0.9238795325112869605, 1.000000000000000000, 0.9238795325112869605, 1.000000000000000000, 0.9238795325112869605, 1.000000000000000000, 0.9238795325112869605, 1.000000000000000000, 0.9238795325112869605, 1.000000000000000000, 0.9238795325112869605, 1.000000000000000000, 0.9238795325112869605, 1.000000000000000000, 0.9238795325112869605, 1.000000000000000000, 0.9238795325112869605, 1.000000000000000000, 0.9238795325112869605, 1.000000000000000000, 0.9238795325112869605, 1.000000000000000000, 0.9238795325112869605, 1.000000000000000000, 0.9238795325112869605, 1.000000000000000000, 0.9238795325112869605, 1.000000000000000000, 0.9238795325112869605, 1.000000000000000000, 0.9238795325112869605, 1.000000000000000000, 0.9238795325112869605, 1.000000000000000000, 0.9238795325112869605, 1.000000000000000000, 0.9238795325112869605, 1.000000000000000000, 0.9238795325112869605, 1.000000000000000000, 0.9238795325112869605, 1.000000000000000000, 0.9238795325112869605, 1.000000000000000000, 0.9238795325112869605, 1.000000000000000000, 0.9238795325112869605, 1.000000000000000000, 0.9238795325112869605, 1.000000000000000000, 0.9238795325112869605, 1.000000000000000000, 0.9238795325112869605, 1.000000000000000000, 0.9238795325112869605, 1.000000000000000000, 0.9238795325112869605, 1.000000000000000000, 0.9238795325112869605, 1.000000000000000000, 0.9238795325112869605, 1.000000000000000000, 0.9238795325112869605, 1.000000000000000000, 0.9238795325112869605, 1.000000000000000000, 0.9238795325112869605, 1.000000000000000000, 0.9238795325112869605, 1.000000000000000000, 0.9238795325112869605, 1.000000000000000000, 0.9238795325112869605, 1.000000000000000000, 0.9238795325112869605, 1.000000000000000000, 0.9238795325112869605, 1.000000000000000000, 0.9238795325112869605, 1.000000000000000000, 0.9238795325112869605, 1.000000000000000000, 0.9238795325112869605, 1.000000000000000000, 0.9238795325112869605, 1.000000000000000000, 0.9238795325112869605, 1.000000000000000000, 0.9238795325112869605, 1.000000000000000000, 0.9238795325112869605, 1.000000000000000000, 0.9238795325112869605, 1.000000000000000000, 0.9238795325112869605, 1.000000000000000000, 0.9238795325112869605, 1.000000000000000000, 0.9238795325112869605, 1.000000000000000000, 0.9238795325112869605, 1.000000000000000000, 0.9238795325112869605, 1.000000000000000000, 0.9238795325112869605, 1.000000000000000000, 0.9238795325112869605, 1.000000000000000000, 0.9238795325112869605, 1.000000000000000000, 0.9238795325112869605, 1.000000000000000000, 0.9238795325112869605, 1.000000000000000000, 0.9238795325112869605, 1.000000000000000000, 0.9238795325112869605, 1.000000000000000000, 0.9238795325112869605, 1.000000000000000000, 0.9238795325112869605, 1.000000000000000000, 0.9238795325112869605, 1.000000000000000000, 0.9238795325112869605, 1.000000000000000000, 0.9238795325112869605, 1.000000000000000000, 0.9238795325112869605, 1.000000000000000000, 0.9238795325112869605, 1.000000000000000000, 0.9238795325112869605, 1.000000000000000000, 0.9238795325112869605, 1.000000000000000000, 0.9238795325112869605, 1.000000000000000000, 0.9238795325112869605, 1.000000000000000000, 0.9238795325112869605, 1.000000000000000000, 0.9238795325112869605, 1.000000000000000000, 0.9238795325112869605, 1.000000000000000000, 0.9238795325112869605, 1.000000000000000000, 0.9238795325112869605, 1.000000000000000000, 0.9238795325112869605, 1.000000000000000000, 0.9238795325112869605, 1.000000000000000000, 0.9238795325112869605, 1.000000000000000000, 0.9238795325112869605, 1.000000000000000000, 0.9238795325112869605, 1.000000000000000000, 0.9238795325112869605, 1.000000000000000000, 0.9238795325112869605, 1.000000000000000000, 0.9238795325112869605, 1.000000000000000000, 0.9238795325112869605, 1.000000000000000000, 0.9238795325112869605, 1.000000000000000000, 0.9238795325112869605, 1.000000000000000000, 0.9238795325112869605, 1.000000000000000000, 0.9238795325112869605, 1.000000000000000000, 0.9238795325112869605, 1.000000000000000000),
 ( 1.000000000000000000, 0.9238795325112869605, 1.000000000000000000, 0.9238795325112869605, 1.000000000000000000, 0.9238795325112869605, 1.000000000000000000, 0.9238795325112869605, 1.000000000000000000, 0.9238795325112869605, 1.000000000000000000, 0.9238795325112869605, 1.000000000000000000, 0.9238795325112869605, 1.000000000000000000, 0.9238795325112869605, 1.000000000000000000, 0.9238795325112869605, 1.000000000000000000, 0.9238795325112869605, 1.000000000000000000, 0.9238795325112869605, 1.000000000000000000, 0.9238795325112869605, 1.000000000000000000, 0.9238795325112869605, 1.000000000000000000, 0.9238795325112869605, 1.000000000000000000, 0.9238795325112869605, 1.000000000000000000, 0.9238795325112869605, 1.000000000000000000, 0.9238795325112869605, 1.000000000000000000, 0.9238795325112869605, 1.000000000000000000, 0.9238795325112869605, 1.000000000000000000, 0.9238795325112869605, 1.000000000000000000, 0.9238795325112869605, 1.000000000000000000, 0.9238795325112869605, 1.000000000000000000, 0.9238795325112869605, 1.000000000000000000, 0.9238795325112869605, 1.000000000000000000, 0.9238795325112869605, 1.000000000000000000, 0.9238795325112869605, 1.000000000000000000, 0.9238795325112869605, 1.000000000000000000, 0.9238795325112869605, 1.000000000000000000, 0.9238795325112869605, 1.000000000000000000, 0.9238795325112869605, 1.000000000000000000, 0.9238795325112869605, 1.000000000000000000, 0.9238795325112869605, 1.000000000000000000, 0.9238795325112869605, 1.000000000000000000, 0.9238795325112869605, 1.000000000000000000, 0.9238795325112869605, 1.000000000000000000, 0.9238795325112869605, 1.000000000000000000, 0.9238795325112869605, 1.000000000000000000, 0.9238795325112869605, 1.000000000000000000, 0.9238795325112869605, 1.000000000000000000, 0.9238795325112869605, 1.000000000000000000, 0.9238795325112869605, 1.000000000000000000, 0.9238795325112869605, 1.000000000000000000, 0.9238795325112869605, 1.000000000000000000, 0.9238795325112869605, 1.000000000000000000, 0.9238795325112869605, 1.000000000000000000, 0.9238795325112869605, 1.000000000000000000, 0.9238795325112869605, 1.000000000000000000, 0.9238795325112869605, 1.000000000000000000, 0.9238795325112869605, 1.000000000000000000, 0.9238795325112869605, 1.000000000000000000, 0.9238795325112869605, 1.000000000000000000, 0.9238795325112869605, 1.000000000000000000, 0.9238795325112869605, 1.000000000000000000, 0.9238795325112869605, 1.000000000000000000, 0.9238795325112869605, 1.000000000000000000, 0.9238795325112869605, 1.000000000000000000, 0.9238795325112869605, 1.000000000000000000, 0.9238795325112869605, 1.000000000000000000, 0.9238795325112869605, 1.000000000000000000, 0.9238795325112869605, 1.000000000000000000, 0.9238795325112869605, 1.000000000000000000, 0.9238795325112869605, 1.000000000000000000, 0.9238795325112869605, 1.000000000000000000, 0.9238795325112869605, 1.000000000000000000, 0.9238795325112869605, 1.000000000000000000, 0.9238795325112869605, 1.000000000000000000, 0.9238795325112869605, 1.000000000000000000, 0.9238795325112869605, 1.000000000000000000, 0.9238795325112869605, 1.000000000000000000, 0.9238795325112869605, 1.000000000000000000, 0.9238795325112869605, 1.000000000000000000, 0.9238795325112869605, 1.000000000000000000, 0.9238795325112869605, 1.000000000000000000, 0.9238795325112869605, 1.000000000000000000, 0.9238795325112869605, 1.000000000000000000, 0.9238795325112869605, 1.000000000000000000, 0.9238795325112869605, 1.000000000000000000, 0.9238795325112869605, 1.000000000000000000, 0.9238795325112869605, 1.000000000000000000, 0.9238795325112869605, 1.000000000000000000, 0.9238795325112869605, 1.000000000000000000, 0.9238795325112869605, 1.000000000000000000, 0.9238795325112869605, 1.000000000000000000, 0.9238795325112869605, 1.000000000000000000, 0.9238795325112869605, 1.000000000000000000, 0.9238795325112869605, 1.000000000000000000, 0.9238795325112869605, 1.000000000000000000, 0.9238795325112869605, 1.000000000000000000, 0.9238795325112869605, 1.000000000000000000, 0.9238795325112869605, 1.000000000000000000, 0.9238795325112869605, 1.000000000000000000, 0.9238795325112869605, 1.000000000000000000, 0.9238795325112869605, 1.000000000000000000, 0.9238795325112869605, 1.000000000000000000, 0.9238795325112869605, 1.000000000000000000, 0.9238795325112869605, 1.000000000000000000, 0.9238795325112869605, 1.000000000000000000, 0.9238795325112869605, 1.000000000000000000, 0.9238795325112869605, 1.000000000000000000, 0.9238795325112869605, 1.000000000000000000, 0.9238795325112869605, 1.000000000000000000, 0.9238795325112869605, 1.000000000000000000, 0.9238795325112869605, 1.000000000000000000, 0.9238795325112869605, 1.000000000000000000, 0.9238795325112869605, 1.000000000000000000, 0.9238795325112869605, 1.000000000000000000, 0.9238795325112869605, 1.000000000000000000, 0.9238795325112869605, 1.000000000000000000, 0.9238795325112869605, 1.000000000000000000, 0.9238795325112869605, 1.000000000000000000, 0.9238795325112869605, 1.000000000000000000, 0.9238795325112869605, 1.000000000000000000, 0.9238795325112869605, 1.000000000000000000, 0.9238795325112869605, 1.000000000000000000, 0.9238795325112869605, 1.000000000000000000, 0.9238795325112869605, 1.000000000000000000, 0.9238795325112869605, 1.000000000000000000, 0.9238795325112869605, 1.000000000000000000, 0.9238795325112869605, 1.000000000000000000, 0.9238795325112869605, 1.000000000000000000, 0.9238795325112869605, 1.000000000000000000, 0.9238795325112869605, 1.000000000000000000, 0.9238795325112869605, 1.000000000000000000, 0.9238795325112869605, 1.000000000000000000, 0.9238795325112869605, 1.000000000000000000, 0.9238795325112869605, 1.000000000000000000, 0.9238795325112869605, 1.000000000000000000, 0.9238795325112869605, 1.000000000000000000) ) ) 
 REPRESENTATION_ITEM ( '' )  SURFACE ( )  );
#6330 = CARTESIAN_POINT ( 'NONE',  ( 123.2906948109119867, -8.166667518702819706, -8.995218007635861213 ) ) ;
#6331 = CARTESIAN_POINT ( 'NONE',  ( 110.7603796295247918, -4.863998795839590272, -19.15521520033831493 ) ) ;
#6332 = DIRECTION ( 'NONE',  ( 0.000000000000000000, 0.000000000000000000, -1.000000000000000000 ) ) ;
#6333 = CARTESIAN_POINT ( 'NONE',  ( 124.9235546484006250, -12.43496779199546687, -14.50182173845576727 ) ) ;
#6334 = CARTESIAN_POINT ( 'NONE',  ( 115.6893214775786447, -9.859900752359374465, -12.68260735090039404 ) ) ;
#6335 = CARTESIAN_POINT ( 'NONE',  ( 116.1998614775786507, 0.4262465694468514643, -12.03445270309931736 ) ) ;
#6336 = CARTESIAN_POINT ( 'NONE',  ( 84.49707967414211396, -25.99489077589524300, -13.39321520033831625 ) ) ;
#6337 = CIRCLE ( 'NONE', #44918, 1.499999999999996225 ) ;
#6338 = CARTESIAN_POINT ( 'NONE',  ( 112.2883483795247770, -8.402594152722688392, -16.93181055722141792 ) ) ;
#6339 = B_SPLINE_CURVE_WITH_KNOTS ( 'NONE', 3,
 ( #16066, #11975, #29520, #12200, #19030, #8326, #32917, #9229, #12658, #8768 ),
 .UNSPECIFIED., .F., .F.,
 ( 4, 3, 3, 4 ),
 ( 0.000000000000000000, 0.0001671877548681280042, 0.0003343755096277700343, 0.0006463528481650609656 ),
 .UNSPECIFIED. ) ;
#6340 = ORIENTED_EDGE ( 'NONE', *, *, #30362, .F. ) ;
#6341 = DIRECTION ( 'NONE',  ( 0.000000000000000000, 0.000000000000000000, -1.000000000000000000 ) ) ;
#6342 = CARTESIAN_POINT ( 'NONE',  ( 113.4202548109119846, -10.30919188438810075, -12.61870101168855918 ) ) ;
#6343 = CARTESIAN_POINT ( 'NONE',  ( 79.61425486644590421, 5.119637120372100725, -6.626096235795095879 ) ) ;
#6344 = CARTESIAN_POINT ( 'NONE',  ( 122.2437673109119629, -9.289237151508434209, -11.05642687123711276 ) ) ;
#6345 = ADVANCED_BREP_SHAPE_REPRESENTATION ( '', ( #21657, #12375 ), #32226 ) ;
#6346 = CARTESIAN_POINT ( 'NONE',  ( 119.5350954359119839, 0.5291689781388270175, -13.89700978578772705 ) ) ;
#6347 = ORIENTED_EDGE ( 'NONE', *, *, #38682, .F. ) ;
#6348 = CARTESIAN_POINT ( 'NONE',  ( 123.5508514527377315, -3.041208495916663423, -14.57149963527472103 ) ) ;
#6349 = CARTESIAN_POINT ( 'NONE',  ( 111.5005945643030856, -1.275047081438759111, -16.92345106201108251 ) ) ;
#6350 = ADVANCED_FACE ( 'NONE', ( #6769 ), #12464, .T. ) ;
#6351 = CIRCLE ( 'NONE', #44927, 2.000000000000000444 ) ;
#6352 = ORIENTED_EDGE ( 'NONE', *, *, #32499, .F. ) ;
#6353 = CARTESIAN_POINT ( 'NONE',  ( 118.7525614775786380, -8.166667518702819706, -8.995218007635861213 ) ) ;
#6354 = CARTESIAN_POINT ( 'NONE',  ( 114.0442481442453300, -1.834011780172310813, -8.268836392978581529 ) ) ;
#6355 = CARTESIAN_POINT ( 'NONE',  ( 118.6958348109119754, -3.505236298600246325, -18.68346056562440793 ) ) ;
#6356 = CARTESIAN_POINT ( 'NONE',  ( 120.2513128976245724, -8.245411914654436458, -17.07692946740144180 ) ) ;
#6357 = CARTESIAN_POINT ( 'NONE',  ( 123.2339681442453241, -6.344957434206665248, -7.627207830600338134 ) ) ;
#6358 = ADVANCED_FACE ( 'NONE', ( #43274 ), #24545, .T. ) ;
#6359 = CARTESIAN_POINT ( 'NONE',  ( 117.2209414775786485, -7.893985811506177619, -18.51759400769804742 ) ) ;
#6360 = EDGE_CURVE ( 'NONE', #15954, #32359, #26166, .T. ) ;
#6361 = CARTESIAN_POINT ( 'NONE',  ( 106.8710046295248759, -4.863998795839590272, -18.39754474579285315 ) ) ;
#6362 = CARTESIAN_POINT ( 'NONE',  ( 114.5547881442453217, -4.153390946401321671, -8.397313243818183892 ) ) ;
#6363 = DIRECTION ( 'NONE',  ( 0.000000000000000000, -1.000000000000000000, 1.195183497228115774E-16 ) ) ;
#6364 = EDGE_LOOP ( 'NONE', ( #24925, #949, #28706, #7528, #30199 ) ) ;
#6365 = B_SPLINE_CURVE_WITH_KNOTS ( 'NONE', 3,
 ( #20187, #39009, #7780, #6723, #20635, #21687, #3290, #14395, #4347, #28306 ),
 .UNSPECIFIED., .F., .F.,
 ( 4, 3, 3, 4 ),
 ( 0.000000000000000000, 0.0001671877548681309858, 0.0003343755096277739917, 0.0006463528481650629171 ),
 .UNSPECIFIED. ) ;
#6366 = CARTESIAN_POINT ( 'NONE',  ( 119.2063748109119814, -1.561330072975668504, -17.79121239304076951 ) ) ;
#6367 = DIRECTION ( 'NONE',  ( -1.000000000000000000, 0.000000000000000000, 0.000000000000000000 ) ) ;
#6368 = CARTESIAN_POINT ( 'NONE',  ( 114.4980614775786592, -7.893985811506177619, -18.51759400769804742 ) ) ;
#6369 = EDGE_LOOP ( 'NONE', ( #33977, #18603, #8506, #6643 ) ) ;
#6370 = CARTESIAN_POINT ( 'NONE',  ( 122.1561614775786353, -0.4660016031367893996, -10.09054647747474043 ) ) ;
#6372 = DIRECTION ( 'NONE',  ( -1.000000000000000000, 0.000000000000000000, 0.000000000000000000 ) ) ;
#6371 = AXIS2_PLACEMENT_3D ( 'NONE', #36394, #43260, #25707 ) ;
#6373 = DIRECTION ( 'NONE',  ( 1.000000000000000000, 0.000000000000000000, 0.000000000000000000 ) ) ;
#6374 = ADVANCED_FACE ( 'NONE', ( #8391 ), #40071, .F. ) ;
#6375 = CARTESIAN_POINT ( 'NONE',  ( 93.24708369096698846, -24.14644159042263993, -12.62951656296512937 ) ) ;
#6376 = CARTESIAN_POINT ( 'NONE',  ( 115.8595014775786609, -7.643976991954077427, -18.09477374809248928 ) ) ;
#6377 = EDGE_CURVE ( 'NONE', #2745, #2517, #30035, .T. ) ;
#6378 = EDGE_CURVE ( 'NONE', #7925, #23072, #37240, .T. ) ;
#6379 = CARTESIAN_POINT ( 'NONE',  ( 70.19691569158496236, 3.834886253390165756, -6.893215200338315363 ) ) ;
#6380 = CARTESIAN_POINT ( 'NONE',  ( 117.2776681442452968, -4.153390946401325223, -8.397313243818185668 ) ) ;
#6381 = DIRECTION ( 'NONE',  ( -0.9609149988134837450, 0.1028163501681645109, -0.2570431154366520921 ) ) ;
#6382 = CARTESIAN_POINT ( 'NONE',  ( 116.8805814775786445, -3.505236298600246325, -18.68346056562440793 ) ) ;
#6383 = CARTESIAN_POINT ( 'NONE',  ( 115.0653281442453277, -6.344957434206662583, -7.627207830600332805 ) ) ;
#6384 = CARTESIAN_POINT ( 'NONE',  ( 120.1601735609119856, 0.6414057260225851653, -11.69287257290600657 ) ) ;
#6385 = CARTESIAN_POINT ( 'NONE',  ( 112.4559014775786494, -9.988377603198976828, -10.36322818467138340 ) ) ;
#6386 = CARTESIAN_POINT ( 'NONE',  ( 115.3489614775786407, -0.8288870151387760510, -10.36305467784173118 ) ) ;
#6387 = CARTESIAN_POINT ( 'NONE',  ( 112.0020881442453344, -9.565557343593413364, -10.61323700422348004 ) ) ;
#6388 = AXIS2_PLACEMENT_3D ( 'NONE', #1481, #39573, #42776 ) ;
#6389 = CARTESIAN_POINT ( 'NONE',  ( 115.2355081442453155, 0.1319031606808879209, -14.10382304977623669 ) ) ;
#6390 = ORIENTED_EDGE ( 'NONE', *, *, #41804, .T. ) ;
#6391 = CARTESIAN_POINT ( 'NONE',  ( 113.8740681442453138, 0.5811942927096154232, -14.16772938898807155 ) ) ;
#6392 = CARTESIAN_POINT ( 'NONE',  ( 107.2877233795247776, -8.938348069036489818, -17.46756447353520159 ) ) ;
#6393 = CARTESIAN_POINT ( 'NONE',  ( 107.8433483795247838, -8.402594152722688392, -16.93181055722141792 ) ) ;
#6394 = CARTESIAN_POINT ( 'NONE',  ( 106.8015515045248378, -6.936859964151250502, -18.39754474579286025 ) ) ;
#6395 = B_SPLINE_CURVE_WITH_KNOTS ( 'NONE', 3,
 ( #23092, #26286, #22860, #12615, #36752, #5521, #19441, #33324, #2098, #29933 ),
 .UNSPECIFIED., .F., .F.,
 ( 4, 3, 3, 4 ),
 ( 0.000000000000000000, 0.0001671877560958114864, 0.0003343755126086574896, 0.0006438490228507209303 ),
 .UNSPECIFIED. ) ;
#6396 = DIRECTION ( 'NONE',  ( 0.000000000000000000, -0.9242245927363029745, -0.3818493186865927758 ) ) ;
#6397 = CARTESIAN_POINT ( 'NONE',  ( 118.6958348109119754, -6.344957434206665248, -7.627207830600338134 ) ) ;
#6398 = ORIENTED_EDGE ( 'NONE', *, *, #11163, .T. ) ;
#6399 = CARTESIAN_POINT ( 'NONE',  ( 125.5597614775786326, -1.561330072975669392, -17.79121239304076951 ) ) ;
#6400 = CARTESIAN_POINT ( 'NONE',  ( 125.1059481442452750, -8.166667518702794837, -8.995218007635845225 ) ) ;
#6401 = CARTESIAN_POINT ( 'NONE',  ( 116.8805814775786445, -3.505236298600246325, -18.68346056562440793 ) ) ;
#6402 = CARTESIAN_POINT ( 'NONE',  ( 124.5386814775786206, -4.153390946401287032, -8.397313243818187445 ) ) ;
#6403 = CARTESIAN_POINT ( 'NONE',  ( 124.9924948109119924, -4.089484607189486809, -7.948022111789456723 ) ) ;
#6404 = CARTESIAN_POINT ( 'NONE',  ( 115.4831921295247952, -9.868328341294093420, -13.39321520033831447 ) ) ;
#6405 = CARTESIAN_POINT ( 'NONE',  ( 124.1497896737536877, -8.611453504372539314, -17.77011218421760574 ) ) ;
#6406 = ORIENTED_EDGE ( 'NONE', *, *, #13986, .F. ) ;
#6407 = CARTESIAN_POINT ( 'NONE',  ( 111.9261565460471957, -2.191907684172563986, -18.20049396185734025 ) ) ;
#6408 = CARTESIAN_POINT ( 'NONE',  ( 123.2339681442453241, -3.505236298600246325, -18.68346056562440793 ) ) ;
#6409 = CARTESIAN_POINT ( 'NONE',  ( 118.2987481442453088, -1.561330072975668504, -17.79121239304076951 ) ) ;
#6410 = AXIS2_PLACEMENT_3D ( 'NONE', #19499, #29080, #2149 ) ;
#6411 = CARTESIAN_POINT ( 'NONE',  ( 117.9016614775786280, -0.1624402480850797581, -16.17319339645315424 ) ) ;
#6412 = CARTESIAN_POINT ( 'NONE',  ( 117.9583881442453048, -10.30919188438810075, -12.61870101168855918 ) ) ;
#6413 = CARTESIAN_POINT ( 'NONE',  ( 123.4041481442452834, 0.1319031606808844515, -14.10382304977626511 ) ) ;
#6414 = CARTESIAN_POINT ( 'NONE',  ( 126.4536383592487141, -1.145462627196077721, -9.876933969119310319 ) ) ;
#6415 = CARTESIAN_POINT ( 'NONE',  ( 124.1983214775786166, -1.833838273342659697, -17.42832698103878286 ) ) ;
#6416 = ORIENTED_EDGE ( 'NONE', *, *, #10709, .T. ) ;
#6417 = EDGE_CURVE ( 'NONE', #2957, #29689, #31818, .T. ) ;
#6418 = CARTESIAN_POINT ( 'NONE',  ( 123.9106423109119675, -9.959231468620755479, -10.70263013195267199 ) ) ;
#6419 = CARTESIAN_POINT ( 'NONE',  ( 115.3489614775786407, -9.261995988541697145, -16.69588392320189030 ) ) ;
#6420 = CARTESIAN_POINT ( 'NONE',  ( 121.1350814775786233, -9.859900752359378018, -12.68260735090039759 ) ) ;
#6421 = ORIENTED_EDGE ( 'NONE', *, *, #15843, .F. ) ;
#6422 = CARTESIAN_POINT ( 'NONE',  ( 123.9106423109119675, -0.4387604401700512802, -15.73000352943951619 ) ) ;
#6423 = EDGE_CURVE ( 'NONE', #14508, #6975, #44186, .T. ) ;
#6424 = CARTESIAN_POINT ( 'NONE',  ( 137.2618751061050375, -0.2068468655711039328, -10.95876972476207989 ) ) ;
#6425 = CARTESIAN_POINT ( 'NONE',  ( 119.7169148109119874, -9.988377603198976828, -10.36322818467138340 ) ) ;
#6426 = CARTESIAN_POINT ( 'NONE',  ( 113.6079577545248043, -7.250697342233347165, -7.631215200338321125 ) ) ;
#6427 = CARTESIAN_POINT ( 'NONE',  ( 120.2274548109119934, -9.859900752359374465, -12.68260735090039404 ) ) ;
#6428 = ORIENTED_EDGE ( 'NONE', *, *, #3317, .F. ) ;
#6429 = ORIENTED_EDGE ( 'NONE', *, *, #9761, .F. ) ;
#6430 = CARTESIAN_POINT ( 'NONE',  ( 126.4106614775786284, -6.222761293078241884, -8.102969835052219238 ) ) ;
#6431 = CARTESIAN_POINT ( 'NONE',  ( 124.4819548109119722, -2.084020599724406786, -8.691656652584148546 ) ) ;
#6432 = CARTESIAN_POINT ( 'NONE',  ( 69.36136150295220659, -53.48028990332819177, -31.49013104333824131 ) ) ;
#6433 = EDGE_CURVE ( 'NONE', #5950, #38773, #2660, .T. ) ;
#6434 = ORIENTED_EDGE ( 'NONE', *, *, #36836, .T. ) ;
#6435 = CARTESIAN_POINT ( 'NONE',  ( 120.3409081442453044, -0.4660016031367893996, -10.09054647747474043 ) ) ;
#6436 = CARTESIAN_POINT ( 'NONE',  ( 119.7434548109119703, -12.48189245497263755, -10.95032834292243074 ) ) ;
#6437 = EDGE_CURVE ( 'NONE', #12130, #41268, #23659, .T. ) ;
#6438 = AXIS2_PLACEMENT_3D ( 'NONE', #41953, #35762, #10718 ) ;
#6439 = DIRECTION ( 'NONE',  ( -1.000000000000000000, 0.000000000000000000, 0.000000000000000000 ) ) ;
#6440 = CARTESIAN_POINT ( 'NONE',  ( 120.7947214775786193, -9.261995988541697145, -16.69588392320189030 ) ) ;
#6442 = CARTESIAN_POINT ( 'NONE',  ( 120.0572748109119772, -6.222761293078241884, -8.102969835052219238 ) ) ;
#6441 = CARTESIAN_POINT ( 'NONE',  ( 117.1642148109119859, -9.261995988541697145, -16.69588392320189030 ) ) ;
#6443 = EDGE_CURVE ( 'NONE', #20552, #13839, #37478, .T. ) ;
#6444 = CARTESIAN_POINT ( 'NONE',  ( 125.5030348109119558, -6.222761293078241884, -8.102969835052219238 ) ) ;
#6445 = CARTESIAN_POINT ( 'NONE',  ( 112.3991748109119868, -8.166667518702817929, -8.995218007635859436 ) ) ;
#6446 = ORIENTED_EDGE ( 'NONE', *, *, #26323, .F. ) ;
#6447 = CARTESIAN_POINT ( 'NONE',  ( 122.3830681442452857, -1.833838273342659697, -17.42832698103878286 ) ) ;
#6448 = LINE ( 'NONE', #10319, #43137 ) ;
#6449 = CARTESIAN_POINT ( 'NONE',  ( 108.5378796295247810, -4.863998795839590272, -19.15521520033831493 ) ) ;
#6450 = CARTESIAN_POINT ( 'NONE',  ( 112.4272546295247821, -4.863998795839590272, -18.39754474579285315 ) ) ;
#6451 = CARTESIAN_POINT ( 'NONE',  ( 109.3018640045248304, -10.62599879583958717, -11.00651665394454604 ) ) ;
#6452 = CARTESIAN_POINT ( 'NONE',  ( 122.8368814775786291, -1.561330072975668948, -17.79121239304076951 ) ) ;
#6453 = CARTESIAN_POINT ( 'NONE',  ( 122.8936081442453059, -9.565557343593413364, -10.61323700422348004 ) ) ;
#6454 = VERTEX_POINT ( 'NONE', #34779 ) ;
#6455 = CARTESIAN_POINT ( 'NONE',  ( 122.8936081442453059, 0.2603800115204892296, -16.42320221600525088 ) ) ;
#6456 = CARTESIAN_POINT ( 'NONE',  ( 63.69189222814998175, -69.76310523276724496, -16.89321520033831447 ) ) ;
#6457 = CARTESIAN_POINT ( 'NONE',  ( 125.3328548109119964, -9.261995988541697145, -16.69588392320189030 ) ) ;
#6458 = CARTESIAN_POINT ( 'NONE',  ( 121.7590748109119687, -7.893985811506177619, -18.51759400769804742 ) ) ;
#6459 = CARTESIAN_POINT ( 'NONE',  ( 119.2572829359120021, -5.367793381288652910, -18.78638297431638904 ) ) ;
#6460 = CARTESIAN_POINT ( 'NONE',  ( 112.1722681442453222, -0.4660016031367893996, -10.09054647747474043 ) ) ;
#6461 = DIRECTION ( 'NONE',  ( 1.000000000000000000, 0.000000000000000000, 0.000000000000000000 ) ) ;
#6462 = CARTESIAN_POINT ( 'NONE',  ( 107.6349890045248401, 0.8980012041604421569, -15.77991374673208469 ) ) ;
#6463 = ORIENTED_EDGE ( 'NONE', *, *, #26706, .T. ) ;
#6464 = CARTESIAN_POINT ( 'NONE',  ( 124.9401836525450022, -2.378957183258596064, -17.95140958770220863 ) ) ;
#6465 = CARTESIAN_POINT ( 'NONE',  ( 118.6557253070358939, -1.196538596002800103, -17.02799684832027083 ) ) ;
#6466 = CARTESIAN_POINT ( 'NONE',  ( 123.0070614775786169, -10.15424416112533912, -14.75197769757731336 ) ) ;
#6467 = CARTESIAN_POINT ( 'NONE',  ( 108.4684265045247997, -2.791137627527939813, -8.388885654883777576 ) ) ;
#6468 = CARTESIAN_POINT ( 'NONE',  ( 107.0793640045248196, 0.1403307496149616695, -15.46607636864997204 ) ) ;
#6469 = CARTESIAN_POINT ( 'NONE',  ( 122.9503348109119827, -9.859900752359378018, -12.68260735090039759 ) ) ;
#6470 = CARTESIAN_POINT ( 'NONE',  ( 115.7460481442453357, -10.15424416112533912, -14.75197769757731336 ) ) ;
#6471 = CARTESIAN_POINT ( 'NONE',  ( 123.9146881442452894, 0.9020085738987339008, -11.91225656197089222 ) ) ;
#6472 = ORIENTED_EDGE ( 'NONE', *, *, #18619, .T. ) ;
#6473 = CARTESIAN_POINT ( 'NONE',  ( 123.2906948109119867, -1.833838273342659697, -17.42832698103878286 ) ) ;
#6474 = CARTESIAN_POINT ( 'NONE',  ( 118.3554748109119998, 0.2603800115204892296, -16.42320221600525088 ) ) ;
#6475 = DIRECTION ( 'NONE',  ( 1.000000000000000000, 0.000000000000000000, -0.000000000000000000 ) ) ;
#6476 = ORIENTED_EDGE ( 'NONE', *, *, #25847, .F. ) ;
#6477 = DIRECTION ( 'NONE',  ( 1.000000000000000000, 0.000000000000000000, 0.000000000000000000 ) ) ;
#6478 = ADVANCED_FACE ( 'NONE', ( #20906 ), #37660, .T. ) ;
#6479 = ORIENTED_EDGE ( 'NONE', *, *, #14761, .T. ) ;
#6480 = CARTESIAN_POINT ( 'NONE',  ( 113.6471614775786492, -4.153390946401321671, -8.397313243818183892 ) ) ;
#6481 = CARTESIAN_POINT ( 'NONE',  ( 113.9307948109119764, -10.15424416112533912, -14.75197769757731336 ) ) ;
#6482 = CARTESIAN_POINT ( 'NONE',  ( 115.1010702440515558, -2.467220198592777525, -17.83387418641524391 ) ) ;
#6483 = CARTESIAN_POINT ( 'NONE',  ( 119.7434548109119703, -7.554583864224885481, -18.48844787311982785 ) ) ;
#6484 = ORIENTED_EDGE ( 'NONE', *, *, #26163, .F. ) ;
#6485 = DIRECTION ( 'NONE',  ( 0.000000000000000000, 0.9242245927363027524, 0.3818493186865928868 ) ) ;
#6486 = CARTESIAN_POINT ( 'NONE',  ( 125.0849378844212367, 2.528548847979777303, -12.18453881567924135 ) ) ;
#6487 = CARTESIAN_POINT ( 'NONE',  ( 115.2748327545248657, -2.477300249445798297, -19.15521520033831138 ) ) ;
#6488 = ADVANCED_FACE ( 'NONE', ( #42323 ), #28640, .T. ) ;
#6489 = CARTESIAN_POINT ( 'NONE',  ( 115.8304577545247582, -2.791137627527887410, -18.39754474579284249 ) ) ;
#6490 = CARTESIAN_POINT ( 'NONE',  ( 121.7023481442452919, -0.8288870151387760510, -10.36305467784173118 ) ) ;
#6491 = CARTESIAN_POINT ( 'NONE',  ( 113.9307948109119764, -10.15424416112533912, -14.75197769757731336 ) ) ;
#6492 = CARTESIAN_POINT ( 'NONE',  ( 126.2450673757166442, -5.764848433121719573, -18.32501366739699122 ) ) ;
#6493 = ORIENTED_EDGE ( 'NONE', *, *, #18626, .T. ) ;
#6494 = CARTESIAN_POINT ( 'NONE',  ( 124.8790414775786246, -8.899110576539426276, -16.42337572283528146 ) ) ;
#6495 = CARTESIAN_POINT ( 'NONE',  ( 116.2665301496069929, 0.3591747506842615789, -14.64321520033831447 ) ) ;
#6496 = CARTESIAN_POINT ( 'NONE',  ( 112.4967077545247633, -7.250697342233347165, -7.631215200338321125 ) ) ;
#6497 = FACE_BOUND ( 'NONE', #35843, .T. ) ;
#6499 = LINE ( 'NONE', #27926, #40747 ) ;
#6498 = CARTESIAN_POINT ( 'NONE',  ( 65.89554156778412164, -36.79628389010467515, -5.218367175095595556 ) ) ;
#6500 = CARTESIAN_POINT ( 'NONE',  ( 126.1270281442452870, 0.1319031606808879209, -14.10382304977623669 ) ) ;
#6501 = EDGE_LOOP ( 'NONE', ( #44323, #42058, #33960, #33933, #13218 ) ) ;
#6502 = CARTESIAN_POINT ( 'NONE',  ( 114.2711548109119803, -9.988377603198976828, -10.36322818467138340 ) ) ;
#6503 = AXIS2_PLACEMENT_3D ( 'NONE', #30220, #34079, #40945 ) ;
#6504 = PLANE ( 'NONE',  #686 ) ;
#6505 = CARTESIAN_POINT ( 'NONE',  ( 114.4413952545248350, 0.8980012041604421569, -11.00651665394454071 ) ) ;
#6506 = CARTESIAN_POINT ( 'NONE',  ( 125.3895814775786448, -2.084020599724406786, -8.691656652584148546 ) ) ;
#6507 = CARTESIAN_POINT ( 'NONE',  ( 123.5176014775786228, -0.8288870151387760510, -10.36305467784173118 ) ) ;
#6508 = CARTESIAN_POINT ( 'NONE',  ( 125.4584548109119737, -1.575707845324203493, -20.23615509330177531 ) ) ;
#6509 = CARTESIAN_POINT ( 'NONE',  ( 113.8857702545248003, 0.1403307496149616695, -11.32035403202665336 ) ) ;
#6510 = CARTESIAN_POINT ( 'NONE',  ( 70.19189222814998175, -70.34019061884472990, -41.33884020749756871 ) ) ;
#6511 = DIRECTION ( 'NONE',  ( 1.000000000000000000, 0.000000000000000000, -0.000000000000000000 ) ) ;
#6512 = CARTESIAN_POINT ( 'NONE',  ( 112.9664414775786412, -9.859900752359374465, -12.68260735090039404 ) ) ;
#6513 = CARTESIAN_POINT ( 'NONE',  ( 105.4819421295248247, 0.8980012041604618078, -13.39321520033831447 ) ) ;
#6514 = DIRECTION ( 'NONE',  ( 1.000000000000000000, 0.000000000000000000, 0.000000000000000000 ) ) ;
#6515 = CARTESIAN_POINT ( 'NONE',  ( 115.2748327545248657, -2.477300249445798297, -19.15521520033831138 ) ) ;
#6516 = CARTESIAN_POINT ( 'NONE',  ( 123.7445081442452874, -1.561330072975668948, -17.79121239304076951 ) ) ;
#6517 = CARTESIAN_POINT ( 'NONE',  ( 125.2194014775786286, -10.30919188438810075, -12.61870101168855918 ) ) ;
#6518 = DIRECTION ( 'NONE',  ( -0.2588190451025185190, 0.9659258262890689783, 0.000000000000000000 ) ) ;
#6519 = CARTESIAN_POINT ( 'NONE',  ( 120.5110881442453206, -6.344957434206665248, -7.627207830600338134 ) ) ;
#6520 = CARTESIAN_POINT ( 'NONE',  ( 112.3424481442453384, -6.344957434206662583, -7.627207830600332805 ) ) ;
#6521 = ORIENTED_EDGE ( 'NONE', *, *, #32029, .F. ) ;
#6522 = CARTESIAN_POINT ( 'NONE',  ( 114.0442481442453300, -7.643976991954077427, -18.09477374809248928 ) ) ;
#6523 = CARTESIAN_POINT ( 'NONE',  ( 124.9924948109119924, -4.089484607189486809, -7.948022111789456723 ) ) ;
#6524 = CARTESIAN_POINT ( 'NONE',  ( 122.8936081442453059, 0.2603800115204892296, -16.42320221600525088 ) ) ;
#6525 = CARTESIAN_POINT ( 'NONE',  ( 114.9518748109119883, -1.834011780172310813, -8.268836392978581529 ) ) ;
#6526 = CARTESIAN_POINT ( 'NONE',  ( 113.2500748109119968, -3.505236298600246325, -18.68346056562440793 ) ) ;
#6527 = ORIENTED_EDGE ( 'NONE', *, *, #34763, .F. ) ;
#6528 = CARTESIAN_POINT ( 'NONE',  ( 118.7525614775786380, -1.833838273342659253, -17.42832698103878286 ) ) ;
#6529 = CARTESIAN_POINT ( 'NONE',  ( 61.69189222814998175, -40.21211973637273474, -23.89321520033831803 ) ) ;
#6530 = CARTESIAN_POINT ( 'NONE',  ( 125.1626748109119802, -0.1624402480850797581, -16.17319339645315424 ) ) ;
#6531 = DIRECTION ( 'NONE',  ( -0.000000000000000000, -0.9284778069183721172, -0.3713878862591650232 ) ) ;
#6532 = CARTESIAN_POINT ( 'NONE',  ( 111.5938171295247940, -10.62599879583958540, -13.39321520033831447 ) ) ;
#6533 = EDGE_LOOP ( 'NONE', ( #13112, #18857 ) ) ;
#6534 = VECTOR ( 'NONE', #4526, 1000.000000000000114 ) ;
#6535 = CYLINDRICAL_SURFACE ( 'NONE', #15506, 3.000000000000001776 ) ;
#6536 = CARTESIAN_POINT ( 'NONE',  ( 126.0135748109119902, -8.166667518702819706, -8.995218007635861213 ) ) ;
#6537 = CARTESIAN_POINT ( 'NONE',  ( 116.3860827545247787, -6.936859964151250502, -8.388885654883777576 ) ) ;
#6538 = PLANE ( 'NONE',  #36177 ) ;
#6539 = ADVANCED_FACE ( 'NONE', ( #4228 ), #3562, .T. ) ;
#6540 = CIRCLE ( 'NONE', #25486, 1.610000000000000986 ) ;
#6541 = CARTESIAN_POINT ( 'NONE',  ( 116.8098156552294000, 1.991649196448622039, -5.874233632703256269 ) ) ;
#6542 = CARTESIAN_POINT ( 'NONE',  ( 121.7455514173871194, -8.493878760966627084, -17.54745775818410536 ) ) ;
#6543 = CARTESIAN_POINT ( 'NONE',  ( 105.5513952545248060, -9.868328341294098749, -15.46607636864997204 ) ) ;
#6544 = CARTESIAN_POINT ( 'NONE',  ( 111.4073959279789960, 0.1843591316377651834, -14.64321520033828783 ) ) ;
#6545 = CARTESIAN_POINT ( 'NONE',  ( 116.8805814775786445, -6.344957434206662583, -7.627207830600332805 ) ) ;
#6546 = CARTESIAN_POINT ( 'NONE',  ( 137.4783527756549972, -5.189670303016769459, -18.42458730202076467 ) ) ;
#6547 = DIRECTION ( 'NONE',  ( 0.000000000000000000, 0.000000000000000000, 1.000000000000000000 ) ) ;
#6548 = CARTESIAN_POINT ( 'NONE',  ( 119.0361948109119794, -7.893985811506194494, -18.51759400769804031 ) ) ;
#6549 = CARTESIAN_POINT ( 'NONE',  ( 119.6034614775786196, -3.505236298600246325, -18.68346056562440793 ) ) ;
#6550 = ORIENTED_EDGE ( 'NONE', *, *, #3028, .T. ) ;
#6551 = DIRECTION ( 'NONE',  ( -0.2768435750659360983, -0.3568721902840809590, 0.8921882507333046552 ) ) ;
#6552 = CARTESIAN_POINT ( 'NONE',  ( 117.7314814775786260, -4.089484607189486809, -7.948022111789456723 ) ) ;
#6553 = DIRECTION ( 'NONE',  ( 1.000000000000000000, 0.000000000000000000, -0.000000000000000000 ) ) ;
#6554 = CARTESIAN_POINT ( 'NONE',  ( 113.9307948109119764, -10.15424416112533912, -14.75197769757731336 ) ) ;
#6555 = CARTESIAN_POINT ( 'NONE',  ( 111.5482748109120053, -0.1624402480850797581, -16.17319339645315424 ) ) ;
#6556 = CARTESIAN_POINT ( 'NONE',  ( 112.7050671295247923, -10.62599879583958540, -13.39321520033831447 ) ) ;
#6557 = CYLINDRICAL_SURFACE ( 'NONE', #11118, 6.999999999999999112 ) ;
#6558 = CARTESIAN_POINT ( 'NONE',  ( 115.5526452545247622, 0.8980012041604421569, -11.00651665394454071 ) ) ;
#6559 = CARTESIAN_POINT ( 'NONE',  ( 116.7671281442453335, -7.643976991954077427, -18.09477374809248928 ) ) ;
#6560 = CARTESIAN_POINT ( 'NONE',  ( 119.2063748109119814, -7.894159318335828068, -9.358103419637847864 ) ) ;
#6561 = CARTESIAN_POINT ( 'NONE',  ( 111.5497331777918788, -0.01829820670803256055, -14.64321520033831447 ) ) ;
#6562 = DIRECTION ( 'NONE',  ( 1.000000000000000000, 0.000000000000000000, -0.000000000000000000 ) ) ;
#6563 = B_SPLINE_CURVE_WITH_KNOTS ( 'NONE', 3,
 ( #2802, #3032, #13752, #26758, #44770, #20596, #40667, #44540, #27437, #44993 ),
 .UNSPECIFIED., .F., .F.,
 ( 4, 3, 3, 4 ),
 ( 0.000000000000000000, 0.0001671877560958075020, 0.0003343755126086529902, 0.0006438490228507220145 ),
 .UNSPECIFIED. ) ;
#6564 = CARTESIAN_POINT ( 'NONE',  ( 108.1906140045248037, 0.1403307496149616695, -15.46607636864997204 ) ) ;
#6565 = ORIENTED_EDGE ( 'NONE', *, *, #28729, .F. ) ;
#6566 = DIRECTION ( 'NONE',  ( 0.9609149988134837450, -0.1028163501681639419, 0.2570431154366518145 ) ) ;
#6567 = CARTESIAN_POINT ( 'NONE',  ( 115.2922348109119781, -10.63000616557722466, -14.87417383870573495 ) ) ;
#6568 = CARTESIAN_POINT ( 'NONE',  ( 79.48253577138170556, 5.079490123878041885, -6.428895771584159924 ) ) ;
#6569 = DIRECTION ( 'NONE',  ( 1.000000000000000000, 0.000000000000000000, -0.000000000000000000 ) ) ;
#6570 = CARTESIAN_POINT ( 'NONE',  ( 120.9241579359119925, -4.360204210389833968, -8.000047426360245240 ) ) ;
#6571 = ORIENTED_EDGE ( 'NONE', *, *, #17851, .F. ) ;
#6572 = CARTESIAN_POINT ( 'NONE',  ( 123.4699442700021308, -2.835955651089761442, -14.84486572726433806 ) ) ;
#6573 = ORIENTED_EDGE ( 'NONE', *, *, #6437, .F. ) ;
#6574 = CARTESIAN_POINT ( 'NONE',  ( 123.7445081442452874, -1.561330072975668948, -17.79121239304076951 ) ) ;
#6575 = AXIS2_PLACEMENT_3D ( 'NONE', #39139, #18620, #32064 ) ;
#6576 = CARTESIAN_POINT ( 'NONE',  ( 112.7962614775786676, -3.383040157471821630, -19.15922257007629170 ) ) ;
#6577 = CARTESIAN_POINT ( 'NONE',  ( 119.0929214775786278, -4.153390946401325223, -8.397313243818185668 ) ) ;
#6578 = VECTOR ( 'NONE', #25550, 1000.000000000000000 ) ;
#6579 = DIRECTION ( 'NONE',  ( 0.000000000000000000, 0.000000000000000000, -1.000000000000000000 ) ) ;
#6580 = CARTESIAN_POINT ( 'NONE',  ( 122.0427081442452817, 0.5811942927096110934, -14.16772938898807510 ) ) ;
#6581 = CARTESIAN_POINT ( 'NONE',  ( 118.6958348109119754, -6.344957434206665248, -7.627207830600338134 ) ) ;
#6582 = CARTESIAN_POINT ( 'NONE',  ( 116.1082702545247827, -10.62599879583958717, -15.77991374673208469 ) ) ;
#6583 = CARTESIAN_POINT ( 'NONE',  ( 114.1577014775786552, -3.505236298600246325, -18.68346056562440793 ) ) ;
#6584 = PLANE ( 'NONE',  #14084 ) ;
#6585 = ORIENTED_EDGE ( 'NONE', *, *, #12294, .F. ) ;
#6586 = CARTESIAN_POINT ( 'NONE',  ( 118.2420214775786320, -3.383040157471821630, -19.15922257007629170 ) ) ;
#6587 = MANIFOLD_SOLID_BREP ( 'NONE', #28685 ) ;
#6588 = CARTESIAN_POINT ( 'NONE',  ( 69.48536631248848039, -66.77523564985355620, -42.98127819198803934 ) ) ;
#6589 = CARTESIAN_POINT ( 'NONE',  ( 114.3278814775786429, -10.30919188438810075, -12.61870101168855918 ) ) ;
#6590 = EDGE_LOOP ( 'NONE', ( #37068, #26186, #4604, #2995 ) ) ;
#6591 = CARTESIAN_POINT ( 'NONE',  ( 123.8579614775786126, 0.5811942927096110934, -14.16772938898807510 ) ) ;
#6592 = VECTOR ( 'NONE', #30057, 1000.000000000000000 ) ;
#6593 = CARTESIAN_POINT ( 'NONE',  ( 94.99177781699742695, -22.63071325833509917, -12.00328368031911630 ) ) ;
#6594 = CARTESIAN_POINT ( 'NONE',  ( 113.9307948109119764, -10.15424416112533912, -14.75197769757731336 ) ) ;
#6595 = CARTESIAN_POINT ( 'NONE',  ( 78.26539945782576524, -58.08196990603463661, -0.6585284536243714015 ) ) ;
#6596 =( BOUNDED_CURVE ( )  B_SPLINE_CURVE ( 3, ( #31668, #39190, #31895, #14806 ),
 .UNSPECIFIED., .F., .T. ) 
 B_SPLINE_CURVE_WITH_KNOTS ( ( 4, 4 ),
 ( 3.141592653589795336, 6.283185307179590673 ),
 .UNSPECIFIED. ) 
 CURVE ( )  GEOMETRIC_REPRESENTATION_ITEM ( )  RATIONAL_B_SPLINE_CURVE ( ( 1.000000000000000000, 0.3333333333333335369, 0.3333333333333335369, 1.000000000000000000 ) ) 
 REPRESENTATION_ITEM ( '' )  );
#6597 = CARTESIAN_POINT ( 'NONE',  ( 115.5191414775786569, -6.222761293078241884, -8.102969835052219238 ) ) ;
#6598 = B_SPLINE_CURVE_WITH_KNOTS ( 'NONE', 3,
 ( #27925, #35403, #28144, #34943, #42502, #11262, #7375, #34729 ),
 .UNSPECIFIED., .F., .F.,
 ( 4, 2, 2, 4 ),
 ( 0.000000000000000000, 0.5000000000000000000, 0.7500000000000000000, 1.000000000000000000 ),
 .UNSPECIFIED. ) ;
#6599 = DIRECTION ( 'NONE',  ( 0.1352586133457953366, 0.9908103287288504424, 0.000000000000000000 ) ) ;
#6600 = CARTESIAN_POINT ( 'NONE',  ( 119.5467348109119712, -5.574606645277164318, -18.38911715685844683 ) ) ;
#6601 = AXIS2_PLACEMENT_3D ( 'NONE', #38403, #28167, #27722 ) ;
#6602 = CARTESIAN_POINT ( 'NONE',  ( 120.8933699480702586, -6.365377317481695663, -18.95617363400926081 ) ) ;
#6603 = CARTESIAN_POINT ( 'NONE',  ( 117.4478481442453131, -9.565557343593413364, -10.61323700422348004 ) ) ;
#6604 = CONICAL_SURFACE ( 'NONE', #30632, 2.000000000000000444, 0.9599310885968830309 ) ;
#6605 = CARTESIAN_POINT ( 'NONE',  ( 121.3408766859119794, -0.06289925094097943703, -9.412459353600674206 ) ) ;
#6606 = CARTESIAN_POINT ( 'NONE',  ( 115.4624148109119943, -5.638512984488999180, -18.83840828888717311 ) ) ;
#6607 = CARTESIAN_POINT ( 'NONE',  ( 113.5904348109119866, -2.084020599724406786, -8.691656652584148546 ) ) ;
#6608 = CARTESIAN_POINT ( 'NONE',  ( 118.5256548109119876, -8.899110576539710493, -16.42337572283490132 ) ) ;
#6609 = ORIENTED_EDGE ( 'NONE', *, *, #44531, .T. ) ;
#6610 = CARTESIAN_POINT ( 'NONE',  ( 114.8951481442453115, -0.4660016031367893996, -10.09054647747474043 ) ) ;
#6611 = EDGE_CURVE ( 'NONE', #13382, #44494, #32532, .T. ) ;
#6612 = CARTESIAN_POINT ( 'NONE',  ( 106.3848327545248651, -2.477300249445798297, -19.15521520033831138 ) ) ;
#6613 = DIRECTION ( 'NONE',  ( 0.000000000000000000, 0.9284778069183717841, 0.3713878862591654673 ) ) ;
#6614 = CARTESIAN_POINT ( 'NONE',  ( 110.8846330289902369, -1.498564202500827669, -16.62580459685196743 ) ) ;
#6615 = DIRECTION ( 'NONE',  ( -0.9609149988134837450, 0.1028163501681639419, -0.2570431154366518145 ) ) ;
#6616 = CARTESIAN_POINT ( 'NONE',  ( 123.1772414775786189, -4.089484607189486809, -7.948022111789456723 ) ) ;
#6617 = EDGE_LOOP ( 'NONE', ( #16693, #25151 ) ) ;
#6618 = CARTESIAN_POINT ( 'NONE',  ( 60.06931813437629586, -14.72076136720887085, -19.39321520033831447 ) ) ;
#6619 = CARTESIAN_POINT ( 'NONE',  ( 117.6180281442453150, -8.899110576539710493, -16.42337572283490132 ) ) ;
#6620 = CARTESIAN_POINT ( 'NONE',  ( 124.5954081442453116, -6.222761293078269418, -8.102969835052228120 ) ) ;
#6621 = CARTESIAN_POINT ( 'NONE',  ( 121.8725281442453223, -3.383040157471821630, -19.15922257007629170 ) ) ;
#6622 = CARTESIAN_POINT ( 'NONE',  ( 107.0099108795247815, -8.938348069036489818, -9.318865927141430916 ) ) ;
#6623 = CARTESIAN_POINT ( 'NONE',  ( 61.69189222814998175, -40.21211973637273474, -6.893215200338315363 ) ) ;
#6624 = VERTEX_POINT ( 'NONE', #21115 ) ;
#6625 = PLANE ( 'NONE',  #1917 ) ;
#6626 = CARTESIAN_POINT ( 'NONE',  ( 126.5241148109119393, -9.565557343593413364, -10.61323700422348004 ) ) ;
#6627 = CARTESIAN_POINT ( 'NONE',  ( 124.2550481442452792, -9.988377603198980381, -10.36322818467138518 ) ) ;
#6628 = AXIS2_PLACEMENT_3D ( 'NONE', #44419, #23215, #41454 ) ;
#6629 = CARTESIAN_POINT ( 'NONE',  ( 117.5045748109119756, -9.859900752359374465, -12.68260735090039404 ) ) ;
#6630 = CYLINDRICAL_SURFACE ( 'NONE', #41605, 5.999999999999997335 ) ;
#6631 = CARTESIAN_POINT ( 'NONE',  ( 118.2420214775786320, -3.383040157471821630, -19.15922257007629170 ) ) ;
#6632 = EDGE_CURVE ( 'NONE', #40329, #39890, #38361, .T. ) ;
#6633 = FACE_OUTER_BOUND ( 'NONE', #30966, .T. ) ;
#6634 = CARTESIAN_POINT ( 'NONE',  ( 126.9115046738272241, -1.250902631998696668, -9.451862355402859350 ) ) ;
#6635 = CARTESIAN_POINT ( 'NONE',  ( 123.1205148109119563, -7.643976991954077427, -18.09477374809248928 ) ) ;
#6636 = ORIENTED_EDGE ( 'NONE', *, *, #19032, .T. ) ;
#6637 = EDGE_CURVE ( 'NONE', #43185, #21157, #15105, .T. ) ;
#6638 = EDGE_CURVE ( 'NONE', #18337, #22858, #26040, .T. ) ;
#6639 = DIRECTION ( 'NONE',  ( 1.000000000000000000, 0.000000000000000000, -0.000000000000000000 ) ) ;
#6640 = AXIS2_PLACEMENT_3D ( 'NONE', #38969, #31676, #14584 ) ;
#6641 = CARTESIAN_POINT ( 'NONE',  ( 117.3911214775786505, -1.561330072975668504, -17.79121239304076951 ) ) ;
#6642 = CARTESIAN_POINT ( 'NONE',  ( 135.4522060580516438, -8.536173890036971912, -18.13819535414095085 ) ) ;
#6643 = ORIENTED_EDGE ( 'NONE', *, *, #32613, .F. ) ;
#6644 = VECTOR ( 'NONE', #22480, 1000.000000000000114 ) ;
#6645 = CARTESIAN_POINT ( 'NONE',  ( 121.8965016859119856, -9.665098340737509730, -17.37397104707595474 ) ) ;
#6646 = CARTESIAN_POINT ( 'NONE',  ( 61.57437703972069443, -12.46983040987277214, -9.683387576578219580 ) ) ;
#6647 = CARTESIAN_POINT ( 'NONE',  ( 123.6310548109119765, -5.638512984488999180, -18.83840828888717311 ) ) ;
#6648 = CARTESIAN_POINT ( 'NONE',  ( 107.8433483795247838, -0.7896495226426338832, -9.318865927141430916 ) ) ;
#6649 = CARTESIAN_POINT ( 'NONE',  ( 120.5678148109119832, -1.833838273342659253, -17.42832698103878286 ) ) ;
#6650 = EDGE_LOOP ( 'NONE', ( #15048, #28604, #9104, #28356, #1184, #24409 ) ) ;
#6651 = ORIENTED_EDGE ( 'NONE', *, *, #1232, .T. ) ;
#6652 = CARTESIAN_POINT ( 'NONE',  ( 124.1415948109119540, -3.505236298600246325, -18.68346056562440793 ) ) ;
#6653 = CARTESIAN_POINT ( 'NONE',  ( 124.5954081442453116, -6.222761293078241884, -8.102969835052219238 ) ) ;
#6654 = DIRECTION ( 'NONE',  ( -0.000000000000000000, -0.9284778069183721172, -0.3713878862591650232 ) ) ;
#6655 = CARTESIAN_POINT ( 'NONE',  ( 135.3184548109119874, -4.863998795839242995, -13.39321520033831447 ) ) ;
#6656 = CARTESIAN_POINT ( 'NONE',  ( 121.6456214775786293, -10.63000616557722466, -14.87417383870573495 ) ) ;
#6657 = EDGE_CURVE ( 'NONE', #38752, #33939, #35684, .T. ) ;
#6658 = DIRECTION ( 'NONE',  ( 0.000000000000000000, 0.000000000000000000, -1.000000000000000000 ) ) ;
#6659 = CIRCLE ( 'NONE', #8827, 0.8509999999999994236 ) ;
#6660 = CARTESIAN_POINT ( 'NONE',  ( 42.57150613532612482, -13.18613447638990088, -19.39321520033831447 ) ) ;
#6661 = CARTESIAN_POINT ( 'NONE',  ( 119.0361948109119652, -7.893985811506177619, -18.51759400769804742 ) ) ;
#6663 = CARTESIAN_POINT ( 'NONE',  ( 121.3619881442452879, -5.574606645277164318, -18.38911715685844683 ) ) ;
#6662 = CARTESIAN_POINT ( 'NONE',  ( 118.0151148109119816, -10.63000616557722466, -14.87417383870573495 ) ) ;
#6664 = CARTESIAN_POINT ( 'NONE',  ( 123.3474214775786209, -0.1624402480850797581, -16.17319339645315424 ) ) ;
#6665 = CARTESIAN_POINT ( 'NONE',  ( 115.4624148109119943, -5.638512984488999180, -18.83840828888717311 ) ) ;
#6666 = EDGE_CURVE ( 'NONE', #13270, #16241, #28196, .T. ) ;
#6667 = ORIENTED_EDGE ( 'NONE', *, *, #29474, .T. ) ;
#6668 = CARTESIAN_POINT ( 'NONE',  ( 112.7962614775786676, -3.383040157471821630, -19.15922257007629170 ) ) ;
#6669 = EDGE_CURVE ( 'NONE', #43343, #14177, #24580, .T. ) ;
#6670 = CARTESIAN_POINT ( 'NONE',  ( 125.3223148109119904, 0.3778260857404745487, -12.04688916545782185 ) ) ;
#6671 = CARTESIAN_POINT ( 'NONE',  ( 107.0099108795247815, -8.938348069036489818, -9.318865927141430916 ) ) ;
#6672 = CIRCLE ( 'NONE', #34323, 1.610000000000000986 ) ;
#6673 = CARTESIAN_POINT ( 'NONE',  ( 107.9822546295247889, -4.863998795839590272, -18.39754474579285315 ) ) ;
#6674 = CARTESIAN_POINT ( 'NONE',  ( 108.6767858795247861, -0.7896495226426338832, -17.46756447353520159 ) ) ;
#6675 = CARTESIAN_POINT ( 'NONE',  ( 120.7947214775786193, -9.261995988541697145, -16.69588392320189030 ) ) ;
#6676 = CARTESIAN_POINT ( 'NONE',  ( 124.1415948109119540, -3.505236298600246325, -18.68346056562440793 ) ) ;
#6677 = ORIENTED_EDGE ( 'NONE', *, *, #7215, .F. ) ;
#6678 = CARTESIAN_POINT ( 'NONE',  ( 125.3328548109119964, -9.261995988541697145, -16.69588392320189030 ) ) ;
#6679 = CARTESIAN_POINT ( 'NONE',  ( 112.3578015045248861, -2.477300249445798297, -7.631215200338321125 ) ) ;
#6680 = DIRECTION ( 'NONE',  ( -0.2768435750659241079, -0.3568721902840695792, 0.8921882507333129819 ) ) ;
#6681 = CARTESIAN_POINT ( 'NONE',  ( 122.3263414775786373, -6.344957434206665248, -7.627207830600338134 ) ) ;
#6682 = CARTESIAN_POINT ( 'NONE',  ( 126.0703014775786102, -9.988377603198980381, -10.36322818467138518 ) ) ;
#6683 = CARTESIAN_POINT ( 'NONE',  ( 120.2959048109119777, -7.198765429287387718, -17.81462501705257395 ) ) ;
#6684 = CARTESIAN_POINT ( 'NONE',  ( 113.5904348109119866, -7.893985811506177619, -18.51759400769804742 ) ) ;
#6685 = DIRECTION ( 'NONE',  ( -0.000000000000000000, -0.9284778069183718952, -0.3713878862591649677 ) ) ;
#6686 = CARTESIAN_POINT ( 'NONE',  ( 115.9693640045247776, 0.1403307496149616695, -15.46607636864997204 ) ) ;
#6687 = ORIENTED_EDGE ( 'NONE', *, *, #20591, .T. ) ;
#6688 = LINE ( 'NONE', #44996, #33195 ) ;
#6689 = CARTESIAN_POINT ( 'NONE',  ( 112.3424481442453384, -3.505236298600246325, -18.68346056562440793 ) ) ;
#6690 = CARTESIAN_POINT ( 'NONE',  ( 112.1722681442453222, -0.4660016031367893996, -10.09054647747474043 ) ) ;
#6691 = CARTESIAN_POINT ( 'NONE',  ( 108.0517077545248696, -2.791137627527939813, -18.39754474579286025 ) ) ;
#6692 = CARTESIAN_POINT ( 'NONE',  ( 105.6208483795248299, -8.402594152722688392, -16.93181055722141792 ) ) ;
#6693 = EDGE_CURVE ( 'NONE', #28148, #15377, #10642, .T. ) ;
#6694 = CARTESIAN_POINT ( 'NONE',  ( 123.2906948109119867, -1.833838273342659697, -17.42832698103878286 ) ) ;
#6695 = CARTESIAN_POINT ( 'NONE',  ( 116.6536748109119941, -10.15424416112533912, -14.75197769757731336 ) ) ;
#6696 = CARTESIAN_POINT ( 'NONE',  ( 113.6471614775786492, -4.153390946401321671, -8.397313243818183892 ) ) ;
#6697 = EDGE_LOOP ( 'NONE', ( #6565, #17462, #25426, #2406, #42704 ) ) ;
#6698 = EDGE_CURVE ( 'NONE', #12923, #23361, #1705, .T. ) ;
#6699 = ADVANCED_FACE ( 'NONE', ( #43447 ), #23879, .F. ) ;
#6700 = CARTESIAN_POINT ( 'NONE',  ( 121.1325173109119788, -9.289237151508434209, -11.05642687123711276 ) ) ;
#6701 = CARTESIAN_POINT ( 'NONE',  ( 119.6034614775786196, -6.344957434206665248, -7.627207830600338134 ) ) ;
#6702 = AXIS2_PLACEMENT_3D ( 'NONE', #25084, #4319, #25312 ) ;
#6703 = DIRECTION ( 'NONE',  ( 1.000000000000000000, 0.000000000000000000, -0.000000000000000000 ) ) ;
#6704 = ORIENTED_EDGE ( 'NONE', *, *, #28576, .F. ) ;
#6705 = DIRECTION ( 'NONE',  ( 0.000000000000000000, 0.9284778069183720062, 0.3713878862591650232 ) ) ;
#6706 = AXIS2_PLACEMENT_3D ( 'NONE', #25280, #14790, #1322 ) ;
#6707 = ORIENTED_EDGE ( 'NONE', *, *, #32913, .F. ) ;
#6708 = CARTESIAN_POINT ( 'NONE',  ( 115.9729548109119861, -3.505236298600246325, -18.68346056562440793 ) ) ;
#6709 = CARTESIAN_POINT ( 'NONE',  ( 112.9664414775786412, -9.859900752359374465, -12.68260735090039404 ) ) ;
#6710 = CARTESIAN_POINT ( 'NONE',  ( 114.7356558072985564, 0.3208234527006404435, -15.99825685930877661 ) ) ;
#6711 = CARTESIAN_POINT ( 'NONE',  ( 122.0354079359119908, -4.360204210389833968, -8.000047426360245240 ) ) ;
#6712 = ORIENTED_EDGE ( 'NONE', *, *, #22060, .F. ) ;
#6713 = CARTESIAN_POINT ( 'NONE',  ( 123.0385396737536752, -8.611453504372539314, -17.77011218421760574 ) ) ;
#6714 = CARTESIAN_POINT ( 'NONE',  ( 91.11246428952674137, -25.99489077589524300, -13.39321520033831625 ) ) ;
#6715 = CARTESIAN_POINT ( 'NONE',  ( 115.4137390045248566, 0.8980012041604421569, -15.77991374673208469 ) ) ;
#6716 = CARTESIAN_POINT ( 'NONE',  ( 115.5526452545247622, -9.868328341294102302, -15.46607636865001645 ) ) ;
#6717 = CARTESIAN_POINT ( 'NONE',  ( 122.4397948109119767, -0.1624402480850797581, -16.17319339645315424 ) ) ;
#6718 = CARTESIAN_POINT ( 'NONE',  ( 114.6682414775786469, -7.894159318335828068, -9.358103419637847864 ) ) ;
#6719 = CARTESIAN_POINT ( 'NONE',  ( 119.9375029525735670, -1.111561923218657322, -17.14115599315433158 ) ) ;
#6720 = VERTEX_POINT ( 'NONE', #39790 ) ;
#6721 = CARTESIAN_POINT ( 'NONE',  ( 123.9584548109119737, -8.523281198020143279, -6.279169073056789507 ) ) ;
#6722 = CARTESIAN_POINT ( 'NONE',  ( 112.7395348109119766, -4.153390946401321671, -8.397313243818183892 ) ) ;
#6724 = VECTOR ( 'NONE', #41344, 1000.000000000000114 ) ;
#6723 = CARTESIAN_POINT ( 'NONE',  ( 122.4799043147880440, -2.395992375830759524, -17.92872468182853396 ) ) ;
#6725 = DIRECTION ( 'NONE',  ( -0.2768435750659241079, -0.3568721902840695792, 0.8921882507333129819 ) ) ;
#6727 = CARTESIAN_POINT ( 'NONE',  ( 126.1270281442452870, -10.30919188438810075, -12.61870101168855918 ) ) ;
#6726 = CARTESIAN_POINT ( 'NONE',  ( 65.96249443994719286, -37.38467533475423465, -4.893215200338314474 ) ) ;
#6728 = CARTESIAN_POINT ( 'NONE',  ( 125.6164881442453094, -9.565557343593413364, -10.61323700422348004 ) ) ;
#6729 = APPLICATION_CONTEXT ( 'automotive_design' ) ;
#6730 = ORIENTED_EDGE ( 'NONE', *, *, #24760, .F. ) ;
#6731 = CARTESIAN_POINT ( 'NONE',  ( 113.8173414775786512, 0.2603800115204892296, -16.42320221600525088 ) ) ;
#6732 = CARTESIAN_POINT ( 'NONE',  ( 73.53114257624162065, -54.10809544429395856, -19.39321520033831447 ) ) ;
#6733 = CARTESIAN_POINT ( 'NONE',  ( 115.6915515045247531, -2.477300249445798297, -7.631215200338321125 ) ) ;
#6734 = EDGE_CURVE ( 'NONE', #24095, #41818, #14382, .T. ) ;
#6735 = CARTESIAN_POINT ( 'NONE',  ( 126.2972081442452890, -2.084020599724406786, -8.691656652584148546 ) ) ;
#6736 = CARTESIAN_POINT ( 'NONE',  ( 124.7088614775786226, -9.565557343593413364, -10.61323700422348004 ) ) ;
#6737 = CARTESIAN_POINT ( 'NONE',  ( 124.9252281442453096, -8.862178061932084461, -16.39564131203287545 ) ) ;
#6738 = CARTESIAN_POINT ( 'NONE',  ( 112.0105358795248804, -8.402594152722688392, -9.854619843455216355 ) ) ;
#6739 = CIRCLE ( 'NONE', #22016, 1.499999999999999778 ) ;
#6740 = DIRECTION ( 'NONE',  ( -0.2768435750659243855, -0.3568721902840678029, 0.8921882507333135370 ) ) ;
#6741 = LINE ( 'NONE', #6043, #25999 ) ;
#6742 = CARTESIAN_POINT ( 'NONE',  ( 114.2711548109119803, -0.1624402480850797581, -16.17319339645315424 ) ) ;
#6743 = CARTESIAN_POINT ( 'NONE',  ( 106.5931921295248372, 0.8980012041604618078, -13.39321520033831447 ) ) ;
#6744 = LINE ( 'NONE', #44374, #21890 ) ;
#6745 = CARTESIAN_POINT ( 'NONE',  ( 109.9269421295247753, 0.8980012041604618078, -13.39321520033831447 ) ) ;
#6746 = CARTESIAN_POINT ( 'NONE',  ( 124.4252281442452812, -9.261995988541697145, -16.69588392320189030 ) ) ;
#6747 = CARTESIAN_POINT ( 'NONE',  ( 112.3424481442453384, -3.505236298600246325, -18.68346056562440793 ) ) ;
#6748 = LINE ( 'NONE', #12920, #39378 ) ;
#6749 = CARTESIAN_POINT ( 'NONE',  ( 120.4543614775786295, -4.089484607189486809, -7.948022111789456723 ) ) ;
#6750 = CARTESIAN_POINT ( 'NONE',  ( 115.2922348109119781, -10.63000616557722466, -14.87417383870573495 ) ) ;
#6751 = ORIENTED_EDGE ( 'NONE', *, *, #21116, .T. ) ;
#6752 = CARTESIAN_POINT ( 'NONE',  ( 113.9307948109119764, -10.15424416112533912, -14.75197769757731336 ) ) ;
#6753 = CARTESIAN_POINT ( 'NONE',  ( 123.7445081442452874, -1.561330072975668948, -17.79121239304076951 ) ) ;
#6754 = CARTESIAN_POINT ( 'NONE',  ( 114.5547881442453217, -5.638512984488999180, -18.83840828888717311 ) ) ;
#6755 = CARTESIAN_POINT ( 'NONE',  ( 116.3700414775786527, -4.153390946401321671, -8.397313243818183892 ) ) ;
#6756 = VERTEX_POINT ( 'NONE', #8114 ) ;
#6757 = EDGE_CURVE ( 'NONE', #17138, #14254, #33931, .T. ) ;
#6758 = CARTESIAN_POINT ( 'NONE',  ( 116.5969481442453031, -9.859900752359374465, -12.68260735090039404 ) ) ;
#6759 = CONICAL_SURFACE ( 'NONE', #11857, 2.999999999999999556, 0.9599310885968830309 ) ;
#6760 = VECTOR ( 'NONE', #26806, 1000.000000000000000 ) ;
#6761 = CARTESIAN_POINT ( 'NONE',  ( 115.4624148109119943, -5.638512984488999180, -18.83840828888717311 ) ) ;
#6762 = CARTESIAN_POINT ( 'NONE',  ( 124.7088614775786226, -9.565557343593413364, -10.61323700422348004 ) ) ;
#6763 = CARTESIAN_POINT ( 'NONE',  ( 116.8252597214867308, -1.616710930489624776, -17.49401746026956772 ) ) ;
#6764 = CARTESIAN_POINT ( 'NONE',  ( 113.8163171295247764, -10.62599879583958540, -13.39321520033831447 ) ) ;
#6765 = VERTEX_POINT ( 'NONE', #43664 ) ;
#6766 = CARTESIAN_POINT ( 'NONE',  ( 128.2184548109119930, -4.863998795839242995, -13.39321520033831447 ) ) ;
#6767 = CARTESIAN_POINT ( 'NONE',  ( 126.2404814775786264, -9.261995988541697145, -16.69588392320189030 ) ) ;
#6768 = CARTESIAN_POINT ( 'NONE',  ( 116.1082702545247827, 0.1403307496149616695, -11.32035403202665336 ) ) ;
#6769 = FACE_OUTER_BOUND ( 'NONE', #5355, .T. ) ;
#6770 = CARTESIAN_POINT ( 'NONE',  ( 122.5910329359119828, -4.283928203966204329, -7.183505701512929775 ) ) ;
#6771 = CARTESIAN_POINT ( 'NONE',  ( 113.0231681442453180, -10.15424416112533912, -14.75197769757731336 ) ) ;
#6772 = CARTESIAN_POINT ( 'NONE',  ( 105.7597546295248350, -4.863998795839590272, -18.39754474579285315 ) ) ;
#6773 = CARTESIAN_POINT ( 'NONE',  ( 123.1545820330015317, -1.172797794773259072, -17.05961127468926719 ) ) ;
#6774 = CARTESIAN_POINT ( 'NONE',  ( 115.4137390045248566, -9.868328341294098749, -11.32035403202665869 ) ) ;
#6775 = CARTESIAN_POINT ( 'NONE',  ( 118.3554748109119998, 0.2603800115204892296, -16.42320221600525088 ) ) ;
#6776 = CARTESIAN_POINT ( 'NONE',  ( 136.9861655118718886, -4.492900143882628150, -18.85368254081607375 ) ) ;
#6777 = DIRECTION ( 'NONE',  ( -0.9908103287288504424, 0.1352586133457950313, 0.000000000000000000 ) ) ;
#6778 = FACE_OUTER_BOUND ( 'NONE', #3218, .T. ) ;
#6779 = CARTESIAN_POINT ( 'NONE',  ( 121.0216281442452981, -7.894159318335828068, -9.358103419637847864 ) ) ;
#6780 = VERTEX_POINT ( 'NONE', #26109 ) ;
#6781 = CARTESIAN_POINT ( 'NONE',  ( 126.0135748109119902, -8.166667518702819706, -8.995218007635861213 ) ) ;
#6782 = CARTESIAN_POINT ( 'NONE',  ( 118.3554748109119998, 0.2603800115204892296, -16.42320221600525088 ) ) ;
#6783 = CARTESIAN_POINT ( 'NONE',  ( 117.0111608795247946, -1.325403438956436419, -16.93181055722141792 ) ) ;
#6784 = CARTESIAN_POINT ( 'NONE',  ( 117.2209414775786485, -2.084020599724406786, -8.691656652584148546 ) ) ;
#6786 = CARTESIAN_POINT ( 'NONE',  ( 112.5126281442453120, 0.1319031606808879209, -14.10382304977623669 ) ) ;
#6785 = CIRCLE ( 'NONE', #12614, 1.499999999999999334 ) ;
#6787 = CARTESIAN_POINT ( 'NONE',  ( 112.4967077545247633, -7.250697342233347165, -7.631215200338321125 ) ) ;
#6788 = CARTESIAN_POINT ( 'NONE',  ( 70.19189222814998175, -56.50588100528558044, -39.03625958650156491 ) ) ;
#6789 = CARTESIAN_POINT ( 'NONE',  ( 112.4967077545247633, -7.250697342233347165, -7.631215200338321125 ) ) ;
#6790 = CARTESIAN_POINT ( 'NONE',  ( 115.0086014775786509, -5.574606645277164318, -18.38911715685844683 ) ) ;
#6791 = VECTOR ( 'NONE', #553, 999.9999999999998863 ) ;
#6792 = CARTESIAN_POINT ( 'NONE',  ( 121.4754414775786131, -1.833838273342659697, -17.42832698103878286 ) ) ;
#6793 = DIRECTION ( 'NONE',  ( -1.000000000000000000, 0.000000000000000000, 0.000000000000000000 ) ) ;
#6794 = CARTESIAN_POINT ( 'NONE',  ( 120.9241579359119925, -5.444069387712269226, -19.60292469916370450 ) ) ;
#6795 = CARTESIAN_POINT ( 'NONE',  ( 107.9822546295247889, -4.863998795839590272, -18.39754474579285315 ) ) ;
#6796 = DIRECTION ( 'NONE',  ( 0.9063289528979890930, 0.4225728684367167087, 0.000000000000000000 ) ) ;
#6797 = CARTESIAN_POINT ( 'NONE',  ( 115.5758681442453053, -1.561330072975668060, -17.79121239304076951 ) ) ;
#6798 = CARTESIAN_POINT ( 'NONE',  ( 114.9518748109119883, -1.834011780172310813, -8.268836392978581529 ) ) ;
#6799 = CARTESIAN_POINT ( 'NONE',  ( 0.04488520489200759078, -6.166763362545027327, -7.393215200338315363 ) ) ;
#6800 = ORIENTED_EDGE ( 'NONE', *, *, #32283, .T. ) ;
#6801 = CARTESIAN_POINT ( 'NONE',  ( 123.6849955490782804, -3.391418706753638546, -14.10518582020394618 ) ) ;
#6802 = ORIENTED_EDGE ( 'NONE', *, *, #27375, .T. ) ;
#6803 = CARTESIAN_POINT ( 'NONE',  ( 122.2696148109119889, -4.089484607189486809, -7.948022111789456723 ) ) ;
#6804 = CARTESIAN_POINT ( 'NONE',  ( 111.8319081442453182, -5.638512984488999180, -18.83840828888717311 ) ) ;
#6805 = EDGE_CURVE ( 'NONE', #42907, #17457, #31856, .T. ) ;
#6806 = CARTESIAN_POINT ( 'NONE',  ( 118.6391081442452986, -5.574606645277164318, -18.38911715685844683 ) ) ;
#6807 = SURFACE_SIDE_STYLE ('',( #397 ) ) ;
#6808 = CARTESIAN_POINT ( 'NONE',  ( 87.44708369096657918, -25.99489077589588604, -11.39321520033831447 ) ) ;
#6809 = CARTESIAN_POINT ( 'NONE',  ( 122.1561614775786353, -0.4660016031367893996, -10.09054647747474043 ) ) ;
#6810 = CARTESIAN_POINT ( 'NONE',  ( 116.6536748109119941, 0.9020085738987339008, -11.91225656197089222 ) ) ;
#6811 = CARTESIAN_POINT ( 'NONE',  ( 109.2324108795247923, -1.325403438956436419, -16.93181055722141792 ) ) ;
#6812 = CARTESIAN_POINT ( 'NONE',  ( 113.2500748109119968, -3.505236298600246325, -18.68346056562440793 ) ) ;
#6813 = DIRECTION ( 'NONE',  ( 1.000000000000000000, 0.000000000000000000, 0.000000000000000000 ) ) ;
#6814 = ORIENTED_EDGE ( 'NONE', *, *, #23941, .F. ) ;
#6815 = CARTESIAN_POINT ( 'NONE',  ( 118.4689281442453392, 0.9020085738987339008, -11.91225656197089222 ) ) ;
#6816 = CIRCLE ( 'NONE', #2433, 15.89999999999999680 ) ;
#6817 = CARTESIAN_POINT ( 'NONE',  ( 91.77400275106518279, -25.99489077589524300, -13.39321520033831625 ) ) ;
#6818 = CARTESIAN_POINT ( 'NONE',  ( 116.5402214775786405, 0.2603800115204892296, -16.42320221600525088 ) ) ;
#6819 = ORIENTED_EDGE ( 'NONE', *, *, #11970, .F. ) ;
#6820 = CARTESIAN_POINT ( 'NONE',  ( 107.2877233795247776, -1.325403438956436419, -9.854619843455211026 ) ) ;
#6821 = CIRCLE ( 'NONE', #12652, 5.999999999999997335 ) ;
#6822 = CARTESIAN_POINT ( 'NONE',  ( 125.2194014775786286, -10.30919188438810075, -12.61870101168855918 ) ) ;
#6823 = ADVANCED_FACE ( 'NONE', ( #29532 ), #7846, .T. ) ;
#6824 = CARTESIAN_POINT ( 'NONE',  ( 143.3676850761856940, -69.76310523276724496, 3.106784799661685526 ) ) ;
#6825 = CARTESIAN_POINT ( 'NONE',  ( 69.48536631248848039, -66.77523564985355620, -42.98127819198803934 ) ) ;
#6826 = CARTESIAN_POINT ( 'NONE',  ( 78.01659465443469799, -57.60307796775784084, -1.014495093810897863 ) ) ;
#6827 = CARTESIAN_POINT ( 'NONE',  ( 116.4267681442453153, -6.222761293078241884, -8.102969835052219238 ) ) ;
#6828 = CARTESIAN_POINT ( 'NONE',  ( 93.93057702947278642, -25.99489077589524300, -13.39321520033831447 ) ) ;
#6829 = CARTESIAN_POINT ( 'NONE',  ( 117.6747548109119919, -7.643976991954077427, -18.09477374809248928 ) ) ;
#6830 = AXIS2_PLACEMENT_3D ( 'NONE', #28636, #39112, #38877 ) ;
#6831 = FACE_BOUND ( 'NONE', #906, .T. ) ;
#6832 = CARTESIAN_POINT ( 'NONE',  ( 120.4543614775786295, -5.574606645277164318, -18.38911715685844683 ) ) ;
#6833 = CARTESIAN_POINT ( 'NONE',  ( 121.1325173109119788, 0.2312338769422704887, -16.08380026872395874 ) ) ;
#6834 = CARTESIAN_POINT ( 'NONE',  ( 115.4056881442453459, -7.893985811506177619, -18.51759400769804742 ) ) ;
#6835 = CARTESIAN_POINT ( 'NONE',  ( 125.7866681442452688, -0.4660016031367893996, -10.09054647747474043 ) ) ;
#6836 = CARTESIAN_POINT ( 'NONE',  ( 116.1998614775786507, 0.4262465694468514643, -12.03445270309931736 ) ) ;
#6837 = ORIENTED_EDGE ( 'NONE', *, *, #41809, .F. ) ;
#6838 = CARTESIAN_POINT ( 'NONE',  ( 115.4624148109119943, -5.638512984488999180, -18.83840828888717311 ) ) ;
#6839 = CARTESIAN_POINT ( 'NONE',  ( 109.5102233795247884, -8.938348069036489818, -17.46756447353520159 ) ) ;
#6840 = DIRECTION ( 'NONE',  ( 1.000000000000000000, 0.000000000000000000, 0.000000000000000000 ) ) ;
#6841 = CARTESIAN_POINT ( 'NONE',  ( 105.2735827545248810, -6.936859964151250502, -8.388885654883777576 ) ) ;
#6842 = CARTESIAN_POINT ( 'NONE',  ( 113.5403276191212854, 0.4261359969231631739, -12.14321520033833046 ) ) ;
#6843 = CARTESIAN_POINT ( 'NONE',  ( 120.8514481442452961, -7.893985811506177619, -18.51759400769804742 ) ) ;
#6844 = ORIENTED_EDGE ( 'NONE', *, *, #35027, .F. ) ;
#6845 = CARTESIAN_POINT ( 'NONE',  ( 118.4361142721482878, -2.287189184988681401, -18.07361239780446738 ) ) ;
#6846 = CARTESIAN_POINT ( 'NONE',  ( 118.4122014775786340, -9.859900752359374465, -12.68260735090039404 ) ) ;
#6847 = CARTESIAN_POINT ( 'NONE',  ( 123.9106423109119675, -9.959231468620748373, -10.70263013195265778 ) ) ;
#6848 = CARTESIAN_POINT ( 'NONE',  ( 121.6456214775786293, -10.63000616557722466, -14.87417383870573495 ) ) ;
#6849 = CIRCLE ( 'NONE', #32314, 4.499999999999994671 ) ;
#6850 = CARTESIAN_POINT ( 'NONE',  ( 112.0799890045248475, -9.868328341294098749, -11.32035403202665869 ) ) ;
#6851 = CARTESIAN_POINT ( 'NONE',  ( 89.21236786697126320, -10.20601085363140648, -13.93603761494362736 ) ) ;
#6852 = ORIENTED_EDGE ( 'NONE', *, *, #4845, .T. ) ;
#6853 = CARTESIAN_POINT ( 'NONE',  ( 113.0798948109119948, -0.4660016031367893996, -10.09054647747474043 ) ) ;
#6854 = CARTESIAN_POINT ( 'NONE',  ( 112.2289948109119848, -1.834011780172310813, -8.268836392978581529 ) ) ;
#6855 = CARTESIAN_POINT ( 'NONE',  ( 123.6310548109119765, -5.638512984488999180, -18.83840828888717311 ) ) ;
#6856 = CARTESIAN_POINT ( 'NONE',  ( 118.2420214775786320, -6.222761293078241884, -8.102969835052219238 ) ) ;
#6857 = CARTESIAN_POINT ( 'NONE',  ( 69.36136150295220659, -101.1685209014307674, -50.56525720990386219 ) ) ;
#6858 = CARTESIAN_POINT ( 'NONE',  ( 118.8660148109119774, -10.30919188438810075, -12.61870101168855918 ) ) ;
#6859 = DIRECTION ( 'NONE',  ( 0.9908103287288506644, -0.1352586133457941986, 0.000000000000000000 ) ) ;
#6860 = CARTESIAN_POINT ( 'NONE',  ( 122.6667014775786413, -2.084020599724406786, -8.691656652584148546 ) ) ;
#6861 = ORIENTED_EDGE ( 'NONE', *, *, #8696, .T. ) ;
#6862 = CARTESIAN_POINT ( 'NONE',  ( 88.93653725331050452, -10.83229915613791761, -18.64321520033831803 ) ) ;
#6863 = CARTESIAN_POINT ( 'NONE',  ( 115.9162281442453235, -4.089484607189486809, -7.948022111789456723 ) ) ;
#6864 = CARTESIAN_POINT ( 'NONE',  ( 136.0320772899191297, -8.512149301715753680, -18.04415937378387724 ) ) ;
#6865 = ORIENTED_EDGE ( 'NONE', *, *, #10240, .T. ) ;
#6866 = LINE ( 'NONE', #20774, #22377 ) ;
#6867 = CARTESIAN_POINT ( 'NONE',  ( 63.13539060704677297, -12.63253393809564784, -10.30225669948812950 ) ) ;
#6868 = CARTESIAN_POINT ( 'NONE',  ( 123.9146881442452894, 0.9020085738987339008, -11.91225656197089222 ) ) ;
#6869 = CARTESIAN_POINT ( 'NONE',  ( 107.7044421295247929, 0.8980012041604618078, -13.39321520033831447 ) ) ;
#6870 = CARTESIAN_POINT ( 'NONE',  ( 119.9438214775786378, -2.084020599724406786, -8.691656652584148546 ) ) ;
#6871 = EDGE_LOOP ( 'NONE', ( #26996, #22919, #18770, #23061 ) ) ;
#6872 = ORIENTED_EDGE ( 'NONE', *, *, #9270, .T. ) ;
#6873 = CARTESIAN_POINT ( 'NONE',  ( 113.1933481442453058, -4.089484607189486809, -7.948022111789456723 ) ) ;
#6874 = CARTESIAN_POINT ( 'NONE',  ( 123.2339681442453241, -3.505236298600246325, -18.68346056562440793 ) ) ;
#6875 = SURFACE_STYLE_USAGE ( .BOTH. , #31037 ) ;
#6876 = CARTESIAN_POINT ( 'NONE',  ( 117.2294421295247844, 1.035107641088057973, -4.893215200338314474 ) ) ;
#6877 = CARTESIAN_POINT ( 'NONE',  ( 123.0637881442452937, -0.4660016031367893996, -10.09054647747474043 ) ) ;
#6878 = DIRECTION ( 'NONE',  ( 0.9609149988134843001, -0.1028163501681632064, 0.2570431154366505933 ) ) ;
#6879 = CARTESIAN_POINT ( 'NONE',  ( 60.53937939559665438, -4.256997083809236138, -19.39321520033831447 ) ) ;
#6880 = CARTESIAN_POINT ( 'NONE',  ( 120.2274548109119934, 0.5811942927096110934, -14.16772938898807510 ) ) ;
#6882 = CARTESIAN_POINT ( 'NONE',  ( 120.7379948109119709, 0.4262465694468514643, -12.03445270309931736 ) ) ;
#6881 = CARTESIAN_POINT ( 'NONE',  ( 119.7736414775786358, -10.30919188438810075, -12.61870101168855918 ) ) ;
#6883 = CARTESIAN_POINT ( 'NONE',  ( 75.95778847736481509, -3.256761025687722189, -18.64321520033831803 ) ) ;
#6884 = CARTESIAN_POINT ( 'NONE',  ( 115.3489614775786407, -9.261995988541697145, -16.69588392320189030 ) ) ;
#6885 = ADVANCED_FACE ( 'NONE', ( #29752 ), #40247, .T. ) ;
#6886 = ORIENTED_EDGE ( 'NONE', *, *, #11485, .F. ) ;
#6887 = CARTESIAN_POINT ( 'NONE',  ( 125.2761281442453338, 0.4262465694465857324, -12.03445270309828175 ) ) ;
#6888 = CARTESIAN_POINT ( 'NONE',  ( 110.2047546295247855, -4.863998795839590272, -7.631215200338315796 ) ) ;
#6889 = CARTESIAN_POINT ( 'NONE',  ( 109.7880358795247986, -8.402594152722688392, -9.854619843455216355 ) ) ;
#6890 = CARTESIAN_POINT ( 'NONE',  ( 106.8015515045248378, -2.477300249445798297, -7.631215200338321125 ) ) ;
#6891 = DIRECTION ( 'NONE',  ( 1.000000000000000000, 0.000000000000000000, -0.000000000000000000 ) ) ;
#6892 = CARTESIAN_POINT ( 'NONE',  ( 113.3068014775786594, -8.166667518702817929, -8.995218007635859436 ) ) ;
#6893 = ORIENTED_EDGE ( 'NONE', *, *, #26511, .T. ) ;
#6894 = CARTESIAN_POINT ( 'NONE',  ( 122.7801548109119665, -3.383040157471821630, -19.15922257007629170 ) ) ;
#6895 = CARTESIAN_POINT ( 'NONE',  ( 112.9828796295247884, -4.863998795839590272, -19.15521520033831493 ) ) ;
#6896 = DIRECTION ( 'NONE',  ( 0.9387755102040817867, -0.3445294493088593701, 0.000000000000000000 ) ) ;
#6897 = CARTESIAN_POINT ( 'NONE',  ( 125.4463081442452932, -5.638512984488999180, -18.83840828888717311 ) ) ;
#6898 = CARTESIAN_POINT ( 'NONE',  ( 125.2194014775786286, -10.30919188438810075, -12.61870101168855918 ) ) ;
#6899 = DIRECTION ( 'NONE',  ( 0.1352586133457950590, 0.9908103287288504424, 0.000000000000000000 ) ) ;
#6900 = CARTESIAN_POINT ( 'NONE',  ( 113.1366214775786432, -1.834011780172310813, -8.268836392978581529 ) ) ;
#6901 = CARTESIAN_POINT ( 'NONE',  ( 96.54708369096698561, -25.64989040597826175, -15.57695047384496156 ) ) ;
#6902 = CARTESIAN_POINT ( 'NONE',  ( 115.2053796295247849, -4.863998795839590272, -8.388885654883775800 ) ) ;
#6903 = AXIS2_PLACEMENT_3D ( 'NONE', #22847, #5960, #9392 ) ;
#6904 = EDGE_LOOP ( 'NONE', ( #6091, #35097, #32843, #26335 ) ) ;
#6905 = FACE_OUTER_BOUND ( 'NONE', #27682, .T. ) ;
#6906 = CARTESIAN_POINT ( 'NONE',  ( 114.7249681442453237, -9.565557343593413364, -10.61323700422348004 ) ) ;
#6907 = CARTESIAN_POINT ( 'NONE',  ( 113.5904348109119866, -7.893985811506177619, -18.51759400769804742 ) ) ;
#6908 = CARTESIAN_POINT ( 'NONE',  ( 115.1359265045248605, -7.250697342233347165, -19.15521520033831138 ) ) ;
#6909 = CARTESIAN_POINT ( 'NONE',  ( 107.4266296295248821, -4.863998795839590272, -8.388885654883775800 ) ) ;
#6910 = CARTESIAN_POINT ( 'NONE',  ( 120.9649014775786355, -6.222761293078241884, -8.102969835052219238 ) ) ;
#6911 = UNCERTAINTY_MEASURE_WITH_UNIT (LENGTH_MEASURE( 1.000000000000000082E-05 ), #38688, 'distance_accuracy_value', 'NONE');
#6912 = CARTESIAN_POINT ( 'NONE',  ( 116.7671281442453335, -7.643976991954077427, -18.09477374809248928 ) ) ;
#6913 = CARTESIAN_POINT ( 'NONE',  ( 111.3213681442453264, -7.643976991954077427, -18.09477374809248928 ) ) ;
#6914 = VERTEX_POINT ( 'NONE', #5126 ) ;
#6915 = VECTOR ( 'NONE', #22072, 1000.000000000000114 ) ;
#6916 = EDGE_CURVE ( 'NONE', #6181, #24205, #42107, .T. ) ;
#6917 = CARTESIAN_POINT ( 'NONE',  ( 121.8965016859119856, -0.6942167230862511529, -9.935906262978006609 ) ) ;
#6918 = CARTESIAN_POINT ( 'NONE',  ( 69.36136150295220659, -101.1685209014307674, -50.56525720990386219 ) ) ;
#6919 = CARTESIAN_POINT ( 'NONE',  ( 115.2355081442453155, 0.1319031606808879209, -14.10382304977623669 ) ) ;
#6920 = ORIENTED_EDGE ( 'NONE', *, *, #5262, .F. ) ;
#6921 = CARTESIAN_POINT ( 'NONE',  ( 126.3509913982019413, -9.162490483930437080, -16.07503793292245931 ) ) ;
#6922 = EDGE_CURVE ( 'NONE', #15443, #28262, #37701, .T. ) ;
#6923 = EDGE_CURVE ( 'NONE', #17457, #21347, #18024, .T. ) ;
#6924 = EDGE_LOOP ( 'NONE', ( #28323, #7052, #35262, #3977 ) ) ;
#6925 = CARTESIAN_POINT ( 'NONE',  ( 117.7314814775786260, -5.574606645277164318, -18.38911715685844683 ) ) ;
#6926 = CARTESIAN_POINT ( 'NONE',  ( 115.5758681442453053, -7.894159318335828068, -9.358103419637847864 ) ) ;
#6927 = CARTESIAN_POINT ( 'NONE',  ( 116.5944421295247793, -4.863998795839590272, -8.393215200338314474 ) ) ;
#6928 = CARTESIAN_POINT ( 'NONE',  ( 122.1743141859119817, -8.321307733199551748, -9.223433127585318303 ) ) ;
#6929 = EDGE_LOOP ( 'NONE', ( #1898, #40656, #36045 ) ) ;
#6930 = ADVANCED_FACE ( 'NONE', ( #8561 ), #33376, .T. ) ;
#6931 = FACE_OUTER_BOUND ( 'NONE', #18754, .T. ) ;
#6932 = CARTESIAN_POINT ( 'NONE',  ( 124.4646854081434526, 2.188825697814051452, -9.798915638107947856 ) ) ;
#6933 = AXIS2_PLACEMENT_3D ( 'NONE', #1805, #36682, #26447 ) ;
#6934 = CARTESIAN_POINT ( 'NONE',  ( 114.9275671295247889, -10.62599879583958540, -13.39321520033831447 ) ) ;
#6935 = DIRECTION ( 'NONE',  ( -0.2768435750659241079, -0.3568721902840686355, 0.8921882507333134260 ) ) ;
#6936 = EDGE_CURVE ( 'NONE', #37642, #19531, #9015, .T. ) ;
#6937 = CARTESIAN_POINT ( 'NONE',  ( 124.1415948109119540, -3.505236298600246325, -18.68346056562440793 ) ) ;
#6938 = CARTESIAN_POINT ( 'NONE',  ( 118.6958348109119754, -3.505236298600246325, -18.68346056562440793 ) ) ;
#6939 = CARTESIAN_POINT ( 'NONE',  ( 109.2294421295247844, 0.2400687412228638684, -12.14321520033831625 ) ) ;
#6940 = EDGE_CURVE ( 'NONE', #3847, #34659, #43718, .T. ) ;
#6941 = EDGE_CURVE ( 'NONE', #33968, #6119, #13115, .T. ) ;
#6942 = ORIENTED_EDGE ( 'NONE', *, *, #15899, .F. ) ;
#6943 = CARTESIAN_POINT ( 'NONE',  ( 86.09323753712084226, -26.60966817898065884, -11.90521360603286816 ) ) ;
#6944 = VECTOR ( 'NONE', #9688, 1000.000000000000114 ) ;
#6945 = CARTESIAN_POINT ( 'NONE',  ( 116.5969481442453031, -9.859900752359374465, -12.68260735090039404 ) ) ;
#6946 = CARTESIAN_POINT ( 'NONE',  ( 84.72166425534338430, -29.42112683882138668, -9.627754957239334388 ) ) ;
#6947 = CARTESIAN_POINT ( 'NONE',  ( 125.0492214775786266, -6.344957434206665248, -7.627207830600338134 ) ) ;
#6948 = CARTESIAN_POINT ( 'NONE',  ( 125.1059481442452750, -1.833838273342660141, -17.42832698103878286 ) ) ;
#6949 = VERTEX_POINT ( 'NONE', #20409 ) ;
#6950 = CARTESIAN_POINT ( 'NONE',  ( 112.3991748109119868, -8.166667518702817929, -8.995218007635859436 ) ) ;
#6951 = CARTESIAN_POINT ( 'NONE',  ( 114.1009748109119784, -4.089484607189490362, -7.948022111789460276 ) ) ;
#6952 = CARTESIAN_POINT ( 'NONE',  ( 114.7886608795247696, -8.938348069036489818, -9.318865927141430916 ) ) ;
#6953 = CARTESIAN_POINT ( 'NONE',  ( 126.2972081442452890, -2.084020599724406786, -8.691656652584148546 ) ) ;
#6954 = CARTESIAN_POINT ( 'NONE',  ( 114.8951481442453115, -0.4660016031367893996, -10.09054647747474043 ) ) ;
#6955 = CARTESIAN_POINT ( 'NONE',  ( 125.2194014775786286, 0.1319031606808879209, -14.10382304977623669 ) ) ;
#6956 = CARTESIAN_POINT ( 'NONE',  ( 112.4272546295247821, -4.863998795839541422, -18.39754474579285315 ) ) ;
#6957 = CARTESIAN_POINT ( 'NONE',  ( 109.6491296295247793, -4.863998795839590272, -8.388885654883775800 ) ) ;
#6958 = CARTESIAN_POINT ( 'NONE',  ( 117.3237071478583573, -3.807985514183284348, -19.09877912889400520 ) ) ;
#6959 = CARTESIAN_POINT ( 'NONE',  ( 109.2294315388255228, -7.824389221362666902, -17.82941758066625582 ) ) ;
#6960 = CARTESIAN_POINT ( 'NONE',  ( 118.1852948109119836, -4.153390946401325223, -8.397313243818185668 ) ) ;
#6961 = CARTESIAN_POINT ( 'NONE',  ( 107.7044421295247929, 0.8980012041604618078, -13.39321520033831447 ) ) ;
#6962 = CARTESIAN_POINT ( 'NONE',  ( 86.48169505875749508, -25.99489077589524300, -13.39321520033831625 ) ) ;
#6963 = CARTESIAN_POINT ( 'NONE',  ( 109.7880358795247986, -0.7896495226426338832, -17.46756447353520159 ) ) ;
#6964 = CARTESIAN_POINT ( 'NONE',  ( 123.8579614775786126, 0.5811942927096110934, -14.16772938898807510 ) ) ;
#6965 = CARTESIAN_POINT ( 'NONE',  ( 124.3685014775786328, -10.63000616557722466, -14.87417383870573495 ) ) ;
#6966 = DIRECTION ( 'NONE',  ( 0.000000000000000000, 0.000000000000000000, -1.000000000000000000 ) ) ;
#6967 = CARTESIAN_POINT ( 'NONE',  ( 120.5678148109119832, -8.166667518702819706, -8.995218007635861213 ) ) ;
#6968 = CARTESIAN_POINT ( 'NONE',  ( 118.0151148109119816, -10.63000616557722466, -14.87417383870573495 ) ) ;
#6969 = ORIENTED_EDGE ( 'NONE', *, *, #39328, .T. ) ;
#6970 = AXIS2_PLACEMENT_3D ( 'NONE', #24595, #38478, #32090 ) ;
#6971 = CARTESIAN_POINT ( 'NONE',  ( 115.8595014775786609, -7.643976991954077427, -18.09477374809248928 ) ) ;
#6972 = CARTESIAN_POINT ( 'NONE',  ( 122.2128881442453263, -1.834011780172310813, -8.268836392978581529 ) ) ;
#6973 = CARTESIAN_POINT ( 'NONE',  ( 115.5191414775786569, -3.383040157471821630, -19.15922257007629170 ) ) ;
#6974 = CARTESIAN_POINT ( 'NONE',  ( 117.0507614775786465, 0.1319031606808879209, -14.10382304977623669 ) ) ;
#6975 = VERTEX_POINT ( 'NONE', #23148 ) ;
#6976 = CARTESIAN_POINT ( 'NONE',  ( 120.5110881442453206, -3.505236298600246325, -18.68346056562440793 ) ) ;
#6977 = AXIS2_PLACEMENT_3D ( 'NONE', #28853, #42765, #5113 ) ;
#6978 = EDGE_CURVE ( 'NONE', #18690, #16480, #29681, .T. ) ;
#6979 = CARTESIAN_POINT ( 'NONE',  ( 118.0718414775786300, -9.261995988541697145, -16.69588392320189030 ) ) ;
#6980 = CARTESIAN_POINT ( 'NONE',  ( 70.19189222814998175, -61.69445140165969121, -37.88057465812982372 ) ) ;
#6981 = CARTESIAN_POINT ( 'NONE',  ( 114.9275671295247889, -10.62599879583958540, -13.39321520033831447 ) ) ;
#6982 = ORIENTED_EDGE ( 'NONE', *, *, #40694, .F. ) ;
#6983 = CARTESIAN_POINT ( 'NONE',  ( 65.82164714941100669, 4.169909004287361221, -7.393215200338315363 ) ) ;
#6984 = DIRECTION ( 'NONE',  ( 0.9659258262890690894, 0.2588190451025180749, 0.000000000000000000 ) ) ;
#6985 = DIRECTION ( 'NONE',  ( 4.336808689942015271E-16, -1.000000000000000000, 1.517883041479705024E-15 ) ) ;
#6986 = CARTESIAN_POINT ( 'NONE',  ( 114.5547881442453217, -5.638512984488999180, -18.83840828888717311 ) ) ;
#6987 = CARTESIAN_POINT ( 'NONE',  ( 71.31713442278440596, 2.423123680056959550, -10.60032198152486238 ) ) ;
#6988 = CARTESIAN_POINT ( 'NONE',  ( 124.6259452904873655, -9.410405169419663096, -15.50563694605804876 ) ) ;
#6989 = DIRECTION ( 'NONE',  ( 0.9609149988134837450, -0.1028163501681639419, 0.2570431154366518145 ) ) ;
#6990 = EDGE_CURVE ( 'NONE', #279, #34887, #32568, .T. ) ;
#6991 = CARTESIAN_POINT ( 'NONE',  ( 123.3116793777725064, -1.267766418764731728, -16.93314635290706605 ) ) ;
#6992 = CARTESIAN_POINT ( 'NONE',  ( 114.7886608795247696, -1.325403438956436419, -16.93181055722141792 ) ) ;
#6993 = CARTESIAN_POINT ( 'NONE',  ( 118.1852948109119836, -5.638512984488999180, -18.83840828888717311 ) ) ;
#6994 = CARTESIAN_POINT ( 'NONE',  ( 123.5880035264548837, -8.247323210606174015, -17.08054893949881858 ) ) ;
#6995 = DIRECTION ( 'NONE',  ( -0.4225728684367169308, 0.9063289528979889820, 0.000000000000000000 ) ) ;
#6996 = CARTESIAN_POINT ( 'NONE',  ( 124.2579079359120016, -4.360204210390138613, -8.000047426360218594 ) ) ;
#6997 = CARTESIAN_POINT ( 'NONE',  ( 121.5321681442453183, -0.1624402480850797581, -16.17319339645315424 ) ) ;
#6998 = VERTEX_POINT ( 'NONE', #12667 ) ;
#6999 = CARTESIAN_POINT ( 'NONE',  ( 124.9924948109119924, -4.089484607189486809, -7.948022111789456723 ) ) ;
#7000 = ADVANCED_FACE ( 'NONE', ( #37030 ), #4849, .T. ) ;
#7001 = CARTESIAN_POINT ( 'NONE',  ( 119.1496481442453046, -3.383040157471821630, -19.15922257007629170 ) ) ;
#7002 = PLANE ( 'NONE',  #21211 ) ;
#7003 = CARTESIAN_POINT ( 'NONE',  ( 116.9373081442452929, -1.833838273342659253, -17.42832698103878286 ) ) ;
#7004 = PRODUCT_RELATED_PRODUCT_CATEGORY ( 'part', '', ( #35013 ) ) ;
#7005 = VECTOR ( 'NONE', #7514, 1000.000000000000114 ) ;
#7006 = CARTESIAN_POINT ( 'NONE',  ( 113.2500748109119968, -3.505236298600246325, -18.68346056562440793 ) ) ;
#7007 = CARTESIAN_POINT ( 'NONE',  ( 82.31000308962319423, -13.76004065658516673, -16.89321520033831447 ) ) ;
#7008 = CARTESIAN_POINT ( 'NONE',  ( 110.8992858795247827, -0.7896495226426338832, -17.46756447353520159 ) ) ;
#7009 = CARTESIAN_POINT ( 'NONE',  ( 122.0427081442452817, -9.859900752359378018, -12.68260735090039759 ) ) ;
#7010 = CARTESIAN_POINT ( 'NONE',  ( 119.8303681442453126, 0.4262465694468514643, -12.03445270309931736 ) ) ;
#7011 = CARTESIAN_POINT ( 'NONE',  ( 109.2293480927346252, -6.550713907899789135, -8.000234073319102635 ) ) ;
#7012 = CARTESIAN_POINT ( 'NONE',  ( 122.7993923109119692, -9.959231468620755479, -10.70263013195267199 ) ) ;
#7013 = CARTESIAN_POINT ( 'NONE',  ( 110.3436608795247764, -1.325403438956436419, -16.93181055722141792 ) ) ;
#7014 = CARTESIAN_POINT ( 'NONE',  ( 70.19189222814998175, -55.19510675323109439, -35.28085945431567438 ) ) ;
#7015 = CARTESIAN_POINT ( 'NONE',  ( 113.9875214775786532, -0.4660016031367893996, -10.09054647747474043 ) ) ;
#7016 = CARTESIAN_POINT ( 'NONE',  ( 114.7816948109119863, 0.5811942927096154232, -14.16772938898807155 ) ) ;
#7017 = CARTESIAN_POINT ( 'NONE',  ( 121.3408766859119794, -9.033780868592240054, -16.85052413769862056 ) ) ;
#7018 = ORIENTED_EDGE ( 'NONE', *, *, #36322, .T. ) ;
#7019 = CARTESIAN_POINT ( 'NONE',  ( 86.34560043013698305, -9.320000780048239619, -14.14321520033831625 ) ) ;
#7020 = CARTESIAN_POINT ( 'NONE',  ( 121.8158014775786171, -5.638512984488999180, -18.83840828888717311 ) ) ;
#7021 = CARTESIAN_POINT ( 'NONE',  ( 113.9307948109119906, 0.9020085738987339008, -11.91225656197089222 ) ) ;
#7022 = CARTESIAN_POINT ( 'NONE',  ( 117.1074881442453233, 0.4262465694468514643, -12.03445270309931736 ) ) ;
#7023 = AXIS2_PLACEMENT_3D ( 'NONE', #557, #24953, #39308 ) ;
#7024 = CARTESIAN_POINT ( 'NONE',  ( 126.1270281442452870, -10.30919188438810075, -12.61870101168855918 ) ) ;
#7025 = CARTESIAN_POINT ( 'NONE',  ( 118.1852948109119836, -5.638512984488999180, -18.83840828888717311 ) ) ;
#7026 = AXIS2_PLACEMENT_3D ( 'NONE', #2661, #17047, #9514 ) ;
#7027 = CARTESIAN_POINT ( 'NONE',  ( 108.1211608795247798, -1.325403438956436419, -16.93181055722141792 ) ) ;
#7028 = CARTESIAN_POINT ( 'NONE',  ( 112.7395348109119766, -4.153390946401321671, -8.397313243818183892 ) ) ;
#7029 = DIRECTION ( 'NONE',  ( 0.000000000000000000, -1.000000000000000000, 0.000000000000000000 ) ) ;
#7030 = VERTEX_POINT ( 'NONE', #43673 ) ;
#7031 = CARTESIAN_POINT ( 'NONE',  ( 119.4900081442453086, -1.834011780172310813, -8.268836392978581529 ) ) ;
#7032 = EDGE_CURVE ( 'NONE', #23460, #16741, #22469, .T. ) ;
#7033 = AXIS2_PLACEMENT_3D ( 'NONE', #3822, #4275, #32087 ) ;
#7034 = CARTESIAN_POINT ( 'NONE',  ( 120.2990798109119766, -2.173413727453600508, -8.297982527556802879 ) ) ;
#7035 = CARTESIAN_POINT ( 'NONE',  ( 117.1074881442453233, -10.63000616557722466, -14.87417383870573495 ) ) ;
#7036 = VERTEX_POINT ( 'NONE', #25675 ) ;
#7037 = CARTESIAN_POINT ( 'NONE',  ( 107.4960827545248350, -6.936859964151250502, -8.388885654883777576 ) ) ;
#7038 = CARTESIAN_POINT ( 'NONE',  ( 124.9357681442453014, -1.834011780172310813, -8.268836392978581529 ) ) ;
#7039 = CARTESIAN_POINT ( 'NONE',  ( 122.1561614775786353, -0.4660016031367685829, -10.09054647747476885 ) ) ;
#7040 = DIRECTION ( 'NONE',  ( 0.000000000000000000, 0.6004852223388321697, -0.7996358532186279566 ) ) ;
#7041 = CARTESIAN_POINT ( 'NONE',  ( 70.19189222814998175, -50.76020450571126474, -33.50691401458669105 ) ) ;
#7042 = CARTESIAN_POINT ( 'NONE',  ( 120.2841814775786276, -10.15424416112533912, -14.75197769757731336 ) ) ;
#7043 = CARTESIAN_POINT ( 'NONE',  ( 2.384484203314607420, -10.01861149699890063, -8.893215200338314474 ) ) ;
#7044 = CARTESIAN_POINT ( 'NONE',  ( 116.2565881442453133, -0.8288870151387760510, -10.36305467784173118 ) ) ;
#7045 = EDGE_CURVE ( 'NONE', #3982, #6624, #20226, .T. ) ;
#7046 = CYLINDRICAL_SURFACE ( 'NONE', #20864, 1.587500000000000355 ) ;
#7047 = CARTESIAN_POINT ( 'NONE',  ( 120.9649014775786355, -6.222761293078241884, -8.102969835052219238 ) ) ;
#7048 = CARTESIAN_POINT ( 'NONE',  ( 120.8547048109119686, -7.554583864224885481, -18.48844787311982785 ) ) ;
#7049 = CARTESIAN_POINT ( 'NONE',  ( 116.9940348109119839, -9.988377603198976828, -10.36322818467138340 ) ) ;
#7050 = DIRECTION ( 'NONE',  ( 0.3127730236694426513, -0.9498278979187093629, 0.000000000000000000 ) ) ;
#7051 = CARTESIAN_POINT ( 'NONE',  ( 116.4267681442453153, -6.222761293078241884, -8.102969835052219238 ) ) ;
#7052 = ORIENTED_EDGE ( 'NONE', *, *, #42339, .T. ) ;
#7053 = CARTESIAN_POINT ( 'NONE',  ( 116.0864081442453113, -9.988377603198976828, -10.36322818467138340 ) ) ;
#7054 = CARTESIAN_POINT ( 'NONE',  ( 108.8156921295247912, 0.8980012041604618078, -13.39321520033831447 ) ) ;
#7055 = CIRCLE ( 'NONE', #29610, 2.999999999999998668 ) ;
#7056 = DIRECTION ( 'NONE',  ( 1.000000000000000000, 0.000000000000000000, 0.000000000000000000 ) ) ;
#7057 = DIRECTION ( 'NONE',  ( 1.000000000000000000, 0.000000000000000000, -0.000000000000000000 ) ) ;
#7058 = CARTESIAN_POINT ( 'NONE',  ( 123.5003147965036447, -8.305800998871427865, -17.19128988610635744 ) ) ;
#7059 = CARTESIAN_POINT ( 'NONE',  ( 123.9714148109119805, -0.4660016031367893996, -10.09054647747474043 ) ) ;
#7060 = ORIENTED_EDGE ( 'NONE', *, *, #27562, .F. ) ;
#7061 = CARTESIAN_POINT ( 'NONE',  ( 127.0400190879708049, -8.899344475176020453, -9.788696381569236493 ) ) ;
#7062 = CARTESIAN_POINT ( 'NONE',  ( 116.4267681442453153, -6.222761293078241884, -8.102969835052219238 ) ) ;
#7063 = CARTESIAN_POINT ( 'NONE',  ( 116.1431348109119881, -10.30919188438809542, -12.61870101168854852 ) ) ;
#7064 = CARTESIAN_POINT ( 'NONE',  ( 122.6667014775786413, -7.893985811506177619, -18.51759400769804742 ) ) ;
#7065 = CARTESIAN_POINT ( 'NONE',  ( 113.1912390045248031, -9.868328341294098749, -11.32035403202665869 ) ) ;
#7066 = CARTESIAN_POINT ( 'NONE',  ( 89.29245855188943892, -9.882163754870950001, -13.24321520033830879 ) ) ;
#7067 = EDGE_LOOP ( 'NONE', ( #28374, #837, #13477, #30475, #29245 ) ) ;
#7068 = CARTESIAN_POINT ( 'NONE',  ( 114.8951481442453115, -0.4660016031367893996, -10.09054647747474043 ) ) ;
#7069 = CARTESIAN_POINT ( 'NONE',  ( 124.6521348109119884, -7.894159318335828068, -9.358103419637847864 ) ) ;
#7070 = CARTESIAN_POINT ( 'NONE',  ( 123.5743281442453139, -7.893985811506177619, -18.51759400769804742 ) ) ;
#7071 = ADVANCED_FACE ( 'NONE', ( #18605 ), #10045, .T. ) ;
#7072 = CARTESIAN_POINT ( 'NONE',  ( 118.5823814775786360, -7.643976991954077427, -18.09477374809248928 ) ) ;
#7073 =( LENGTH_UNIT ( ) NAMED_UNIT ( * ) SI_UNIT ( .MILLI., .METRE. ) );
#7074 = CARTESIAN_POINT ( 'NONE',  ( 119.3765548109119834, 0.9020085738987339008, -11.91225656197089222 ) ) ;
#7075 = CARTESIAN_POINT ( 'NONE',  ( 67.84197459855160162, -53.65469605205331050, -35.39387355951068059 ) ) ;
#7076 = CARTESIAN_POINT ( 'NONE',  ( 123.6310548109119765, -4.153390946401325223, -8.397313243818185668 ) ) ;
#7077 = ORIENTED_EDGE ( 'NONE', *, *, #18100, .F. ) ;
#7078 = DIRECTION ( 'NONE',  ( 0.000000000000000000, 0.000000000000000000, -1.000000000000000000 ) ) ;
#7079 = AXIS2_PLACEMENT_3D ( 'NONE', #41594, #6705, #21046 ) ;
#7080 = CARTESIAN_POINT ( 'NONE',  ( 115.5191414775786569, -3.383040157471821630, -19.15922257007629170 ) ) ;
#7081 = CARTESIAN_POINT ( 'NONE',  ( 123.9714148109119805, -8.899110576539710493, -16.42337572283490132 ) ) ;
#7082 = EDGE_LOOP ( 'NONE', ( #23298, #34259, #11712, #33044 ) ) ;
#7083 = CARTESIAN_POINT ( 'NONE',  ( 60.62063666025856179, -12.51771357505162285, -9.460505781647388091 ) ) ;
#7084 = CARTESIAN_POINT ( 'NONE',  ( 122.6099748109119929, -9.261995988541697145, -16.69588392320189030 ) ) ;
#7085 = CARTESIAN_POINT ( 'NONE',  ( 109.3713171295247832, -10.62599879583958540, -13.39321520033831447 ) ) ;
#7086 = CARTESIAN_POINT ( 'NONE',  ( 118.1285681442453068, -2.084020599724406786, -8.691656652584148546 ) ) ;
#7087 = ORIENTED_EDGE ( 'NONE', *, *, #14827, .F. ) ;
#7088 = ORIENTED_EDGE ( 'NONE', *, *, #9452, .T. ) ;
#7089 = CARTESIAN_POINT ( 'NONE',  ( 114.0442481442453300, -1.834011780172310813, -8.268836392978581529 ) ) ;
#7090 = CARTESIAN_POINT ( 'NONE',  ( 125.7299414775786346, -10.15424416112533912, -14.75197769757731336 ) ) ;
#7091=STYLED_ITEM('',(#45169),#6132);
#7092 = FACE_OUTER_BOUND ( 'NONE', #36289, .T. ) ;
#7093 = CARTESIAN_POINT ( 'NONE',  ( 120.7947214775786193, -9.261995988541697145, -16.69588392320189030 ) ) ;
#7094 = CARTESIAN_POINT ( 'NONE',  ( 70.19189222814998175, -55.76308905022629858, -35.50805039322867884 ) ) ;
#7095 = EDGE_CURVE ( 'NONE', #23894, #3183, #23624, .T. ) ;
#7096 = CARTESIAN_POINT ( 'NONE',  ( 70.47992290675011873, 2.032776587329049978, -16.39321520033831447 ) ) ;
#7097 = CARTESIAN_POINT ( 'NONE',  ( 124.1983214775786166, -8.166667518702819706, -8.995218007635861213 ) ) ;
#7099 = CARTESIAN_POINT ( 'NONE',  ( 124.1415948109119540, -3.505236298600246325, -18.68346056562440793 ) ) ;
#7098 = CARTESIAN_POINT ( 'NONE',  ( 120.1707281442453166, 0.2603800115204892296, -16.42320221600525088 ) ) ;
#7100 = CARTESIAN_POINT ( 'NONE',  ( 121.7023481442452919, -0.8288870151387760510, -10.36305467784173118 ) ) ;
#7101 = CARTESIAN_POINT ( 'NONE',  ( 66.82415148905926117, -40.21211973637273474, -7.393215200338315363 ) ) ;
#7102 = CARTESIAN_POINT ( 'NONE',  ( 114.7816948109119863, 0.5811942927096154232, -14.16772938898807155 ) ) ;
#7103 = ORIENTED_EDGE ( 'NONE', *, *, #23332, .T. ) ;
#7104 = CARTESIAN_POINT ( 'NONE',  ( 71.02242295334774269, -99.02728775972636299, -55.91838671430374319 ) ) ;
#7105 = CARTESIAN_POINT ( 'NONE',  ( 114.8581140045248361, 0.1403307496149616695, -15.46607636864997204 ) ) ;
#7106 = CARTESIAN_POINT ( 'NONE',  ( 109.5102233795247884, -1.325403438956436419, -9.854619843455211026 ) ) ;
#7107 = CARTESIAN_POINT ( 'NONE',  ( 115.8999108795247821, -1.325403438956436419, -16.93181055722141792 ) ) ;
#7108 = CIRCLE ( 'NONE', #18764, 5.000000000000004441 ) ;
#7109 = CARTESIAN_POINT ( 'NONE',  ( 125.0386814775786490, -5.568102603701690967, -18.34339073538286513 ) ) ;
#7110 = CARTESIAN_POINT ( 'NONE',  ( 112.1155414775786454, 0.9020085738987339008, -11.91225656197089222 ) ) ;
#7111 = ORIENTED_EDGE ( 'NONE', *, *, #16975, .F. ) ;
#7112 = CARTESIAN_POINT ( 'NONE',  ( 113.4769814775786330, 0.4262465694468514643, -12.03445270309931736 ) ) ;
#7113 = CARTESIAN_POINT ( 'NONE',  ( 112.6356140045247827, -10.62599879583958717, -11.00651665394454604 ) ) ;
#7114 = CARTESIAN_POINT ( 'NONE',  ( 83.84865386347668448, -25.99489077589588604, -11.39321520033831447 ) ) ;
#7115 = CARTESIAN_POINT ( 'NONE',  ( 124.5954081442453116, -3.383040157471821630, -19.15922257007629170 ) ) ;
#7116 = CARTESIAN_POINT ( 'NONE',  ( 123.4608748109119745, -10.63000616557722466, -14.87417383870573495 ) ) ;
#7117 = CARTESIAN_POINT ( 'NONE',  ( 64.69189222814998175, -41.76310523276723785, -20.39321520033831447 ) ) ;
#7118 = CARTESIAN_POINT ( 'NONE',  ( 113.6471614775786492, -5.638512984488999180, -18.83840828888717311 ) ) ;
#7119 = CARTESIAN_POINT ( 'NONE',  ( 113.1912390045248031, 0.8980012041604421569, -15.77991374673208469 ) ) ;
#7120 = CARTESIAN_POINT ( 'NONE',  ( 105.8292077545248446, -7.250697342233347165, -7.631215200338321125 ) ) ;
#7121 = ORIENTED_EDGE ( 'NONE', *, *, #23071, .T. ) ;
#7122 = CARTESIAN_POINT ( 'NONE',  ( 124.7112241868944693, -2.239543233855045834, -18.13706010537467606 ) ) ;
#7123 = CARTESIAN_POINT ( 'NONE',  ( 115.3489614775786407, -0.8288870151387760510, -10.36305467784173118 ) ) ;
#7124 = CARTESIAN_POINT ( 'NONE',  ( 113.3068014775786594, -8.166667518702817929, -8.995218007635859436 ) ) ;
#7125 = CARTESIAN_POINT ( 'NONE',  ( 114.3024890045248156, 0.8980012041604421569, -15.77991374673208469 ) ) ;
#7126 = CARTESIAN_POINT ( 'NONE',  ( 106.7320983795247855, -8.402594152722688392, -16.93181055722141792 ) ) ;
#7127 = CARTESIAN_POINT ( 'NONE',  ( 122.0994348109119443, -10.15424416112533912, -14.75197769757731336 ) ) ;
#7128 = CARTESIAN_POINT ( 'NONE',  ( 118.0151148109119816, 0.4262465694468514643, -12.03445270309931736 ) ) ;
#7129 = CARTESIAN_POINT ( 'NONE',  ( 125.7299414775786346, 0.9020085738987339008, -11.91225656197089222 ) ) ;
#7130 = ORIENTED_EDGE ( 'NONE', *, *, #17537, .T. ) ;
#7131 = CARTESIAN_POINT ( 'NONE',  ( 125.2761281442453054, 0.4262465694468514643, -12.03445270309931736 ) ) ;
#7132 = CARTESIAN_POINT ( 'NONE',  ( 85.43169907558235820, -25.99489077589524300, -13.39321520033831625 ) ) ;
#7133 = CARTESIAN_POINT ( 'NONE',  ( 115.2922348109119781, 0.4262465694468514643, -12.03445270309931736 ) ) ;
#7134 = VERTEX_POINT ( 'NONE', #1271 ) ;
#7135 = FACE_OUTER_BOUND ( 'NONE', #8986, .T. ) ;
#7136 = CARTESIAN_POINT ( 'NONE',  ( 110.2742077545248094, -2.791137627527939813, -18.39754474579286025 ) ) ;
#7137 = EDGE_LOOP ( 'NONE', ( #29978, #27047, #17146, #43693, #27293, #42260 ) ) ;
#7138 = CARTESIAN_POINT ( 'NONE',  ( 117.2776681442452968, -4.153390946401321671, -8.397313243818183892 ) ) ;
#7139 = CARTESIAN_POINT ( 'NONE',  ( 114.1009748109119784, -5.574606645277164318, -18.38911715685844683 ) ) ;
#7140 = CARTESIAN_POINT ( 'NONE',  ( 78.69189222814998175, -62.82237896425675672, -47.71602681600972318 ) ) ;
#7141 = CARTESIAN_POINT ( 'NONE',  ( 121.6186891859119896, -8.844754642576884152, -8.592115655440050404 ) ) ;
#7142 = ORIENTED_EDGE ( 'NONE', *, *, #15130, .T. ) ;
#7143 = FACE_OUTER_BOUND ( 'NONE', #4827, .T. ) ;
#7144 = FACE_OUTER_BOUND ( 'NONE', #20978, .T. ) ;
#7145 = CARTESIAN_POINT ( 'NONE',  ( 116.5944421295247793, 0.8980012041604618078, -13.39321520033831447 ) ) ;
#7146 = CARTESIAN_POINT ( 'NONE',  ( 111.7184548109119788, -9.261995988541697145, -16.69588392320189030 ) ) ;
#7147 = CARTESIAN_POINT ( 'NONE',  ( 121.3619881442452879, -5.574606645277164318, -18.38911715685844683 ) ) ;
#7148 = CARTESIAN_POINT ( 'NONE',  ( 119.2631014775786298, -9.565557343593413364, -10.61323700422348004 ) ) ;
#7149 = CARTESIAN_POINT ( 'NONE',  ( 76.36356431740252049, -0.2843300395004543235, -14.39321520033831625 ) ) ;
#7150 = ORIENTED_EDGE ( 'NONE', *, *, #1973, .F. ) ;
#7151 = CARTESIAN_POINT ( 'NONE',  ( 115.8027748109119841, -8.899110576539710493, -16.42337572283490132 ) ) ;
#7152 = EDGE_CURVE ( 'NONE', #22218, #26016, #13680, .T. ) ;
#7153 = CARTESIAN_POINT ( 'NONE',  ( 125.7866681442452688, -8.899110576539710493, -16.42337572283490132 ) ) ;
#7154 = CARTESIAN_POINT ( 'NONE',  ( 125.1693226804736980, -1.293398517294378713, -16.89901338141164899 ) ) ;
#7155 = CARTESIAN_POINT ( 'NONE',  ( 96.46827370896536991, -25.85028767034691199, -12.39451169347363546 ) ) ;
#7156 = CARTESIAN_POINT ( 'NONE',  ( 114.7249681442453237, 0.2603800115204892296, -16.42320221600525088 ) ) ;
#7157 = ORIENTED_EDGE ( 'NONE', *, *, #20045, .F. ) ;
#7158 = CARTESIAN_POINT ( 'NONE',  ( 112.1722681442453222, -0.4660016031367893996, -10.09054647747474043 ) ) ;
#7159 = CARTESIAN_POINT ( 'NONE',  ( 114.6008271478583822, -3.807985514183293230, -19.09877912889401230 ) ) ;
#7160 = CARTESIAN_POINT ( 'NONE',  ( 111.8716296295247901, -4.863998795839590272, -19.15521520033831493 ) ) ;
#7161 = CARTESIAN_POINT ( 'NONE',  ( 126.4673881442452910, -7.894159318335828068, -9.358103419637847864 ) ) ;
#7162 = CARTESIAN_POINT ( 'NONE',  ( 114.2711548109119803, -9.988377603198976828, -10.36322818467138340 ) ) ;
#7163 = CARTESIAN_POINT ( 'NONE',  ( 123.6310548109119765, -4.153390946401325223, -8.397313243818185668 ) ) ;
#7164 = EDGE_CURVE ( 'NONE', #43250, #39978, #19253, .T. ) ;
#7165 = DIRECTION ( 'NONE',  ( 0.000000000000000000, -1.000000000000000000, 0.000000000000000000 ) ) ;
#7166 = CARTESIAN_POINT ( 'NONE',  ( 111.8716296295247901, -4.863998795839590272, -8.388885654883775800 ) ) ;
#7167 = CARTESIAN_POINT ( 'NONE',  ( 112.0044508535611527, -2.239543233855026738, -18.13706010537467606 ) ) ;
#7168 = CARTESIAN_POINT ( 'NONE',  ( 109.2294546431617306, -8.427163038048201216, -17.40843757233801270 ) ) ;
#7169 = CARTESIAN_POINT ( 'NONE',  ( 118.4689281442453392, -10.15424416112533912, -14.75197769757731336 ) ) ;
#7170 = DIRECTION ( 'NONE',  ( 0.000000000000000000, 0.000000000000000000, 1.000000000000000000 ) ) ;
#7171 = CIRCLE ( 'NONE', #39918, 2.999999999999999556 ) ;
#7172 = CARTESIAN_POINT ( 'NONE',  ( 122.4764302067644195, -1.223627541775709426, -16.99192386690442547 ) ) ;
#7173 = CARTESIAN_POINT ( 'NONE',  ( 107.7044421295247929, 0.8980012041604618078, -13.39321520033831447 ) ) ;
#7174 = CARTESIAN_POINT ( 'NONE',  ( 121.7527562859068837, -1.111561923218658210, -17.14115599315433158 ) ) ;
#7175 = CARTESIAN_POINT ( 'NONE',  ( 124.3117748109119844, -10.30919188438810075, -12.61870101168855918 ) ) ;
#7176 = FACE_OUTER_BOUND ( 'NONE', #35122, .T. ) ;
#7177 = CARTESIAN_POINT ( 'NONE',  ( 125.1059481442452750, -8.166667518702819706, -8.995218007635861213 ) ) ;
#7178 = CARTESIAN_POINT ( 'NONE',  ( 115.9162281442453235, -4.089484607189486809, -7.948022111789456723 ) ) ;
#7179 = VERTEX_POINT ( 'NONE', #3297 ) ;
#7180 = CARTESIAN_POINT ( 'NONE',  ( 113.7038881442453402, -6.222761293078241884, -8.102969835052219238 ) ) ;
#7181 = CARTESIAN_POINT ( 'NONE',  ( 111.8319081442453182, -5.638512984488999180, -18.83840828888717311 ) ) ;
#7182 = CARTESIAN_POINT ( 'NONE',  ( 116.1431348109119881, -10.30919188438810075, -12.61870101168855918 ) ) ;
#7183 = CARTESIAN_POINT ( 'NONE',  ( 116.8238548109119819, -5.574606645277164318, -18.38911715685844683 ) ) ;
#7184 = EDGE_LOOP ( 'NONE', ( #15252, #18459, #20537, #28291 ) ) ;
#7185 = EDGE_CURVE ( 'NONE', #35850, #22322, #20642, .T. ) ;
#7186 = CARTESIAN_POINT ( 'NONE',  ( 122.6667014775786413, -2.084020599724406786, -8.691656652584148546 ) ) ;
#7187 = EDGE_CURVE ( 'NONE', #2634, #17999, #5653, .T. ) ;
#7188 = EDGE_CURVE ( 'NONE', #33083, #44381, #23615, .T. ) ;
#7189 = CARTESIAN_POINT ( 'NONE',  ( 117.8449348109119938, -8.166667518702817929, -8.995218007635861213 ) ) ;
#7190 = CARTESIAN_POINT ( 'NONE',  ( 136.0105862893745439, 0.5780522297147454580, -15.71516581483972352 ) ) ;
#7191 = CARTESIAN_POINT ( 'NONE',  ( 112.7745202545247878, -10.62599879583958717, -15.77991374673208469 ) ) ;
#7192 = CARTESIAN_POINT ( 'NONE',  ( 114.6482964575754977, -1.016270020561755860, -17.26805140881366896 ) ) ;
#7193 = CARTESIAN_POINT ( 'NONE',  ( 126.3410021428612566, 0.1890319226722280144, -13.68675727894937388 ) ) ;
#7194 = CARTESIAN_POINT ( 'NONE',  ( 117.1500671295247713, 0.1403307496149613920, -13.39321520033831447 ) ) ;
#7195 = CARTESIAN_POINT ( 'NONE',  ( 113.3635281442453504, -9.988377603198976828, -10.36322818467138340 ) ) ;
#7196 = CARTESIAN_POINT ( 'NONE',  ( 136.9115742440160375, -10.37453544881151757, -13.81866509092029105 ) ) ;
#7197 = CARTESIAN_POINT ( 'NONE',  ( 113.4202548109119846, 0.1319031606808879209, -14.10382304977623669 ) ) ;
#7198 = CARTESIAN_POINT ( 'NONE',  ( 76.69189222814998175, -50.16718729050181480, -4.893215200338314474 ) ) ;
#7199 = CARTESIAN_POINT ( 'NONE',  ( 115.3602436215688414, -1.135392229370332462, -17.10942237759954665 ) ) ;
#7200 = CARTESIAN_POINT ( 'NONE',  ( 116.8028015045247940, -6.936859964151250502, -18.39754474579286025 ) ) ;
#7201 = CARTESIAN_POINT ( 'NONE',  ( 116.7104014775786425, -0.4660016031367893996, -10.09054647747474043 ) ) ;
#7202 = SURFACE_STYLE_USAGE ( .BOTH. , #35454 ) ;
#7203 = EDGE_CURVE ( 'NONE', #10687, #38595, #552, .T. ) ;
#7204 = FACE_OUTER_BOUND ( 'NONE', #38585, .T. ) ;
#7206 = CARTESIAN_POINT ( 'NONE',  ( 113.9307948109119906, 0.9020085738987339008, -11.91225656197089222 ) ) ;
#7205 = CARTESIAN_POINT ( 'NONE',  ( 70.19189222814998175, -66.47064387046886225, -39.79103499669764687 ) ) ;
#7207 = CARTESIAN_POINT ( 'NONE',  ( 124.5954081442453116, -6.222761293078241884, -8.102969835052219238 ) ) ;
#7208 = CARTESIAN_POINT ( 'NONE',  ( 119.5467348109119712, -5.574606645277164318, -18.38911715685844683 ) ) ;
#7209 = ORIENTED_EDGE ( 'NONE', *, *, #24743, .F. ) ;
#7210 = CARTESIAN_POINT ( 'NONE',  ( 122.1655659103642222, -8.454079026182057532, -17.47208793939445215 ) ) ;
#7211 = CARTESIAN_POINT ( 'NONE',  ( 122.2696148109119889, -4.089484607189486809, -7.948022111789456723 ) ) ;
#7212 = CARTESIAN_POINT ( 'NONE',  ( 116.4555358795247884, -8.402594152722688392, -9.854619843455216355 ) ) ;
#7213 = CARTESIAN_POINT ( 'NONE',  ( 114.5547881442453217, -4.153390946401321671, -8.397313243818183892 ) ) ;
#7214 = CARTESIAN_POINT ( 'NONE',  ( 114.4413348109119823, -0.8288870151387760510, -10.36305467784173118 ) ) ;
#7215 = EDGE_CURVE ( 'NONE', #39449, #10182, #44249, .T. ) ;
#7216 = CARTESIAN_POINT ( 'NONE',  ( 85.06881860370363313, -29.48994604112064621, -10.44326554851264888 ) ) ;
#7217 = CARTESIAN_POINT ( 'NONE',  ( 111.3160046295247838, -4.863998795839590272, -7.631215200338315796 ) ) ;
#7218 = CARTESIAN_POINT ( 'NONE',  ( 120.2841814775786276, -10.15424416112533912, -14.75197769757731336 ) ) ;
#7219 = CARTESIAN_POINT ( 'NONE',  ( 122.1561614775786353, -8.899110576539710493, -16.42337572283490132 ) ) ;
#7220 = CARTESIAN_POINT ( 'NONE',  ( 71.02242295334774269, -54.33197696945092758, -38.04041819808246316 ) ) ;
#7221 = CARTESIAN_POINT ( 'NONE',  ( 109.2294548365425015, -3.781108693792560871, -7.969886040473982192 ) ) ;
#7222 = DIRECTION ( 'NONE',  ( 1.000000000000000000, 0.000000000000000000, -0.000000000000000000 ) ) ;
#7223 = CARTESIAN_POINT ( 'NONE',  ( 109.5102233795247884, -1.325403438956436419, -9.854619843455211026 ) ) ;
#7224 = CARTESIAN_POINT ( 'NONE',  ( 117.1147479696649185, 1.569042602373198481, -21.39323033354518344 ) ) ;
#7225 = CARTESIAN_POINT ( 'NONE',  ( 118.4122014775786340, 0.5811942927096110934, -14.16772938898807510 ) ) ;
#7226 = CARTESIAN_POINT ( 'NONE',  ( 114.3846081442453197, -10.63000616557722466, -14.87417383870573495 ) ) ;
#7227 = CARTESIAN_POINT ( 'NONE',  ( 111.1770983795247787, -0.7896495226426338832, -9.318865927141430916 ) ) ;
#7228 = CARTESIAN_POINT ( 'NONE',  ( 70.36267391504958368, -5.685877709920885259, -7.393215200338315363 ) ) ;
#7229 = ORIENTED_EDGE ( 'NONE', *, *, #1232, .F. ) ;
#7230 = DIRECTION ( 'NONE',  ( 0.000000000000000000, -0.6004852223388320587, 0.7996358532186281787 ) ) ;
#7231 = CARTESIAN_POINT ( 'NONE',  ( 120.3976348109119812, -1.834011780172310813, -8.268836392978581529 ) ) ;
#7232 = CARTESIAN_POINT ( 'NONE',  ( 126.2404814775786264, -0.8288870151387760510, -10.36305467784173118 ) ) ;
#7233 = VECTOR ( 'NONE', #22939, 1000.000000000000000 ) ;
#7234 = CARTESIAN_POINT ( 'NONE',  ( 123.6310548109119765, -4.153390946401325223, -8.397313243818185668 ) ) ;
#7235 = PRESENTATION_STYLE_ASSIGNMENT (( #7453 ) ) ;
#7236 = CARTESIAN_POINT ( 'NONE',  ( 126.1837548109119211, -10.63000616557722466, -14.87417383870573495 ) ) ;
#7237 = CARTESIAN_POINT ( 'NONE',  ( 118.2987481442453088, -1.561330072975668504, -17.79121239304076951 ) ) ;
#7238 = ADVANCED_FACE ( 'NONE', ( #10377 ), #2616, .T. ) ;
#7239 = CARTESIAN_POINT ( 'NONE',  ( 107.4960827545248350, -6.936859964151250502, -8.388885654883777576 ) ) ;
#7240 = CARTESIAN_POINT ( 'NONE',  ( 115.8595014775786609, -7.643976991954077427, -18.09477374809248928 ) ) ;
#7241 = CARTESIAN_POINT ( 'NONE',  ( 117.2294421295247844, 7.836001204160461420, -12.14321520033831625 ) ) ;
#7242 = ORIENTED_EDGE ( 'NONE', *, *, #2511, .F. ) ;
#7243 = EDGE_CURVE ( 'NONE', #13898, #29623, #22391, .T. ) ;
#7244 =( BOUNDED_CURVE ( )  B_SPLINE_CURVE ( 3, ( #1330, #880, #25290, #39418 ),
 .UNSPECIFIED., .F., .T. ) 
 B_SPLINE_CURVE_WITH_KNOTS ( ( 4, 4 ),
 ( 1.570796326794896558, 1.618943030528138038 ),
 .UNSPECIFIED. ) 
 CURVE ( )  GEOMETRIC_REPRESENTATION_ITEM ( )  RATIONAL_B_SPLINE_CURVE ( ( 1.000000000000000000, 0.9998068339056410680, 0.9998068339056410680, 1.000000000000000000 ) ) 
 REPRESENTATION_ITEM ( '' )  );
#7245 = CARTESIAN_POINT ( 'NONE',  ( 119.8303681442453126, -10.63000616557722466, -14.87417383870573495 ) ) ;
#7246 = LINE ( 'NONE', #6588, #16969 ) ;
#7247 = CARTESIAN_POINT ( 'NONE',  ( 117.5045748109119756, 0.5811942927096110934, -14.16772938898807510 ) ) ;
#7248 = VERTEX_POINT ( 'NONE', #27258 ) ;
#7249 = CARTESIAN_POINT ( 'NONE',  ( 106.3153796295248412, -4.863998795839590272, -8.388885654883775800 ) ) ;
#7250 = CARTESIAN_POINT ( 'NONE',  ( 125.5597614775786326, -1.561330072975669392, -17.79121239304076951 ) ) ;
#7251 = CARTESIAN_POINT ( 'NONE',  ( 122.6667014775786413, -7.893985811506198047, -18.51759400769803676 ) ) ;
#7252 = CARTESIAN_POINT ( 'NONE',  ( 116.0296814775786345, -1.833838273342658809, -17.42832698103878286 ) ) ;
#7253 = FACE_OUTER_BOUND ( 'NONE', #14340, .T. ) ;
#7254 = CARTESIAN_POINT ( 'NONE',  ( 118.6391081442452986, -5.574606645277164318, -18.38911715685844683 ) ) ;
#7255 = CARTESIAN_POINT ( 'NONE',  ( 120.4744527483928920, -2.423081321603731908, -17.89265170041263175 ) ) ;
#7256 = CARTESIAN_POINT ( 'NONE',  ( 121.3619881442452879, -5.574606645277164318, -18.38911715685844683 ) ) ;
#7257 = AXIS2_PLACEMENT_3D ( 'NONE', #32020, #31799, #42082 ) ;
#7258 = CARTESIAN_POINT ( 'NONE',  ( 125.0532895624267553, -10.95664536207781659, -8.976081904060929872 ) ) ;
#7259 = CARTESIAN_POINT ( 'NONE',  ( 121.1918081442452859, -10.15424416112533912, -14.75197769757731336 ) ) ;
#7260 = CARTESIAN_POINT ( 'NONE',  ( 123.7717360609119623, -6.564341423271550902, -7.887810678476487425 ) ) ;
#7261 = CARTESIAN_POINT ( 'NONE',  ( 114.2711548109119803, -9.988377603198976828, -10.36322818467138340 ) ) ;
#7262 = CARTESIAN_POINT ( 'NONE',  ( 121.9484597424434043, -0.9924539043446216624, -17.29976612834909133 ) ) ;
#7263 = CARTESIAN_POINT ( 'NONE',  ( 121.8725281442453223, -6.222761293078241884, -8.102969835052219238 ) ) ;
#7264 = ORIENTED_EDGE ( 'NONE', *, *, #42709, .F. ) ;
#7265 = CARTESIAN_POINT ( 'NONE',  ( 116.8238548109119819, -4.089484607189486809, -7.948022111789456723 ) ) ;
#7266 = CARTESIAN_POINT ( 'NONE',  ( 106.4542858795248179, -0.7896495226426338832, -17.46756447353520159 ) ) ;
#7267 = CARTESIAN_POINT ( 'NONE',  ( 115.8027748109119841, -8.899110576539719375, -16.42337572283489067 ) ) ;
#7268 = CARTESIAN_POINT ( 'NONE',  ( 113.9094545411902857, -0.3595008806742185925, -10.82052240173742064 ) ) ;
#7269 = VECTOR ( 'NONE', #892, 1000.000000000000000 ) ;
#7270 = CARTESIAN_POINT ( 'NONE',  ( 121.5492360609119800, -3.387241619883789134, -18.17469012370384718 ) ) ;
#7271 = CARTESIAN_POINT ( 'NONE',  ( 123.2906948109119867, -8.166667518702819706, -8.995218007635861213 ) ) ;
#7272 = ORIENTED_EDGE ( 'NONE', *, *, #22839, .F. ) ;
#7273 = VECTOR ( 'NONE', #23552, 1000.000000000000000 ) ;
#7274 = CARTESIAN_POINT ( 'NONE',  ( 126.2455040230451004, -8.053725330373652014, -9.523658174356643968 ) ) ;
#7275 = CARTESIAN_POINT ( 'NONE',  ( 116.9373081442452929, -1.833838273342659253, -17.42832698103878286 ) ) ;
#7276 = CARTESIAN_POINT ( 'NONE',  ( 125.3134144568203681, -8.454919450556467098, -17.47367947343729710 ) ) ;
#7277 = CARTESIAN_POINT ( 'NONE',  ( 109.2781797178594019, -0.3595008806742686081, -15.96590799893915857 ) ) ;
#7278 = EDGE_CURVE ( 'NONE', #452, #24392, #2359, .T. ) ;
#7279 = CARTESIAN_POINT ( 'NONE',  ( 110.8298327545248299, -6.936859964151250502, -8.388885654883777576 ) ) ;
#7280 = DIRECTION ( 'NONE',  ( 0.000000000000000000, 1.069961080215129965E-32, -1.000000000000000000 ) ) ;
#7281 = ORIENTED_EDGE ( 'NONE', *, *, #18105, .F. ) ;
#7282 = CARTESIAN_POINT ( 'NONE',  ( 115.0086014775786509, -4.089484607189486809, -7.948022111789456723 ) ) ;
#7283 = CARTESIAN_POINT ( 'NONE',  ( 112.9097148109120070, 0.2603800115204892296, -16.42320221600525088 ) ) ;
#7284 = CARTESIAN_POINT ( 'NONE',  ( 121.9292548109119849, -1.561330072975668948, -17.79121239304076951 ) ) ;
#7285 = CARTESIAN_POINT ( 'NONE',  ( 116.8238548109119819, -5.574606645277164318, -18.38911715685844683 ) ) ;
#7286 = DIRECTION ( 'NONE',  ( -1.000000000000000000, 0.000000000000000000, -0.000000000000000000 ) ) ;
#7287 = CARTESIAN_POINT ( 'NONE',  ( 119.6601881442453106, -8.166667518702819706, -8.995218007635861213 ) ) ;
#7288 = CARTESIAN_POINT ( 'NONE',  ( 111.3886348109119808, -3.517672760959766887, -18.63504008191830508 ) ) ;
#7289 = CARTESIAN_POINT ( 'NONE',  ( 67.84197459855160162, -59.22556289356354142, -37.62220087706567284 ) ) ;
#7290 = CARTESIAN_POINT ( 'NONE',  ( 88.73939138327467901, -25.99489077589524300, -13.39321520033831625 ) ) ;
#7291 = CARTESIAN_POINT ( 'NONE',  ( 121.6456214775786293, 0.4262465694468514643, -12.03445270309931736 ) ) ;
#7292 = ORIENTED_EDGE ( 'NONE', *, *, #25608, .T. ) ;
#7293 = CARTESIAN_POINT ( 'NONE',  ( 1093.930577029472943, -25.99489077589524300, -13.39321520033831447 ) ) ;
#7294 = CIRCLE ( 'NONE', #8021, 1.610000000000000986 ) ;
#7295 = CARTESIAN_POINT ( 'NONE',  ( 116.3133148109119759, -7.893985811506177619, -18.51759400769804742 ) ) ;
#7296 = CARTESIAN_POINT ( 'NONE',  ( 123.5176014775786228, -0.8288870151387760510, -10.36305467784173118 ) ) ;
#7297 = VERTEX_POINT ( 'NONE', #23382 ) ;
#7298 = CARTESIAN_POINT ( 'NONE',  ( 112.4559014775786494, -9.988377603198976828, -10.36322818467138340 ) ) ;
#7299 = CARTESIAN_POINT ( 'NONE',  ( 122.0994348109119443, 0.9020085738987339008, -11.91225656197089222 ) ) ;
#7300 = CARTESIAN_POINT ( 'NONE',  ( 106.6626452545248611, 0.8980012041604421569, -11.00651665394454071 ) ) ;
#7301 = CARTESIAN_POINT ( 'NONE',  ( 121.3619881442452879, -5.574606645277164318, -18.38911715685844683 ) ) ;
#7302 = EDGE_LOOP ( 'NONE', ( #28989, #43092, #18629, #40157, #10590 ) ) ;
#7303 = CONICAL_SURFACE ( 'NONE', #33484, 2.445500000000005336, 0.9599310885968757034 ) ;
#7304 = CARTESIAN_POINT ( 'NONE',  ( 115.0653281442453277, -6.344957434206662583, -7.627207830600332805 ) ) ;
#7305 = CARTESIAN_POINT ( 'NONE',  ( 123.7445081442452874, -7.894159318335828068, -9.358103419637847864 ) ) ;
#7306 = CARTESIAN_POINT ( 'NONE',  ( 79.40485529179196078, 5.048385126289187674, -20.47678328014367821 ) ) ;
#7307 = CYLINDRICAL_SURFACE ( 'NONE', #6153, 1.200000000000000622 ) ;
#7308 = CARTESIAN_POINT ( 'NONE',  ( 123.9714148109119805, -0.4660016031367893996, -10.09054647747474043 ) ) ;
#7309 = DIRECTION ( 'NONE',  ( -0.9908103287288504424, 0.1352586133457950035, 0.000000000000000000 ) ) ;
#7310 = CARTESIAN_POINT ( 'NONE',  ( 135.3184548109119874, -10.81584935473217080, -14.15181583611863303 ) ) ;
#7311 = CARTESIAN_POINT ( 'NONE',  ( 122.1561614775786353, -0.4660016031367893996, -10.09054647747474043 ) ) ;
#7313 = CARTESIAN_POINT ( 'NONE',  ( 122.9503348109119827, -9.859900752359378018, -12.68260735090039759 ) ) ;
#7312 = CARTESIAN_POINT ( 'NONE',  ( 121.2485348109119769, -0.4660016031367893996, -10.09054647747474043 ) ) ;
#7314 = CARTESIAN_POINT ( 'NONE',  ( 120.9081748109119872, -4.153390946401325223, -8.397313243818185668 ) ) ;
#7315 = CARTESIAN_POINT ( 'NONE',  ( 125.2205968368549946, -0.1451374939622062654, -15.72356508888822191 ) ) ;
#7316 = CARTESIAN_POINT ( 'NONE',  ( 116.1431348109119881, -10.30919188438810075, -12.61870101168855918 ) ) ;
#7317 = ORIENTED_EDGE ( 'NONE', *, *, #40378, .F. ) ;
#7318 = CARTESIAN_POINT ( 'NONE',  ( 125.3895814775786590, -2.084020599725330491, -8.691656652583604981 ) ) ;
#7319 = CARTESIAN_POINT ( 'NONE',  ( 115.4831921295247952, -9.868328341294093420, -13.39321520033831447 ) ) ;
#7320 = CARTESIAN_POINT ( 'NONE',  ( 110.9687390045248350, -9.868328341294098749, -11.32035403202665869 ) ) ;
#7321 = CARTESIAN_POINT ( 'NONE',  ( 112.2883483795247770, -8.402594152722688392, -16.93181055722141792 ) ) ;
#7322 = CIRCLE ( 'NONE', #25562, 4.500000000000003553 ) ;
#7323 = CARTESIAN_POINT ( 'NONE',  ( 124.8790414775786246, -0.4660016031367893996, -10.09054647747474043 ) ) ;
#7324 = CARTESIAN_POINT ( 'NONE',  ( 125.1626748109119802, -0.1624402480850797581, -16.17319339645315424 ) ) ;
#7325 =( BOUNDED_CURVE ( )  B_SPLINE_CURVE ( 3, ( #1744, #39612, #8600, #15896 ),
 .UNSPECIFIED., .F., .T. ) 
 B_SPLINE_CURVE_WITH_KNOTS ( ( 4, 4 ),
 ( 2.617993877991494855, 4.712388980384689674 ),
 .UNSPECIFIED. ) 
 CURVE ( )  GEOMETRIC_REPRESENTATION_ITEM ( )  RATIONAL_B_SPLINE_CURVE ( ( 1.000000000000000000, 0.6666666666666670737, 0.6666666666666670737, 1.000000000000000000 ) ) 
 REPRESENTATION_ITEM ( '' )  );
#7326 = ORIENTED_EDGE ( 'NONE', *, *, #9969, .F. ) ;
#7327 = CARTESIAN_POINT ( 'NONE',  ( 111.7751814775786556, -2.084020599724406786, -8.691656652584148546 ) ) ;
#7328 = CARTESIAN_POINT ( 'NONE',  ( 113.3301452545248083, 0.8980012041604421569, -11.00651665394454071 ) ) ;
#7329 = LINE ( 'NONE', #21248, #32135 ) ;
#7330 = CARTESIAN_POINT ( 'NONE',  ( 123.1205148109119563, -1.834011780172310813, -8.268836392978581529 ) ) ;
#7331 = CARTESIAN_POINT ( 'NONE',  ( 125.7299414775786346, 0.9020085738987339008, -11.91225656197089222 ) ) ;
#7332 = FACE_OUTER_BOUND ( 'NONE', #29233, .T. ) ;
#7333 = CARTESIAN_POINT ( 'NONE',  ( 114.8951481442453115, -0.4660016031367893996, -10.09054647747474043 ) ) ;
#7334 = CARTESIAN_POINT ( 'NONE',  ( 112.7745202545247878, -10.62599879583958717, -15.77991374673208469 ) ) ;
#7335 = CARTESIAN_POINT ( 'NONE',  ( 115.7610046295247912, -4.863998795839590272, -18.39754474579285315 ) ) ;
#7336 = ORIENTED_EDGE ( 'NONE', *, *, #11969, .T. ) ;
#7337 = FACE_OUTER_BOUND ( 'NONE', #40602, .T. ) ;
#7338 = CONICAL_SURFACE ( 'NONE', #8770, 1.610000000000000986, 0.9599310885968765916 ) ;
#7339 = CARTESIAN_POINT ( 'NONE',  ( 113.7606148109119886, -7.894159318335828068, -9.358103419637847864 ) ) ;
#7340 = CARTESIAN_POINT ( 'NONE',  ( 126.6375681442452930, -10.15424416112533912, -14.75197769757731336 ) ) ;
#7341 = CARTESIAN_POINT ( 'NONE',  ( 114.5108483795247878, -0.7896495226426338832, -9.318865927141430916 ) ) ;
#7342 = CARTESIAN_POINT ( 'NONE',  ( 104.9263171295248327, 0.1403307496149613920, -13.39321520033831447 ) ) ;
#7343 = AXIS2_PLACEMENT_3D ( 'NONE', #44879, #20702, #19618 ) ;
#7344 = CARTESIAN_POINT ( 'NONE',  ( 122.6667014775786413, -2.084020599724406786, -8.691656652584148546 ) ) ;
#7345 = UNCERTAINTY_MEASURE_WITH_UNIT (LENGTH_MEASURE( 1.000000000000000082E-05 ), #8867, 'distance_accuracy_value', 'NONE');
#7346 = CARTESIAN_POINT ( 'NONE',  ( 120.5110881442453206, -3.505236298600246325, -18.68346056562440793 ) ) ;
#7347 = CARTESIAN_POINT ( 'NONE',  ( 112.7962614775786676, -6.222761293078241884, -8.102969835052219238 ) ) ;
#7348 = ORIENTED_EDGE ( 'NONE', *, *, #32913, .T. ) ;
#7349 = CARTESIAN_POINT ( 'NONE',  ( 121.5492360609119800, -3.387241619883791355, -18.17469012370385073 ) ) ;
#7350 = ADVANCED_FACE ( 'NONE', ( #19958 ), #6504, .F. ) ;
#7351 = FACE_OUTER_BOUND ( 'NONE', #8877, .T. ) ;
#7352 = CARTESIAN_POINT ( 'NONE',  ( 115.5191414775786569, -6.222761293078241884, -8.102969835052219238 ) ) ;
#7353 = EDGE_LOOP ( 'NONE', ( #45122, #29834, #37218, #10005 ) ) ;
#7354 = CARTESIAN_POINT ( 'NONE',  ( 70.19189222814998175, -58.90901798090458641, -36.76641099935233825 ) ) ;
#7355 = CARTESIAN_POINT ( 'NONE',  ( 105.6903015045248253, -2.477300249445798297, -7.631215200338321125 ) ) ;
#7356 = CARTESIAN_POINT ( 'NONE',  ( 109.4407702545248355, 0.1403307496149616695, -11.32035403202665336 ) ) ;
#7357 = ORIENTED_EDGE ( 'NONE', *, *, #22236, .T. ) ;
#7358 = VECTOR ( 'NONE', #4292, 1000.000000000000000 ) ;
#7359 = CARTESIAN_POINT ( 'NONE',  ( 119.8870948109119752, -0.8288870151387760510, -10.36305467784173118 ) ) ;
#7360 = CARTESIAN_POINT ( 'NONE',  ( 114.5547881442453217, -4.153390946401321671, -8.397313243818183892 ) ) ;
#7361 = CARTESIAN_POINT ( 'NONE',  ( 124.5827871365980144, -9.800012535114518641, -14.21035762377393041 ) ) ;
#7362 = CARTESIAN_POINT ( 'NONE',  ( 116.5026997424434114, -0.9924539043446216624, -17.29976612834909133 ) ) ;
#7363 = VERTEX_POINT ( 'NONE', #3075 ) ;
#7364 = CARTESIAN_POINT ( 'NONE',  ( 86.36631847702263087, -26.75858941326842810, -11.54476601486570964 ) ) ;
#7365 = CARTESIAN_POINT ( 'NONE',  ( 125.2512653913828728, -0.8349821636219845189, -7.351438796280286070 ) ) ;
#7366 = CARTESIAN_POINT ( 'NONE',  ( 115.4831921295247952, 0.8980012041604618078, -13.39321520033831447 ) ) ;
#7367 = VECTOR ( 'NONE', #21424, 1000.000000000000000 ) ;
#7368 = CARTESIAN_POINT ( 'NONE',  ( 112.1155414775786454, 0.9020085738987339008, -11.91225656197089222 ) ) ;
#7369 = CARTESIAN_POINT ( 'NONE',  ( 113.0798948109119948, -0.4660016031367893996, -10.09054647747474043 ) ) ;
#7370 = CARTESIAN_POINT ( 'NONE',  ( 117.2209414775786485, -2.084020599724406786, -8.691656652584148546 ) ) ;
#7371 = CARTESIAN_POINT ( 'NONE',  ( 114.1934435773848833, -2.467220198592768199, -17.83387418641523325 ) ) ;
#7372 = ORIENTED_EDGE ( 'NONE', *, *, #21874, .F. ) ;
#7373 = CARTESIAN_POINT ( 'NONE',  ( 117.1642148109119859, -0.8288870151387760510, -10.36305467784173118 ) ) ;
#7374 = CARTESIAN_POINT ( 'NONE',  ( 119.7434548109119703, -0.7361556930925071685, -10.35768125360512393 ) ) ;
#7375 = CARTESIAN_POINT ( 'NONE',  ( 64.22513517183551812, -35.03390339818633947, -5.893215200338315363 ) ) ;
#7376 = CARTESIAN_POINT ( 'NONE',  ( 116.7226334719562288, -1.125321370491268125, -17.12283323191015327 ) ) ;
#7377 = CARTESIAN_POINT ( 'NONE',  ( 115.2922348109119781, -10.63000616557722466, -14.87417383870573495 ) ) ;
#7378 = ORIENTED_EDGE ( 'NONE', *, *, #44007, .F. ) ;
#7379 = CARTESIAN_POINT ( 'NONE',  ( 117.3343948109119737, -3.383040157471821630, -19.15922257007629170 ) ) ;
#7380 = CARTESIAN_POINT ( 'NONE',  ( 109.7884337908067920, 0.5115630086001619059, -12.14321520033828072 ) ) ;
#7381 = CARTESIAN_POINT ( 'NONE',  ( 112.0799890045248475, 0.8980012041604421569, -15.77991374673208469 ) ) ;
#7382 = CARTESIAN_POINT ( 'NONE',  ( 113.8173414775786512, 0.2603800115204892296, -16.42320221600525088 ) ) ;
#7383 = CARTESIAN_POINT ( 'NONE',  ( 114.1577014775786552, -6.344957434206662583, -7.627207830600332805 ) ) ;
#7384 = CARTESIAN_POINT ( 'NONE',  ( 124.8223148109119762, -10.15424416112533912, -14.75197769757731336 ) ) ;
#7385 = LINE ( 'NONE', #42736, #32959 ) ;
#7386 = CARTESIAN_POINT ( 'NONE',  ( 111.7327233795247849, -1.325403438956436419, -9.854619843455211026 ) ) ;
#7387 = ORIENTED_EDGE ( 'NONE', *, *, #36889, .T. ) ;
#7388 = CARTESIAN_POINT ( 'NONE',  ( 112.3781902440515665, -2.467220198592768199, -17.83387418641523325 ) ) ;
#7389 = CARTESIAN_POINT ( 'NONE',  ( 109.2295392859521570, -8.890170852696687831, -16.98076245472113044 ) ) ;
#7390 = VECTOR ( 'NONE', #19709, 1000.000000000000000 ) ;
#7391 = CARTESIAN_POINT ( 'NONE',  ( 116.7104014775786425, -8.899110576539710493, -16.42337572283490132 ) ) ;
#7392 = DIRECTION ( 'NONE',  ( 0.000000000000000000, -0.4669533266896290225, -0.8842819633428516957 ) ) ;
#7393 = CARTESIAN_POINT ( 'NONE',  ( 115.8999108795247821, -1.325403438956436419, -16.93181055722141792 ) ) ;
#7394 = CARTESIAN_POINT ( 'NONE',  ( 110.8992858795247827, -0.7896495226426338832, -17.46756447353520159 ) ) ;
#7395 = CARTESIAN_POINT ( 'NONE',  ( 126.4536383592472788, -4.720982958058952406, -8.277426756250068962 ) ) ;
#7396 = CARTESIAN_POINT ( 'NONE',  ( 124.6521348109119884, -1.561330072975668948, -17.79121239304076951 ) ) ;
#7397 = CARTESIAN_POINT ( 'NONE',  ( 136.1067208867421243, 0.9922915268929951571, -12.69116158526661842 ) ) ;
#7398 = CARTESIAN_POINT ( 'NONE',  ( 122.7801548109119665, -3.383040157471821630, -19.15922257007629170 ) ) ;
#7399 = CARTESIAN_POINT ( 'NONE',  ( 116.8805814775786445, -6.344957434206662583, -7.627207830600332805 ) ) ;
#7400 = ORIENTED_EDGE ( 'NONE', *, *, #37934, .T. ) ;
#7401 = CARTESIAN_POINT ( 'NONE',  ( 115.8027748109119841, -8.899110576539710493, -16.42337572283490132 ) ) ;
#7402 = CARTESIAN_POINT ( 'NONE',  ( 125.8433948109119456, -1.834011780172310813, -8.268836392978581529 ) ) ;
#7403 = CARTESIAN_POINT ( 'NONE',  ( 118.9227414775786400, -10.63000616557722466, -14.87417383870573495 ) ) ;
#7404 = CARTESIAN_POINT ( 'NONE',  ( 117.9583881442453048, 0.1319031606808879209, -14.10382304977623669 ) ) ;
#7405 = VERTEX_POINT ( 'NONE', #27030 ) ;
#7406 = CARTESIAN_POINT ( 'NONE',  ( 119.6601881442453106, -1.833838273342659253, -17.42832698103878286 ) ) ;
#7407 = CARTESIAN_POINT ( 'NONE',  ( 115.6893214775786447, 0.5811942927096154232, -14.16772938898807155 ) ) ;
#7408 = CARTESIAN_POINT ( 'NONE',  ( 136.7937340014177607, 0.7122096995249440621, -12.90670490570438567 ) ) ;
#7409 = CARTESIAN_POINT ( 'NONE',  ( 110.8298327545248299, -2.477300249445798297, -19.15521520033831138 ) ) ;
#7410 = CARTESIAN_POINT ( 'NONE',  ( 63.44904766417841557, -14.80807631840853134, -9.881358851643950558 ) ) ;
#7411 = CARTESIAN_POINT ( 'NONE',  ( 126.2769959775738897, 0.1476450766692196659, -13.81407022109413241 ) ) ;
#7412 = CARTESIAN_POINT ( 'NONE',  ( 116.7333483795247844, -8.402594152722688392, -16.93181055722141792 ) ) ;
#7413 = CARTESIAN_POINT ( 'NONE',  ( 116.0296814775786345, -8.166667518702817929, -8.995218007635861213 ) ) ;
#7414 = FACE_OUTER_BOUND ( 'NONE', #34440, .T. ) ;
#7415 = DIRECTION ( 'NONE',  ( 0.9908103287288504424, -0.1352586133457950590, -0.000000000000000000 ) ) ;
#7416 = CARTESIAN_POINT ( 'NONE',  ( 88.19154317003298615, -15.02898452507898241, -18.64321520033831803 ) ) ;
#7417 = CARTESIAN_POINT ( 'NONE',  ( 112.6586338361194919, 0.1075849324168598464, -12.14321520033831625 ) ) ;
#7418 = CARTESIAN_POINT ( 'NONE',  ( 115.8999108795247821, -1.325403438956436419, -16.93181055722141792 ) ) ;
#7419 = CARTESIAN_POINT ( 'NONE',  ( 113.9307948109119764, -10.15424416112533912, -14.75197769757731336 ) ) ;
#7420 = DIRECTION ( 'NONE',  ( -1.000000000000000000, 0.000000000000000000, 0.000000000000000000 ) ) ;
#7421 = DIRECTION ( 'NONE',  ( -0.5735764363510450492, -0.3127926500124816878, 0.7570804645221038687 ) ) ;
#7423 = CARTESIAN_POINT ( 'NONE',  ( 116.1998614775786507, -10.63000616557722466, -14.87417383870573495 ) ) ;
#7422 = CARTESIAN_POINT ( 'NONE',  ( 118.3179530757767566, -0.9924539043446216624, -17.29976612834909133 ) ) ;
#7424 = CARTESIAN_POINT ( 'NONE',  ( 123.5743281442453139, -2.084020599724406786, -8.691656652584148546 ) ) ;
#7425 = CARTESIAN_POINT ( 'NONE',  ( 118.9794681442453026, -0.8288870151387760510, -10.36305467784173118 ) ) ;
#7426 = ORIENTED_EDGE ( 'NONE', *, *, #33987, .T. ) ;
#7427 = CARTESIAN_POINT ( 'NONE',  ( 136.8192643132362605, -7.130015825163922294, -8.292408517671104207 ) ) ;
#7428 = CARTESIAN_POINT ( 'NONE',  ( 123.2339681442453241, -6.344957434206665248, -7.627207830600338134 ) ) ;
#7429 = CARTESIAN_POINT ( 'NONE',  ( 114.9275671295247889, 0.1403307496149613920, -13.39321520033831447 ) ) ;
#7430 = CARTESIAN_POINT ( 'NONE',  ( 120.6812681442452941, 0.1319031606808879209, -14.10382304977623669 ) ) ;
#7431 = EDGE_CURVE ( 'NONE', #27006, #8254, #7952, .T. ) ;
#7432 = CARTESIAN_POINT ( 'NONE',  ( 111.2646414775786496, -8.899110576539710493, -16.42337572283490132 ) ) ;
#7433 = CARTESIAN_POINT ( 'NONE',  ( 86.21853402767062846, -26.70494960632584736, -8.456736516205184628 ) ) ;
#7434 = CARTESIAN_POINT ( 'NONE',  ( 111.8021765045248372, -7.250697342233347165, -19.15521520033831138 ) ) ;
#7435 = CARTESIAN_POINT ( 'NONE',  ( 120.3409081442453044, -8.899110576539710493, -16.42337572283490132 ) ) ;
#7436 = CARTESIAN_POINT ( 'NONE',  ( 120.9081748109119872, -4.153390946401325223, -8.397313243818185668 ) ) ;
#7437 = FACE_OUTER_BOUND ( 'NONE', #31671, .T. ) ;
#7438 = CARTESIAN_POINT ( 'NONE',  ( 109.2294421276549912, -0.9135388418710063130, -9.738026583846760786 ) ) ;
#7439 = CARTESIAN_POINT ( 'NONE',  ( 120.9936110609119737, -3.163656168406935087, -18.89861972220014508 ) ) ;
#7440 = CARTESIAN_POINT ( 'NONE',  ( 109.3713171295247832, 0.1403307496149613920, -13.39321520033831447 ) ) ;
#7441 = EDGE_CURVE ( 'NONE', #452, #8883, #9524, .T. ) ;
#7442 = LINE ( 'NONE', #7674, #1469 ) ;
#7443 = CARTESIAN_POINT ( 'NONE',  ( 119.0929214775786278, -5.638512984488999180, -18.83840828888717311 ) ) ;
#7444 = CARTESIAN_POINT ( 'NONE',  ( 115.9729548109119861, -6.344957434206662583, -7.627207830600332805 ) ) ;
#7445 = CARTESIAN_POINT ( 'NONE',  ( 109.2324108795247923, -8.938348069036489818, -9.318865927141430916 ) ) ;
#7446 = CARTESIAN_POINT ( 'NONE',  ( 113.5337081442453240, -9.261995988541697145, -16.69588392320189030 ) ) ;
#7447 = EDGE_LOOP ( 'NONE', ( #14154, #725, #44532, #17357, #44036 ) ) ;
#7448 = CARTESIAN_POINT ( 'NONE',  ( 92.04708369096698561, -25.99489077589524300, -13.39321520033831625 ) ) ;
#7449 = AXIS2_PLACEMENT_3D ( 'NONE', #23520, #5943, #30350 ) ;
#7450 = CARTESIAN_POINT ( 'NONE',  ( 123.2906948109119867, -8.166667518702819706, -8.995218007635861213 ) ) ;
#7451 = CARTESIAN_POINT ( 'NONE',  ( 116.4834948109119779, -1.561330072975668504, -17.79121239304076951 ) ) ;
#7452 = CARTESIAN_POINT ( 'NONE',  ( 121.8158014775786171, -4.153390946401325223, -8.397313243818185668 ) ) ;
#7453 = SURFACE_STYLE_USAGE ( .BOTH. , #6807 ) ;
#7454 = CARTESIAN_POINT ( 'NONE',  ( 125.9568481442452850, -6.344957434206665248, -7.627207830600338134 ) ) ;
#7455 = CARTESIAN_POINT ( 'NONE',  ( 120.8514481442452961, -7.893985811506177619, -18.51759400769804742 ) ) ;
#7456 = EDGE_CURVE ( 'NONE', #20884, #40668, #321, .T. ) ;
#7457 = CARTESIAN_POINT ( 'NONE',  ( 114.4413952545248350, 0.8980012041604421569, -11.00651665394454071 ) ) ;
#7458 = AXIS2_PLACEMENT_3D ( 'NONE', #39410, #8399, #39636 ) ;
#7459 = CARTESIAN_POINT ( 'NONE',  ( 117.3343948109119737, -6.222761293078241884, -8.102969835052219238 ) ) ;
#7460 = DIRECTION ( 'NONE',  ( 0.000000000000000000, -0.3818493186865927203, 0.9242245927363029745 ) ) ;
#7461 = ORIENTED_EDGE ( 'NONE', *, *, #45120, .T. ) ;
#7462 = CARTESIAN_POINT ( 'NONE',  ( 123.2339681442453241, -6.344957434206665248, -7.627207830600338134 ) ) ;
#7463 = EDGE_CURVE ( 'NONE', #735, #12514, #14459, .T. ) ;
#7464 = CARTESIAN_POINT ( 'NONE',  ( 123.1466579359119891, -5.444069387712269226, -19.60292469916370450 ) ) ;
#7465 = EDGE_CURVE ( 'NONE', #7697, #17646, #20380, .T. ) ;
#7466 = CARTESIAN_POINT ( 'NONE',  ( 120.6245414775786458, -9.988377603198976828, -10.36322818467138340 ) ) ;
#7467 = EDGE_LOOP ( 'NONE', ( #42947, #15317, #19668, #15546, #13937 ) ) ;
#7468 = CARTESIAN_POINT ( 'NONE',  ( 106.0375671295248310, 0.1403307496149613920, -13.39321520033831447 ) ) ;
#7469 = CARTESIAN_POINT ( 'NONE',  ( 123.6310548109119765, -5.638512984488999180, -18.83840828888717311 ) ) ;
#7470 = CARTESIAN_POINT ( 'NONE',  ( 119.7570243147880404, -2.395992375830759524, -17.92872468182853396 ) ) ;
#7471 = CARTESIAN_POINT ( 'NONE',  ( 116.7671281442453335, -7.643976991954077427, -18.09477374809248928 ) ) ;
#7472 = CARTESIAN_POINT ( 'NONE',  ( 124.3305360609119816, -6.339478340643663223, -8.615877017535705562 ) ) ;
#7473 = CARTESIAN_POINT ( 'NONE',  ( 118.7525614775786380, -1.833838273342659253, -17.42832698103878286 ) ) ;
#7474 = CARTESIAN_POINT ( 'NONE',  ( 86.09323753712084226, -25.99489077589524300, -13.39321520033831625 ) ) ;
#7475 = EDGE_CURVE ( 'NONE', #34675, #36736, #5667, .T. ) ;
#7476 = CARTESIAN_POINT ( 'NONE',  ( 123.1772414775786189, -5.574606645277164318, -18.38911715685844683 ) ) ;
#7477 = AXIS2_PLACEMENT_3D ( 'NONE', #38844, #14916, #35414 ) ;
#7478 = FACE_OUTER_BOUND ( 'NONE', #39647, .T. ) ;
#7479 = CARTESIAN_POINT ( 'NONE',  ( 118.9794681442453026, -0.8288870151387760510, -10.36305467784173118 ) ) ;
#7480 = EDGE_CURVE ( 'NONE', #11473, #26016, #17879, .T. ) ;
#7481 = CARTESIAN_POINT ( 'NONE',  ( 124.0495485609119584, -10.36940331770106916, -15.09355782777062061 ) ) ;
#7482 = CARTESIAN_POINT ( 'NONE',  ( 116.5402214775786405, 0.2603800115204892296, -16.42320221600525088 ) ) ;
#7483 = CARTESIAN_POINT ( 'NONE',  ( 113.0798948109119948, -0.4660016031367893996, -10.09054647747474043 ) ) ;
#7484 = CARTESIAN_POINT ( 'NONE',  ( 88.28425963449632263, -11.60945497031996787, -13.24321520033830879 ) ) ;
#7485 = EDGE_CURVE ( 'NONE', #30859, #16407, #20343, .T. ) ;
#7486 = EDGE_CURVE ( 'NONE', #28223, #31466, #21748, .T. ) ;
#7487 = CARTESIAN_POINT ( 'NONE',  ( 120.0005481442453146, -4.153390946401325223, -8.397313243818185668 ) ) ;
#7488 = VERTEX_POINT ( 'NONE', #3517 ) ;
#7489 = CARTESIAN_POINT ( 'NONE',  ( 115.8595014775786609, -1.834011780172310813, -8.268836392978581529 ) ) ;
#7490 = CARTESIAN_POINT ( 'NONE',  ( 112.2883483795247770, -8.402594152722688392, -16.93181055722141792 ) ) ;
#7491 = CARTESIAN_POINT ( 'NONE',  ( 70.19189222814998175, -60.76597359474132531, -37.50918677187066663 ) ) ;
#7492 = VECTOR ( 'NONE', #44625, 1000.000000000000114 ) ;
#7493 = DIRECTION ( 'NONE',  ( 0.1352586133457952255, 0.9908103287288504424, 0.000000000000000000 ) ) ;
#7494 = CARTESIAN_POINT ( 'NONE',  ( 61.69189222814998175, -63.77884951796256274, -31.62409037935697143 ) ) ;
#7495 = CARTESIAN_POINT ( 'NONE',  ( 122.8936081442453059, 0.2603800115204892296, -16.42320221600525088 ) ) ;
#7496 = ORIENTED_EDGE ( 'NONE', *, *, #30687, .T. ) ;
#7497 = DIRECTION ( 'NONE',  ( 0.000000000000000000, 0.9284778069183720062, 0.3713878862591650232 ) ) ;
#7498 = CARTESIAN_POINT ( 'NONE',  ( 121.8725281442453223, -6.222761293078241884, -8.102969835052219238 ) ) ;
#7499 = CARTESIAN_POINT ( 'NONE',  ( 120.7852516859119731, -9.665098340737509730, -17.37397104707595474 ) ) ;
#7500 = CARTESIAN_POINT ( 'NONE',  ( 65.58061229095905276, -14.25342924908086673, -17.12691776711527325 ) ) ;
#7501 = LINE ( 'NONE', #4756, #39197 ) ;
#7502 = CARTESIAN_POINT ( 'NONE',  ( 109.9963952545248134, -9.868328341294098749, -15.46607636864997204 ) ) ;
#7503 = CARTESIAN_POINT ( 'NONE',  ( 85.83930302032700865, -9.140269361470602760, -13.24321520033831412 ) ) ;
#7504 = ORIENTED_EDGE ( 'NONE', *, *, #40126, .F. ) ;
#7505 = CARTESIAN_POINT ( 'NONE',  ( 116.3133148109119759, -7.893985811506177619, -18.51759400769804742 ) ) ;
#7506 = CARTESIAN_POINT ( 'NONE',  ( 125.2761281442453054, 0.4262465694468514643, -12.03445270309931736 ) ) ;
#7507 = CARTESIAN_POINT ( 'NONE',  ( 124.1415948109119540, -6.344957434206665248, -7.627207830600338134 ) ) ;
#7508 = CARTESIAN_POINT ( 'NONE',  ( 121.6456214775786293, 0.4262465694468514643, -12.03445270309931736 ) ) ;
#7509 = CARTESIAN_POINT ( 'NONE',  ( 126.6390922358630604, -3.374097159969326576, -8.400043106829690132 ) ) ;
#7510 = LINE ( 'NONE', #6236, #7708 ) ;
#7511 = CARTESIAN_POINT ( 'NONE',  ( 122.6667014775786413, -7.893985811506177619, -18.51759400769804742 ) ) ;
#7512 = CARTESIAN_POINT ( 'NONE',  ( 111.9559014775786494, -9.522524984348097021, -10.63868154973201108 ) ) ;
#7513 =( BOUNDED_SURFACE ( )  B_SPLINE_SURFACE ( 1, 2, ( 
 ( #31280, #6459, #23570, #41572, #34031, #13967, #20593, #30623, #10551, #34469, #28103, #274, #37905, #30845, #10332, #21027, #41126 ),
 ( #34900, #3689, #16951, #17611, #9648, #13300, #9885, #17174, #23796, #37686, #20368, #34255, #3030, #13750, #20809, #44768, #6683 ) ),
 .UNSPECIFIED., .F., .F., .T. ) 
 B_SPLINE_SURFACE_WITH_KNOTS ( ( 2, 2 ),
 ( 3, 2, 2, 2, 2, 2, 2, 2, 3 ),
 ( 0.000000000000000000, 1.000000000000000000 ),
 ( 0.000000000000000000, 0.1250000000000000000, 0.2500000000000000000, 0.3750000000000000000, 0.5000000000000000000, 0.6250000000000000000, 0.7500000000000000000, 0.8750000000000000000, 1.000000000000000000 ),
 .UNSPECIFIED. ) 
 GEOMETRIC_REPRESENTATION_ITEM ( )  RATIONAL_B_SPLINE_SURFACE ( (
 ( 1.000000000000000000, 0.9238795325112869605, 1.000000000000000000, 0.9238795325112869605, 1.000000000000000000, 0.9238795325112869605, 1.000000000000000000, 0.9238795325112869605, 1.000000000000000000, 0.9238795325112869605, 1.000000000000000000, 0.9238795325112869605, 1.000000000000000000, 0.9238795325112869605, 1.000000000000000000, 0.9238795325112869605, 1.000000000000000000),
 ( 1.000000000000000000, 0.9238795325112869605, 1.000000000000000000, 0.9238795325112869605, 1.000000000000000000, 0.9238795325112869605, 1.000000000000000000, 0.9238795325112869605, 1.000000000000000000, 0.9238795325112869605, 1.000000000000000000, 0.9238795325112869605, 1.000000000000000000, 0.9238795325112869605, 1.000000000000000000, 0.9238795325112869605, 1.000000000000000000) ) ) 
 REPRESENTATION_ITEM ( '' )  SURFACE ( )  );
#7514 = DIRECTION ( 'NONE',  ( 0.7202110682883375858, 0.2576522076061144029, -0.6441361323747234469 ) ) ;
#7515 = DIRECTION ( 'NONE',  ( -1.000000000000000000, 0.000000000000000000, 0.000000000000000000 ) ) ;
#7516 = ORIENTED_EDGE ( 'NONE', *, *, #10853, .F. ) ;
#7517 = AXIS2_PLACEMENT_3D ( 'NONE', #22594, #32842, #2063 ) ;
#7518 = DIRECTION ( 'NONE',  ( 0.000000000000000000, 0.000000000000000000, -1.000000000000000000 ) ) ;
#7519 = AXIS2_PLACEMENT_3D ( 'NONE', #6179, #16908, #2753 ) ;
#7520 = CARTESIAN_POINT ( 'NONE',  ( 119.4332814775786318, -0.4660016031367893996, -10.09054647747474043 ) ) ;
#7521 = CARTESIAN_POINT ( 'NONE',  ( 124.6521348109119884, -7.894159318335828068, -9.358103419637847864 ) ) ;
#7522 = ORIENTED_EDGE ( 'NONE', *, *, #34241, .F. ) ;
#7523 = DIRECTION ( 'NONE',  ( 0.9609149988134843001, -0.1028163501681632064, 0.2570431154366505933 ) ) ;
#7524 = CARTESIAN_POINT ( 'NONE',  ( 122.4397948109119767, -9.988377603198976828, -10.36322818467138340 ) ) ;
#7525 = CARTESIAN_POINT ( 'NONE',  ( 108.7462390045248242, 0.8980012041604421569, -15.77991374673208469 ) ) ;
#7526 = CARTESIAN_POINT ( 'NONE',  ( 123.8012348109119642, -9.565557343593413364, -10.61323700422348004 ) ) ;
#7527 = AXIS2_PLACEMENT_3D ( 'NONE', #42365, #42814, #32529 ) ;
#7528 = ORIENTED_EDGE ( 'NONE', *, *, #18352, .F. ) ;
#7529 = CARTESIAN_POINT ( 'NONE',  ( 116.2565881442452991, -9.261995988541697145, -16.69588392320189030 ) ) ;
#7530 = CARTESIAN_POINT ( 'NONE',  ( 62.92618109310924268, -32.76310523276723785, -23.89321520033831803 ) ) ;
#7531 = DIRECTION ( 'NONE',  ( 0.000000000000000000, 0.000000000000000000, -1.000000000000000000 ) ) ;
#7532 = DIRECTION ( 'NONE',  ( -1.000000000000000000, 0.000000000000000000, 0.000000000000000000 ) ) ;
#7533 = CARTESIAN_POINT ( 'NONE',  ( 111.6617281442453304, 0.4262465694468514643, -12.03445270309931736 ) ) ;
#7534 = EDGE_CURVE ( 'NONE', #38311, #36696, #11041, .T. ) ;
#7535 = CARTESIAN_POINT ( 'NONE',  ( 123.0681493241987425, -6.333924026435813204, -18.89660969823682279 ) ) ;
#7536 = DIRECTION ( 'NONE',  ( 0.000000000000000000, -0.3818493186865927203, 0.9242245927363029745 ) ) ;
#7537 = CARTESIAN_POINT ( 'NONE',  ( 121.7590748109119687, -7.893985811506177619, -18.51759400769804742 ) ) ;
#7539 = CARTESIAN_POINT ( 'NONE',  ( 123.7445081442452874, -7.894159318335828068, -9.358103419637847864 ) ) ;
#7538 = CARTESIAN_POINT ( 'NONE',  ( 124.0281414775786146, -1.834011780172310813, -8.268836392978581529 ) ) ;
#7540 = CARTESIAN_POINT ( 'NONE',  ( 118.3554748109119998, -9.565557343593413364, -10.61323700422348004 ) ) ;
#7541 = CARTESIAN_POINT ( 'NONE',  ( 125.7761281442453196, -10.10582367741896093, -14.73954123521881066 ) ) ;
#7542 = CARTESIAN_POINT ( 'NONE',  ( 117.3911214775786505, -1.561330072975668504, -17.79121239304076951 ) ) ;
#7543 = EDGE_LOOP ( 'NONE', ( #4128, #12032, #11215, #24908 ) ) ;
#7544 = PRESENTATION_LAYER_ASSIGNMENT (  '', '', ( #37398 ) ) ;
#7545 = EDGE_LOOP ( 'NONE', ( #6193, #32571 ) ) ;
#7546 = CARTESIAN_POINT ( 'NONE',  ( 76.56645223742121686, 1.201885453592819397, -15.89321520033831447 ) ) ;
#7547 = DIRECTION ( 'NONE',  ( 0.000000000000000000, 0.000000000000000000, 1.000000000000000000 ) ) ;
#7548 = CARTESIAN_POINT ( 'NONE',  ( 113.4690515045247992, -6.936859964151250502, -18.39754474579286025 ) ) ;
#7549 = VECTOR ( 'NONE', #26072, 1000.000000000000227 ) ;
#7550 = CARTESIAN_POINT ( 'NONE',  ( 109.7185827545247889, -6.936859964151250502, -8.388885654883777576 ) ) ;
#7551 = CARTESIAN_POINT ( 'NONE',  ( 113.2606921295247702, -9.868328341294093420, -13.39321520033831447 ) ) ;
#7552 = CARTESIAN_POINT ( 'NONE',  ( 124.3685014775786328, -10.63000616557722466, -14.87417383870573495 ) ) ;
#7553 = CARTESIAN_POINT ( 'NONE',  ( 112.2857214775786474, -4.089484607189486809, -7.948022111789456723 ) ) ;
#7554 = EDGE_LOOP ( 'NONE', ( #33129, #30401, #18640, #35038 ) ) ;
#7555 = CARTESIAN_POINT ( 'NONE',  ( 112.7395348109119766, -4.153390946401321671, -8.397313243818183892 ) ) ;
#7556 = CARTESIAN_POINT ( 'NONE',  ( 109.9269421295247753, 0.8980012041604618078, -13.39321520033831447 ) ) ;
#7557 = CARTESIAN_POINT ( 'NONE',  ( 119.6392035773848761, -2.467220198592778413, -17.83387418641524391 ) ) ;
#7558 = EDGE_CURVE ( 'NONE', #20751, #12347, #10818, .T. ) ;
#7559 = CARTESIAN_POINT ( 'NONE',  ( 120.2475493874819961, -6.063848558940142297, -18.38516058545102183 ) ) ;
#7560 = CARTESIAN_POINT ( 'NONE',  ( 124.1415948109119540, -6.344957434206665248, -7.627207830600338134 ) ) ;
#7561 = CARTESIAN_POINT ( 'NONE',  ( 63.13224612813448999, -13.41522658373937738, -18.64540057500950354 ) ) ;
#7562 = CARTESIAN_POINT ( 'NONE',  ( 115.2355081442453155, -10.30919188438810075, -12.61870101168855918 ) ) ;
#7563 = CARTESIAN_POINT ( 'NONE',  ( 114.0941296295247867, -4.863998795839590272, -19.15521520033831493 ) ) ;
#7564 = CARTESIAN_POINT ( 'NONE',  ( 113.5385046295247804, -4.863998795839590272, -18.39754474579285315 ) ) ;
#7565 = ORIENTED_EDGE ( 'NONE', *, *, #1349, .T. ) ;
#7566 = CIRCLE ( 'NONE', #44729, 1.499999999999996225 ) ;
#7567 = DIRECTION ( 'NONE',  ( 1.000000000000000000, 0.000000000000000000, -0.000000000000000000 ) ) ;
#7568 = CARTESIAN_POINT ( 'NONE',  ( 115.2355081442453155, 0.1319031606808879209, -14.10382304977623669 ) ) ;
#7569 = CARTESIAN_POINT ( 'NONE',  ( 126.2404814775786264, -0.8288870151387760510, -10.36305467784173118 ) ) ;
#7570 = CARTESIAN_POINT ( 'NONE',  ( 113.1933481442453058, -4.089484607189486809, -7.948022111789456723 ) ) ;
#7571 = CARTESIAN_POINT ( 'NONE',  ( 118.4122014775786340, -9.859900752359374465, -12.68260735090039404 ) ) ;
#7572 = CARTESIAN_POINT ( 'NONE',  ( 120.0572748109119772, -6.222761293078241884, -8.102969835052219238 ) ) ;
#7573 = CARTESIAN_POINT ( 'NONE',  ( 116.9940348109119839, -0.1624402480850797581, -16.17319339645315424 ) ) ;
#7574 = ORIENTED_EDGE ( 'NONE', *, *, #14450, .F. ) ;
#7575 = CARTESIAN_POINT ( 'NONE',  ( 121.3408766859119794, -9.033780868592240054, -16.85052413769862056 ) ) ;
#7576 = CARTESIAN_POINT ( 'NONE',  ( 128.2184548109119930, -4.863998795839242995, -13.39321520033831447 ) ) ;
#7577 = CARTESIAN_POINT ( 'NONE',  ( 113.7606148109119886, -7.894159318335828068, -9.358103419637847864 ) ) ;
#7578 = ORIENTED_EDGE ( 'NONE', *, *, #8890, .T. ) ;
#7579 = CARTESIAN_POINT ( 'NONE',  ( 126.2471382750693323, -8.992437524846883079, -16.23933567622449559 ) ) ;
#7580 = CARTESIAN_POINT ( 'NONE',  ( 106.9404577545248145, -7.250697342233347165, -7.631215200338321125 ) ) ;
#7581 = AXIS2_PLACEMENT_3D ( 'NONE', #37428, #6198, #29920 ) ;
#7582 = CARTESIAN_POINT ( 'NONE',  ( 112.5661608795247872, -1.325403438956436419, -16.93181055722141792 ) ) ;
#7583 = CARTESIAN_POINT ( 'NONE',  ( 124.0281414775786146, -7.643976991954077427, -18.09477374809248928 ) ) ;
#7584 = VERTEX_POINT ( 'NONE', #38839 ) ;
#7585 = CARTESIAN_POINT ( 'NONE',  ( 119.6601881442453106, -1.833838273342659253, -17.42832698103878286 ) ) ;
#7586 = CARTESIAN_POINT ( 'NONE',  ( 118.1852948109119836, -4.153390946401325223, -8.397313243818185668 ) ) ;
#7587 = CARTESIAN_POINT ( 'NONE',  ( 124.5726818087965171, -9.839536840243070515, -13.91122383889339353 ) ) ;
#7588 = EDGE_CURVE ( 'NONE', #42171, #1522, #10599, .T. ) ;
#7589 = CARTESIAN_POINT ( 'NONE',  ( 121.3408766859119794, -0.06289925094097943703, -9.412459353600674206 ) ) ;
#7590 = ORIENTED_EDGE ( 'NONE', *, *, #11969, .F. ) ;
#7591 = DIRECTION ( 'NONE',  ( 0.000000000000000000, 0.000000000000000000, -1.000000000000000000 ) ) ;
#7592 = DIRECTION ( 'NONE',  ( 0.000000000000000000, 0.000000000000000000, -1.000000000000000000 ) ) ;
#7593 = CARTESIAN_POINT ( 'NONE',  ( 112.8439733795247832, -8.938348069036489818, -17.46756447353520159 ) ) ;
#7594 = DIRECTION ( 'NONE',  ( -1.000000000000000000, 0.000000000000000000, 0.000000000000000000 ) ) ;
#7595 = CARTESIAN_POINT ( 'NONE',  ( 112.5693548109119888, -10.63000616557722466, -14.87417383870573495 ) ) ;
#7596 = CARTESIAN_POINT ( 'NONE',  ( 116.4834948109119779, -7.894159318335828068, -9.358103419637847864 ) ) ;
#7597 = DIRECTION ( 'NONE',  ( -0.9609149988134837450, 0.1028163501681639419, -0.2570431154366518145 ) ) ;
#7598 = EDGE_LOOP ( 'NONE', ( #32902, #5727, #2414, #21061 ) ) ;
#7599 = CARTESIAN_POINT ( 'NONE',  ( 116.0296814775786345, -1.833838273342658809, -17.42832698103878286 ) ) ;
#7600 = VECTOR ( 'NONE', #43151, 1000.000000000000227 ) ;
#7601 = CARTESIAN_POINT ( 'NONE',  ( 115.2053796295247849, -4.863998795839590272, -19.15521520033831493 ) ) ;
#7602 = CARTESIAN_POINT ( 'NONE',  ( 85.11152112150389826, -28.35884296389746595, -9.118680713869798282 ) ) ;
#7603 = DIRECTION ( 'NONE',  ( 1.000000000000000000, 0.000000000000000000, -0.000000000000000000 ) ) ;
#7604 = EDGE_CURVE ( 'NONE', #32855, #23460, #33415, .T. ) ;
#7605 = CARTESIAN_POINT ( 'NONE',  ( 113.4202548109119846, -10.30919188438810075, -12.61870101168855918 ) ) ;
#7606 = ORIENTED_EDGE ( 'NONE', *, *, #1993, .T. ) ;
#7607 = CARTESIAN_POINT ( 'NONE',  ( 115.5191414775786569, -3.383040157471821630, -19.15922257007629170 ) ) ;
#7608 = CARTESIAN_POINT ( 'NONE',  ( 113.9307948109119764, 0.9020085738987376756, -11.91225656197089755 ) ) ;
#7609 = CARTESIAN_POINT ( 'NONE',  ( 113.0523327545247838, -2.477300249445798297, -19.15521520033831138 ) ) ;
#7610 = CARTESIAN_POINT ( 'NONE',  ( 114.4413348109119823, -9.261995988541697145, -16.69588392320189030 ) ) ;
#7611 = CARTESIAN_POINT ( 'NONE',  ( 112.5693548109119888, -10.63000616557722466, -14.87417383870573495 ) ) ;
#7613 = CIRCLE ( 'NONE', #44783, 1.300000000000000044 ) ;
#7612 = DIRECTION ( 'NONE',  ( -1.000000000000000000, 0.000000000000000000, 0.000000000000000000 ) ) ;
#7614 = CARTESIAN_POINT ( 'NONE',  ( 111.8021765045248372, -2.791137627527939813, -8.388885654883754484 ) ) ;
#7615 = CARTESIAN_POINT ( 'NONE',  ( 110.8992858795247827, -8.402594152722688392, -9.854619843455216355 ) ) ;
#7616 = ORIENTED_EDGE ( 'NONE', *, *, #28641, .T. ) ;
#7617 = CARTESIAN_POINT ( 'NONE',  ( 121.8615784624957570, -6.270977643812233104, -18.77740645536396258 ) ) ;
#7618 = CARTESIAN_POINT ( 'NONE',  ( 109.2294421586085775, -7.222005445833587167, -18.14121012771779462 ) ) ;
#7619 = CARTESIAN_POINT ( 'NONE',  ( 116.5402214775786405, -9.565557343593413364, -10.61323700422348004 ) ) ;
#7620 = CARTESIAN_POINT ( 'NONE',  ( 123.9584548109119737, -4.863998795839242995, -13.39321520033831447 ) ) ;
#7621 = CARTESIAN_POINT ( 'NONE',  ( 122.6212569549021794, -1.135392229370309369, -17.10942237759952889 ) ) ;
#7622 = CARTESIAN_POINT ( 'NONE',  ( 111.0381921295247878, 0.8980012041604618078, -13.39321520033831447 ) ) ;
#7623 = CARTESIAN_POINT ( 'NONE',  ( 127.0553483106897943, -5.177147889503950218, -7.983820274244006754 ) ) ;
#7624 = CARTESIAN_POINT ( 'NONE',  ( 115.9729548109119861, -3.505236298600246325, -18.68346056562440793 ) ) ;
#7625 = CARTESIAN_POINT ( 'NONE',  ( 70.19189222814998175, -51.68868231262963775, -33.87830190084585524 ) ) ;
#7626 = CARTESIAN_POINT ( 'NONE',  ( 124.5386814775786206, -5.638512984488999180, -18.83840828888717311 ) ) ;
#7627 = CARTESIAN_POINT ( 'NONE',  ( 117.5613014775786525, 0.9020085738987339008, -11.91225656197089222 ) ) ;
#7628 = ORIENTED_EDGE ( 'NONE', *, *, #41595, .F. ) ;
#7629 = CARTESIAN_POINT ( 'NONE',  ( 115.7460481442453357, -10.15424416112533912, -14.75197769757731336 ) ) ;
#7630 = CARTESIAN_POINT ( 'NONE',  ( 72.54180985774836188, -61.58539327607277869, -37.10777877198333385 ) ) ;
#7632 = EDGE_CURVE ( 'NONE', #9687, #24866, #5765, .T. ) ;
#7631 = CARTESIAN_POINT ( 'NONE',  ( 117.6747548109119919, -1.834011780172310813, -8.268836392978581529 ) ) ;
#7633 = CARTESIAN_POINT ( 'NONE',  ( 114.5547881442453217, -4.153390946401321671, -8.397313243818183892 ) ) ;
#7634 = ORIENTED_EDGE ( 'NONE', *, *, #844, .T. ) ;
#7635 = CARTESIAN_POINT ( 'NONE',  ( 122.4397948109119767, -0.1624402480850797581, -16.17319339645315424 ) ) ;
#7636 = AXIS2_PLACEMENT_3D ( 'NONE', #16412, #12995, #2943 ) ;
#7637 = CARTESIAN_POINT ( 'NONE',  ( 118.0151148109119816, -10.63000616557722466, -14.87417383870573495 ) ) ;
#7638 = CARTESIAN_POINT ( 'NONE',  ( 83.82415148905927538, -32.76310523276723785, -22.89321520033831803 ) ) ;
#7639 = CARTESIAN_POINT ( 'NONE',  ( 109.2324108795247923, -8.938348069036489818, -9.318865927141430916 ) ) ;
#7640 = AXIS2_PLACEMENT_3D ( 'NONE', #35681, #39113, #10862 ) ;
#7641 = LINE ( 'NONE', #10854, #18416 ) ;
#7642 = CARTESIAN_POINT ( 'NONE',  ( 126.3037217343607495, 0.1656680361304483373, -13.75559490932021944 ) ) ;
#7643 = CARTESIAN_POINT ( 'NONE',  ( 115.2748327545248657, -6.936859964151250502, -8.388885654883777576 ) ) ;
#7644 = CARTESIAN_POINT ( 'NONE',  ( 113.7606148109119886, -1.561330072975668060, -17.79121239304076596 ) ) ;
#7645 = CARTESIAN_POINT ( 'NONE',  ( 89.33740294208338639, -9.098375579515472822, -16.89321520033831447 ) ) ;
#7646 = CARTESIAN_POINT ( 'NONE',  ( 114.3846081442453197, 0.4262465694468514643, -12.03445270309931736 ) ) ;
#7647 = CARTESIAN_POINT ( 'NONE',  ( 60.61575878210037871, -12.54259051716152307, -17.30460924804371103 ) ) ;
#7648 = CARTESIAN_POINT ( 'NONE',  ( -13.08016704199594393, -4.101600364181877900, -7.578546675885130313 ) ) ;
#7649 = CARTESIAN_POINT ( 'NONE',  ( 113.3301452545248083, -9.868328341294098749, -15.46607636864997204 ) ) ;
#7650 = CARTESIAN_POINT ( 'NONE',  ( 114.4980614775786734, -2.084020599724406786, -8.691656652584148546 ) ) ;
#7651 = CARTESIAN_POINT ( 'NONE',  ( 123.7184548109119788, -4.863998795839242995, -13.39321520033831447 ) ) ;
#7652 = CARTESIAN_POINT ( 'NONE',  ( 84.86020291624612355, -29.99489077589588959, -18.39321520033831803 ) ) ;
#7654 = CARTESIAN_POINT ( 'NONE',  ( 119.7736414775786358, -10.30919188438810075, -12.61870101168855918 ) ) ;
#7653 = CARTESIAN_POINT ( 'NONE',  ( 63.51882515645636573, -14.83470500876697606, -9.935931153571182506 ) ) ;
#7655 = EDGE_CURVE ( 'NONE', #37519, #10810, #2118, .T. ) ;
#7656 = CARTESIAN_POINT ( 'NONE',  ( 118.8092881442453290, -0.1624402480850797581, -16.17319339645315424 ) ) ;
#7657 = CARTESIAN_POINT ( 'NONE',  ( 113.4202548109119846, 0.1319031606808879209, -14.10382304977623669 ) ) ;
#7658 = ORIENTED_EDGE ( 'NONE', *, *, #5645, .T. ) ;
#7659 = CARTESIAN_POINT ( 'NONE',  ( 137.4478226697682999, -7.537440151351030515, -9.085464482628538008 ) ) ;
#7660 = CARTESIAN_POINT ( 'NONE',  ( 122.7234281442452755, -5.638512984488999180, -18.83840828888717311 ) ) ;
#7661 = CARTESIAN_POINT ( 'NONE',  ( 113.4690515045247992, -6.936859964151250502, -18.39754474579286025 ) ) ;
#7662 = CARTESIAN_POINT ( 'NONE',  ( 118.5256548109119876, -8.899110576539710493, -16.42337572283490132 ) ) ;
#7663 = CARTESIAN_POINT ( 'NONE',  ( 115.5758681442453053, -7.894159318335828068, -9.358103419637847864 ) ) ;
#7664 = LINE ( 'NONE', #31610, #14009 ) ;
#7665 = CARTESIAN_POINT ( 'NONE',  ( 113.7468640045248236, -10.62599879583958717, -11.00651665394454604 ) ) ;
#7666 = CIRCLE ( 'NONE', #33136, 3.000000000000002665 ) ;
#7667 = CARTESIAN_POINT ( 'NONE',  ( 119.5467348109119712, -5.574606645277164318, -18.38911715685844683 ) ) ;
#7668 = CARTESIAN_POINT ( 'NONE',  ( 123.3474214775786209, -0.1624402480850797581, -16.17319339645315424 ) ) ;
#7669 = CARTESIAN_POINT ( 'NONE',  ( 116.9163235773848726, -2.467220198592778413, -17.83387418641524391 ) ) ;
#7670 = CARTESIAN_POINT ( 'NONE',  ( 109.2293241013981060, -6.781090337013601754, -8.066615733728053073 ) ) ;
#7671 = CARTESIAN_POINT ( 'NONE',  ( 124.1884548109119777, -7.554583864224885481, -18.48844787311982785 ) ) ;
#7672 = B_SPLINE_CURVE_WITH_KNOTS ( 'NONE', 3,
 ( #22369, #943, #25352, #2457, #28994, #42901, #36265, #18947, #39476, #33447, #2227, #26639, #16379, #30281, #39246, #12968, #21700, #35588, #18278, #13420, #20705, #41460, #37571, #27324, #17066, #30505, #20028, #3582, #6109, #17286 ),
 .UNSPECIFIED., .F., .F.,
 ( 4, 2, 1, 1, 1, 1, 1, 2, 2, 2, 2, 2, 1, 1, 1, 2, 2, 2, 4 ),
 ( 0.000000000000000000, 0.1250000000000580647, 0.1875000000000879297, 0.2187500000001020017, 0.2343750000001090517, 0.2421875000001116884, 0.2460937500001130485, 0.2480468750001137146, 0.2500000000001144085, 0.3750000000001373346, 0.4375000000001479927, 0.4687500000001532663, 0.4843750000001549871, 0.4921875000001567635, 0.4960937500001575962, 0.4980468750001580958, 0.5000000000001585398, 0.7500000000000792699, 1.000000000000000000 ),
 .UNSPECIFIED. ) ;
#7673 = CARTESIAN_POINT ( 'NONE',  ( 113.2606921295247702, 0.8980012041604618078, -13.39321520033831447 ) ) ;
#7674 = CARTESIAN_POINT ( 'NONE',  ( 74.32979735608419958, -48.45188957854135481, -16.39321520033831447 ) ) ;
#7675 = CARTESIAN_POINT ( 'NONE',  ( 118.5823814775786360, -1.834011780172310813, -8.268836392978581529 ) ) ;
#7676 = CARTESIAN_POINT ( 'NONE',  ( 113.2500748109119968, -6.344957434206662583, -7.627207830600332805 ) ) ;
#7677 = CARTESIAN_POINT ( 'NONE',  ( 111.3160046295247838, -4.863998795839590272, -7.631215200338315796 ) ) ;
#7678 = CARTESIAN_POINT ( 'NONE',  ( 112.3424481442453384, -6.344957434206662583, -7.627207830600332805 ) ) ;
#7679 = ORIENTED_EDGE ( 'NONE', *, *, #25980, .T. ) ;
#7680 = LINE ( 'NONE', #31625, #25437 ) ;
#7681 = AXIS2_PLACEMENT_3D ( 'NONE', #38357, #10131, #14205 ) ;
#7682 = CARTESIAN_POINT ( 'NONE',  ( 124.4252281442452812, -9.261995988541697145, -16.69588392320189030 ) ) ;
#7683 = CARTESIAN_POINT ( 'NONE',  ( 115.1220548109119761, -8.166667518702817929, -8.995218007635861213 ) ) ;
#7684 = CARTESIAN_POINT ( 'NONE',  ( 120.7379948109119709, 0.4262465694468514643, -12.03445270309931736 ) ) ;
#7685 = PRODUCT_CONTEXT ( 'NONE', #25371, 'mechanical' ) ;
#7686 = CARTESIAN_POINT ( 'NONE',  ( 124.8790414775786246, -0.4660016031367893996, -10.09054647747474043 ) ) ;
#7687 = CARTESIAN_POINT ( 'NONE',  ( 122.4397948109119767, -9.988377603198976828, -10.36322818467138340 ) ) ;
#7688 = CARTESIAN_POINT ( 'NONE',  ( 112.9134265045247645, -7.250697342233347165, -19.15521520033831138 ) ) ;
#7689 = CARTESIAN_POINT ( 'NONE',  ( 116.9373081442452929, -1.833838273342659253, -17.42832698103878286 ) ) ;
#7690 = CARTESIAN_POINT ( 'NONE',  ( 67.37136766119182596, -70.31694239570130378, -42.20474206142759499 ) ) ;
#7691 = CARTESIAN_POINT ( 'NONE',  ( 71.02242295334774269, -49.63644658180010083, -36.16222241080433264 ) ) ;
#7692 = ORIENTED_EDGE ( 'NONE', *, *, #1112, .T. ) ;
#7693 = CARTESIAN_POINT ( 'NONE',  ( 121.4754414775786131, -8.166667518702819706, -8.995218007635861213 ) ) ;
#7694 = CARTESIAN_POINT ( 'NONE',  ( 122.1048610609119720, -3.163656168406935087, -18.89861972220014508 ) ) ;
#7695 = CARTESIAN_POINT ( 'NONE',  ( 117.9583881442453048, -10.30919188438810075, -12.61870101168855918 ) ) ;
#7696 = AXIS2_PLACEMENT_3D ( 'NONE', #13674, #9574, #34829 ) ;
#7697 = VERTEX_POINT ( 'NONE', #5313 ) ;
#7698 = CARTESIAN_POINT ( 'NONE',  ( 115.6915515045247531, -2.477300249445798297, -7.631215200338321125 ) ) ;
#7699 = CARTESIAN_POINT ( 'NONE',  ( 64.68571552958836435, -2.672612419674116335, -8.182496787467194110 ) ) ;
#7700 = FACE_OUTER_BOUND ( 'NONE', #27323, .T. ) ;
#7701 = CARTESIAN_POINT ( 'NONE',  ( 117.3343948109119737, -6.222761293078241884, -8.102969835052219238 ) ) ;
#7702 = DIRECTION ( 'NONE',  ( -0.000000000000000000, -0.9284778069183721172, -0.3713878862591650232 ) ) ;
#7703 = CARTESIAN_POINT ( 'NONE',  ( 64.47830633734803030, -35.88190373598614258, -5.786960771376335799 ) ) ;
#7704 = CARTESIAN_POINT ( 'NONE',  ( 118.5823814775786360, -7.643976991954077427, -18.09477374809248928 ) ) ;
#7705 = DIRECTION ( 'NONE',  ( 0.2768435750659235528, 0.3568721902840663041, -0.8921882507333145362 ) ) ;
#7706 = VECTOR ( 'NONE', #40235, 1000.000000000000114 ) ;
#7707 = CARTESIAN_POINT ( 'NONE',  ( 122.3830681442452857, -1.833838273342659697, -17.42832698103878286 ) ) ;
#7708 = VECTOR ( 'NONE', #20158, 1000.000000000000000 ) ;
#7709 = FACE_OUTER_BOUND ( 'NONE', #22621, .T. ) ;
#7710 = CARTESIAN_POINT ( 'NONE',  ( 119.6034614775786196, -3.505236298600246325, -18.68346056562440793 ) ) ;
#7711 = CARTESIAN_POINT ( 'NONE',  ( 114.2144281442453178, -8.166667518702817929, -8.995218007635859436 ) ) ;
#7712 = CARTESIAN_POINT ( 'NONE',  ( 119.6601881442453106, -8.166667518702819706, -8.995218007635861213 ) ) ;
#7713 = CARTESIAN_POINT ( 'NONE',  ( 126.1837548109119496, 0.4262465694468514643, -12.03445270309931736 ) ) ;
#7714 = CARTESIAN_POINT ( 'NONE',  ( 69.36136150295220659, -101.1685209014307674, -50.56525720990386219 ) ) ;
#7715 = CARTESIAN_POINT ( 'NONE',  ( 121.5321681442453183, -0.1624402480850797581, -16.17319339645315424 ) ) ;
#7716 = VERTEX_POINT ( 'NONE', #29040 ) ;
#7717 = CARTESIAN_POINT ( 'NONE',  ( 115.6893214775786447, 0.5811942927096154232, -14.16772938898807155 ) ) ;
#7718 = CARTESIAN_POINT ( 'NONE',  ( 111.9410827545248708, -6.936859964151250502, -8.388885654883777576 ) ) ;
#7719 = EDGE_CURVE ( 'NONE', #11048, #41727, #35607, .T. ) ;
#7720 = DIRECTION ( 'NONE',  ( 1.000000000000000000, 0.000000000000000000, -0.000000000000000000 ) ) ;
#7721 = CARTESIAN_POINT ( 'NONE',  ( 114.0941296295247867, -4.863998795839638234, -8.388885654883775800 ) ) ;
#7722 = DIRECTION ( 'NONE',  ( 0.7871354856660167654, -0.6167752151498625546, -0.002461946824136807422 ) ) ;
#7723 = CIRCLE ( 'NONE', #16505, 1.499999999999999334 ) ;
#7724 = EDGE_LOOP ( 'NONE', ( #27738, #23789, #13591, #32692 ) ) ;
#7725 = CARTESIAN_POINT ( 'NONE',  ( 126.3115243456346093, -8.177670693431501547, -9.587005482640760690 ) ) ;
#7726 = CARTESIAN_POINT ( 'NONE',  ( 121.2485348109119769, -8.899110576539710493, -16.42337572283490132 ) ) ;
#7727 = CARTESIAN_POINT ( 'NONE',  ( 116.5944421295247793, -4.863998795839590272, -13.39321520033831447 ) ) ;
#7728 = CARTESIAN_POINT ( 'NONE',  ( 60.11760374155739584, -14.70486118635414385, -19.35686119223086266 ) ) ;
#7729 = CARTESIAN_POINT ( 'NONE',  ( 125.9568481442452850, -6.344957434206665248, -7.627207830600338134 ) ) ;
#7730 = EDGE_CURVE ( 'NONE', #13487, #34510, #18139, .T. ) ;
#7731 = CARTESIAN_POINT ( 'NONE',  ( 110.7603796295247918, -4.863998795839590272, -8.388885654883775800 ) ) ;
#7732 = AXIS2_PLACEMENT_3D ( 'NONE', #27357, #2948, #24379 ) ;
#7733 = VERTEX_POINT ( 'NONE', #22867 ) ;
#7734 = CARTESIAN_POINT ( 'NONE',  ( 115.9729548109119861, -6.344957434206662583, -7.627207830600332805 ) ) ;
#7735 = CARTESIAN_POINT ( 'NONE',  ( 114.3846081442453197, -10.63000616557722466, -14.87417383870573495 ) ) ;
#7736 = CARTESIAN_POINT ( 'NONE',  ( 88.77226126511364157, -11.08399544887646293, -14.12116704279862667 ) ) ;
#7737 = CARTESIAN_POINT ( 'NONE',  ( 121.9292548109119849, -7.894159318335828068, -9.358103419637847864 ) ) ;
#7738 = FACE_OUTER_BOUND ( 'NONE', #26887, .T. ) ;
#7739 = CARTESIAN_POINT ( 'NONE',  ( 123.7445081442452874, -1.561330072975668948, -17.79121239304076951 ) ) ;
#7740 = CARTESIAN_POINT ( 'NONE',  ( 112.1722681442453222, -8.899110576539710493, -16.42337572283490132 ) ) ;
#7741 = DIRECTION ( 'NONE',  ( -0.2768435750659241079, -0.3568721902840695792, 0.8921882507333129819 ) ) ;
#7742 = PLANE ( 'NONE',  #41933 ) ;
#7743 = CARTESIAN_POINT ( 'NONE',  ( 125.6732148109119862, -9.859900752359378018, -12.68260735090039759 ) ) ;
#7744 = ORIENTED_EDGE ( 'NONE', *, *, #5224, .T. ) ;
#7745 = CIRCLE ( 'NONE', #453, 5.999999999999997335 ) ;
#7746 = ADVANCED_FACE ( 'NONE', ( #26068 ), #16033, .F. ) ;
#7747 = CARTESIAN_POINT ( 'NONE',  ( 114.2330358795247776, -8.402594152722688392, -9.854619843455216355 ) ) ;
#7748 = CARTESIAN_POINT ( 'NONE',  ( 120.1140014775786398, -1.561330072975668504, -17.79121239304076951 ) ) ;
#7749 = CARTESIAN_POINT ( 'NONE',  ( 136.8192643132354078, -9.964805478506571390, -15.65923222966296713 ) ) ;
#7750 = VERTEX_POINT ( 'NONE', #15807 ) ;
#7751 = PRODUCT_DEFINITION_SHAPE ( 'NONE', 'NONE',  #9359 ) ;
#7752 = EDGE_CURVE ( 'NONE', #38119, #3495, #2882, .T. ) ;
#7753 = CARTESIAN_POINT ( 'NONE',  ( 70.19189222814998175, -57.62004466406304459, -36.25082616574700722 ) ) ;
#7754 = EDGE_CURVE ( 'NONE', #12295, #21542, #36760, .T. ) ;
#7755 = ADVANCED_FACE ( 'NONE', ( #29941 ), #29708, .F. ) ;
#7756 = CARTESIAN_POINT ( 'NONE',  ( 111.8886348109120092, -6.222761293078241884, -8.102969835052219238 ) ) ;
#7757 = CARTESIAN_POINT ( 'NONE',  ( 35.90261398037149121, 14.17005867477686820, -7.393215200338315363 ) ) ;
#7758 = CARTESIAN_POINT ( 'NONE',  ( 123.6877814775786533, -6.222761293078241884, -8.102969835052219238 ) ) ;
#7759 = EDGE_LOOP ( 'NONE', ( #27228, #6712, #33060, #34498 ) ) ;
#7760 = CARTESIAN_POINT ( 'NONE',  ( 117.9016614775786280, -9.988377603198976828, -10.36322818467138340 ) ) ;
#7761 = AXIS2_PLACEMENT_3D ( 'NONE', #7798, #3917, #17836 ) ;
#7762 = CARTESIAN_POINT ( 'NONE',  ( 116.6208609388149426, -2.287189184988710267, -18.07361239780447448 ) ) ;
#7763 = CARTESIAN_POINT ( 'NONE',  ( 112.6373636215688521, -1.135392229370320694, -17.10942237759953954 ) ) ;
#7764 = CARTESIAN_POINT ( 'NONE',  ( 135.9690293846558404, -5.581979509648644644, -7.510532691874653999 ) ) ;
#7765 = CARTESIAN_POINT ( 'NONE',  ( 124.7655881442452852, 0.5811942927096110934, -14.16772938898807510 ) ) ;
#7766 = AXIS2_PLACEMENT_3D ( 'NONE', #29770, #1947, #36150 ) ;
#7767 = CARTESIAN_POINT ( 'NONE',  ( 71.37572422742091760, -11.86958442233774313, -21.89321520033831447 ) ) ;
#7768 = CARTESIAN_POINT ( 'NONE',  ( 96.46827370896536991, -25.38949206727775731, -12.58586697536825660 ) ) ;
#7769 = B_SPLINE_CURVE_WITH_KNOTS ( 'NONE', 3,
 ( #25745, #25968, #29608, #9091, #43524, #22993, #12292, #26644, #43069, #11837 ),
 .UNSPECIFIED., .F., .F.,
 ( 4, 3, 3, 4 ),
 ( 2.168404344971010024E-18, 0.0002476486541971034965, 0.0004952973025691040062, 0.0009610892161188160261 ),
 .UNSPECIFIED. ) ;
#7770 = CARTESIAN_POINT ( 'NONE',  ( 123.4041481442452834, -10.30919188438810075, -12.61870101168855918 ) ) ;
#7772 = CARTESIAN_POINT ( 'NONE',  ( 124.3685014775786328, 0.4262465694468514643, -12.03445270309931736 ) ) ;
#7771 = CARTESIAN_POINT ( 'NONE',  ( 122.7801548109119665, -3.383040157471821630, -19.15922257007629170 ) ) ;
#7773 = CARTESIAN_POINT ( 'NONE',  ( 126.2184548109105435, -9.814174330883648878, -12.68911139247483710 ) ) ;
#7774 = CARTESIAN_POINT ( 'NONE',  ( 123.8579614775786126, -9.859900752359378018, -12.68260735090039759 ) ) ;
#7775 = CARTESIAN_POINT ( 'NONE',  ( 113.1366214775786432, -7.643976991954077427, -18.09477374809248928 ) ) ;
#7776 = CARTESIAN_POINT ( 'NONE',  ( 117.9016614775786280, -9.988377603198976828, -10.36322818467138340 ) ) ;
#7777 = ORIENTED_EDGE ( 'NONE', *, *, #2248, .T. ) ;
#7778 = AXIS2_PLACEMENT_3D ( 'NONE', #17746, #31642, #24593 ) ;
#7779 = ORIENTED_EDGE ( 'NONE', *, *, #29474, .F. ) ;
#7780 = CARTESIAN_POINT ( 'NONE',  ( 122.4406277074048859, -2.419733177069661512, -17.89711025544711376 ) ) ;
#7781 = CARTESIAN_POINT ( 'NONE',  ( 75.95778847736481509, -3.256761025687722189, -16.89321520033831447 ) ) ;
#7782 = CARTESIAN_POINT ( 'NONE',  ( 115.2748327545248657, -6.936859964151250502, -8.388885654883777576 ) ) ;
#7783 = CARTESIAN_POINT ( 'NONE',  ( 111.5938171295247940, 0.1403307496149613920, -13.39321520033831447 ) ) ;
#7784 = CARTESIAN_POINT ( 'NONE',  ( 124.7088614775786226, 0.2603800115204892296, -16.42320221600525088 ) ) ;
#7785 = CARTESIAN_POINT ( 'NONE',  ( 111.8886348109120092, -3.383040157471821630, -19.15922257007629170 ) ) ;
#7786 = ORIENTED_EDGE ( 'NONE', *, *, #38125, .F. ) ;
#7787 = CARTESIAN_POINT ( 'NONE',  ( 113.8173414775786512, -9.565557343593413364, -10.61323700422348004 ) ) ;
#7788 = CARTESIAN_POINT ( 'NONE',  ( 106.1764733795248219, -8.938348069036489818, -17.46756447353520159 ) ) ;
#7789 = CARTESIAN_POINT ( 'NONE',  ( 96.23375075340858587, -25.23356801022904961, -15.23591384769724755 ) ) ;
#7790 = LINE ( 'NONE', #25569, #40775 ) ;
#7791 =( BOUNDED_SURFACE ( )  B_SPLINE_SURFACE ( 1, 2, ( 
 ( #14112, #10480, #24381, #10699, #35512, #43052, #22300, #4054, #25049, #4517, #35744, #18659, #18440, #32550, #32329, #36197, #643, #17978, #15011, #1095, #31878, #28924, #42831, #11592, #21848, #14558, #22080, #28701, #25502, #28477, #8396, #15230, #42606, #39173, #38943, #4962, #29139, #32101, #39407, #8170, #11371, #11145, #25277, #42381, #7711, #35968, #4738, #1319, #21624, #11818, #4284, #25726, #39633, #7937, #18203, #868, #14787, #24745, #130, #14486, #41428, #42088, #24973, #27959, #4215, #17685, #6761, #18131, #17459, #28396, #7407, #41867, #31137, #20670, #10848, #13821, #24316, #10184, #28180, #10406, #24091, #31357, #3544, #38201, #45061, #34546, #35213, #21096, #38633, #38868, #21550, #27510, #44848, #350, #14042, #3985, #3327, #10627, #24531, #17249, #38418, #35438, #21327, #13600, #37984, #14263, #3762, #27735, #7189, #34975, #41649, #7637, #6979, #20887, #17907, #34765, #31583, #31805, #576, #42309, #11069, #43428, #39100, #32694, #14938, #36337, #32910, #39774, #39997, #11971, #35892, #11524, #42974, #36565, #5107, #12194, #18581, #29065, #42760, #8543, #22445, #32473, #28849, #792, #4887, #14714, #15607, #19025, #1688, #29514, #39330, #8098, #39559, #7870, #26093, #8762, #29290, #11294, #28625, #15387, #25428, #22669, #21779, #5341, #1463, #21999, #11745, #32025, #42534, #25870, #4661, #1248, #25204, #35669, #15160, #25653, #8319, #4443, #22222, #18361, #32253, #1021, #36117, #18804, #43204, #12879, #9909, #37009, #16749, #6010, #26322, #19699, #16060, #23131, #12653, #19934, #37708, #30643, #15836, #44113, #16293, #29967, #29735, #2131, #19258, #2820, #23821, #2363, #12421, #26779, #5779, #44340, #44563, #33137, #40688, #1909, #20170, #19477, #8997, #33588, #13326, #43881, #43646, #37475, #37238, #6248, #9441, #26549, #40229, #22893, #9223, #36788, #5558, #33358, #33819, #30194, #40460, #2591, #34053, #23352, #16522, #30419, #13099, #27000, #27233, #40919, #41148, #9673, #23591, #44164, #22946, #12472, #2871, #41197, #16339, #26826, #40511 ),
 ( #13381, #20217, #16800, #34103, #37060, #5833, #37292, #36839, #44615, #9957, #27053, #9046, #26372, #13150, #26598, #27282, #5607, #23871, #6298, #2182, #19753, #2413, #9274, #43700, #23182, #30696, #37756, #29787, #6062, #12928, #40282, #19981, #33870, #2640, #30242, #6526, #30466, #33637, #40737, #20443, #34326, #9726, #9494, #23408, #19530, #3099, #16572, #44386, #40971, #33406, #12698, #16112, #30013, #43932, #23638, #37525, #42302, #10624, #7633, #34759, #14482, #3759, #24087, #17456, #13818, #20883, #10401, #17681, #35435, #28392, #13597, #41862, #14038, #27731, #27507, #45058, #17027, #573, #21546, #127, #10181, #24527, #3541, #42084, #11066, #30919, #38414, #44841, #17904, #17243, #6755, #31352, #24968, #41646, #41425, #35209, #34971, #3981, #7183, #24311, #37981, #20666, #6974, #34541, #3323, #31134, #31579, #27955, #38197, #346, #31801, #21093, #14259, #28176, #10844, #24739, #38864, #38629, #7404, #21322, #11291, #35666, #4656, #21774, #32022, #39554, #8759, #22665, #39326, #18357, #1245, #4211, #4439, #8094, #21996, #11966, #8540, #8316, #25650, #18128, #39769, #15382, #32247, #1682, #39994, #787, #25200, #15157, #29062, #25866, #42971, #22442, #11739, #12189, #14708, #15604, #28621, #22217, #36113, #14934, #42531, #1018, #39097, #32907, #7867, #32469, #28845, #4884, #35886, #29286, #29508, #42757, #18801, #11521, #5104, #25425, #18577, #32691, #43424, #1460, #43200, #36334, #19020, #26090, #26775, #43878, #12418, #41145, #26545, #19254, #33133, #26318, #9436, #40456, #40226, #37233, #23587, #29963, #12649, #40685, #29730, #9218, #6244, #23128, #44557, #37472, #43643, #22890, #37004, #8990, #1903, #23349, #9905, #36561, #5775, #5554, #33584, #5336, #36783, #19695, #2360, #44336, #40915, #6007, #12876, #15832, #26995, #2586, #19472, #34049, #27227, #33355, #2127, #16289, #30191, #13096, #44109, #9669, #19930, #13323, #16057, #33816, #16517, #30416, #20166, #2817, #16746, #30640, #10347, #514, #24466, #20613, #20825, #14425, #24685, #3706, #34487 ) ),
 .UNSPECIFIED., .F., .F., .F. ) 
 B_SPLINE_SURFACE_WITH_KNOTS ( ( 2, 2 ),
 ( 3, 2, 2, 2, 2, 2, 2, 2, 2, 2, 2, 2, 2, 2, 2, 2, 2, 2, 2, 2, 2, 2, 2, 2, 2, 2, 2, 2, 2, 2, 2, 2, 2, 2, 2, 2, 2, 2, 2, 2, 2, 2, 2, 2, 2, 2, 2, 2, 2, 2, 2, 2, 2, 2, 2, 2, 2, 2, 2, 2, 2, 2, 2, 2, 2, 2, 2, 2, 2, 2, 2, 2, 2, 2, 2, 2, 2, 2, 2, 2, 2, 2, 2, 2, 2, 2, 2, 2, 2, 2, 2, 2, 2, 2, 2, 2, 2, 2, 2, 2, 2, 2, 2, 2, 2, 2, 2, 2, 2, 2, 2, 2, 2, 2, 2, 2, 2, 2, 2, 2, 2, 2, 2, 2, 2, 2, 2, 2, 3 ),
 ( 0.000000000000000000, 1.000000000000000000 ),
 ( 0.000000000000000000, 0.007812500000000000000, 0.01562500000000000000, 0.02343750000000000000, 0.03125000000000000000, 0.03906250000000000000, 0.04687500000000000000, 0.05468750000000000000, 0.06250000000000000000, 0.07031250000000000000, 0.07812500000000000000, 0.08593750000000000000, 0.09375000000000000000, 0.1015625000000000000, 0.1093750000000000000, 0.1171875000000000000, 0.1250000000000000000, 0.1328125000000000000, 0.1406250000000000000, 0.1484375000000000000, 0.1562500000000000000, 0.1640625000000000000, 0.1718750000000000000, 0.1796875000000000000, 0.1875000000000000000, 0.1953125000000000000, 0.2031250000000000000, 0.2109375000000000000, 0.2187500000000000000, 0.2265625000000000000, 0.2343750000000000000, 0.2421875000000000000, 0.2500000000000000000, 0.2578125000000000000, 0.2656250000000000000, 0.2734375000000000000, 0.2812500000000000000, 0.2890625000000000000, 0.2968750000000000000, 0.3046875000000000000, 0.3125000000000000000, 0.3203125000000000000, 0.3281250000000000000, 0.3359375000000000000, 0.3437500000000000000, 0.3515625000000000000, 0.3593750000000000000, 0.3671875000000000000, 0.3750000000000000000, 0.3828125000000000000, 0.3906250000000000000, 0.3984375000000000000, 0.4062500000000000000, 0.4140625000000000000, 0.4218750000000000000, 0.4296875000000000000, 0.4375000000000000000, 0.4453125000000000000, 0.4531250000000000000, 0.4609375000000000000, 0.4687500000000000000, 0.4765625000000000000, 0.4843750000000000000, 0.4921875000000000000, 0.5000000000000000000, 0.5078125000000000000, 0.5156250000000000000, 0.5234375000000000000, 0.5312500000000000000, 0.5390625000000000000, 0.5468750000000000000, 0.5546875000000000000, 0.5625000000000000000, 0.5703125000000000000, 0.5781250000000000000, 0.5859375000000000000, 0.5937500000000000000, 0.6015625000000000000, 0.6093750000000000000, 0.6171875000000000000, 0.6250000000000000000, 0.6328125000000000000, 0.6406250000000000000, 0.6484375000000000000, 0.6562500000000000000, 0.6640625000000000000, 0.6718750000000000000, 0.6796875000000000000, 0.6875000000000000000, 0.6953125000000000000, 0.7031250000000000000, 0.7109375000000000000, 0.7187500000000000000, 0.7265625000000000000, 0.7343750000000000000, 0.7421875000000000000, 0.7500000000000000000, 0.7578125000000000000, 0.7656250000000000000, 0.7734375000000000000, 0.7812500000000000000, 0.7890625000000000000, 0.7968750000000000000, 0.8046875000000000000, 0.8125000000000000000, 0.8203125000000000000, 0.8281250000000000000, 0.8359375000000000000, 0.8437500000000000000, 0.8515625000000000000, 0.8593750000000000000, 0.8671875000000000000, 0.8750000000000000000, 0.8828125000000000000, 0.8906250000000000000, 0.8984375000000000000, 0.9062500000000000000, 0.9140625000000000000, 0.9218750000000000000, 0.9296875000000000000, 0.9375000000000000000, 0.9453125000000000000, 0.9531250000000000000, 0.9609375000000000000, 0.9687500000000000000, 0.9765625000000000000, 0.9843750000000000000, 0.9921875000000000000, 1.000000000000000000 ),
 .UNSPECIFIED. ) 
 GEOMETRIC_REPRESENTATION_ITEM ( )  RATIONAL_B_SPLINE_SURFACE ( (
 ( 1.000000000000000000, 0.9238795325112869605, 1.000000000000000000, 0.9238795325112869605, 1.000000000000000000, 0.9238795325112869605, 1.000000000000000000, 0.9238795325112869605, 1.000000000000000000, 0.9238795325112869605, 1.000000000000000000, 0.9238795325112869605, 1.000000000000000000, 0.9238795325112869605, 1.000000000000000000, 0.9238795325112869605, 1.000000000000000000, 0.9238795325112869605, 1.000000000000000000, 0.9238795325112869605, 1.000000000000000000, 0.9238795325112869605, 1.000000000000000000, 0.9238795325112869605, 1.000000000000000000, 0.9238795325112869605, 1.000000000000000000, 0.9238795325112869605, 1.000000000000000000, 0.9238795325112869605, 1.000000000000000000, 0.9238795325112869605, 1.000000000000000000, 0.9238795325112869605, 1.000000000000000000, 0.9238795325112869605, 1.000000000000000000, 0.9238795325112869605, 1.000000000000000000, 0.9238795325112869605, 1.000000000000000000, 0.9238795325112869605, 1.000000000000000000, 0.9238795325112869605, 1.000000000000000000, 0.9238795325112869605, 1.000000000000000000, 0.9238795325112869605, 1.000000000000000000, 0.9238795325112869605, 1.000000000000000000, 0.9238795325112869605, 1.000000000000000000, 0.9238795325112869605, 1.000000000000000000, 0.9238795325112869605, 1.000000000000000000, 0.9238795325112869605, 1.000000000000000000, 0.9238795325112869605, 1.000000000000000000, 0.9238795325112869605, 1.000000000000000000, 0.9238795325112869605, 1.000000000000000000, 0.9238795325112869605, 1.000000000000000000, 0.9238795325112869605, 1.000000000000000000, 0.9238795325112869605, 1.000000000000000000, 0.9238795325112869605, 1.000000000000000000, 0.9238795325112869605, 1.000000000000000000, 0.9238795325112869605, 1.000000000000000000, 0.9238795325112869605, 1.000000000000000000, 0.9238795325112869605, 1.000000000000000000, 0.9238795325112869605, 1.000000000000000000, 0.9238795325112869605, 1.000000000000000000, 0.9238795325112869605, 1.000000000000000000, 0.9238795325112869605, 1.000000000000000000, 0.9238795325112869605, 1.000000000000000000, 0.9238795325112869605, 1.000000000000000000, 0.9238795325112869605, 1.000000000000000000, 0.9238795325112869605, 1.000000000000000000, 0.9238795325112869605, 1.000000000000000000, 0.9238795325112869605, 1.000000000000000000, 0.9238795325112869605, 1.000000000000000000, 0.9238795325112869605, 1.000000000000000000, 0.9238795325112869605, 1.000000000000000000, 0.9238795325112869605, 1.000000000000000000, 0.9238795325112869605, 1.000000000000000000, 0.9238795325112869605, 1.000000000000000000, 0.9238795325112869605, 1.000000000000000000, 0.9238795325112869605, 1.000000000000000000, 0.9238795325112869605, 1.000000000000000000, 0.9238795325112869605, 1.000000000000000000, 0.9238795325112869605, 1.000000000000000000, 0.9238795325112869605, 1.000000000000000000, 0.9238795325112869605, 1.000000000000000000, 0.9238795325112869605, 1.000000000000000000, 0.9238795325112869605, 1.000000000000000000, 0.9238795325112869605, 1.000000000000000000, 0.9238795325112869605, 1.000000000000000000, 0.9238795325112869605, 1.000000000000000000, 0.9238795325112869605, 1.000000000000000000, 0.9238795325112869605, 1.000000000000000000, 0.9238795325112869605, 1.000000000000000000, 0.9238795325112869605, 1.000000000000000000, 0.9238795325112869605, 1.000000000000000000, 0.9238795325112869605, 1.000000000000000000, 0.9238795325112869605, 1.000000000000000000, 0.9238795325112869605, 1.000000000000000000, 0.9238795325112869605, 1.000000000000000000, 0.9238795325112869605, 1.000000000000000000, 0.9238795325112869605, 1.000000000000000000, 0.9238795325112869605, 1.000000000000000000, 0.9238795325112869605, 1.000000000000000000, 0.9238795325112869605, 1.000000000000000000, 0.9238795325112869605, 1.000000000000000000, 0.9238795325112869605, 1.000000000000000000, 0.9238795325112869605, 1.000000000000000000, 0.9238795325112869605, 1.000000000000000000, 0.9238795325112869605, 1.000000000000000000, 0.9238795325112869605, 1.000000000000000000, 0.9238795325112869605, 1.000000000000000000, 0.9238795325112869605, 1.000000000000000000, 0.9238795325112869605, 1.000000000000000000, 0.9238795325112869605, 1.000000000000000000, 0.9238795325112869605, 1.000000000000000000, 0.9238795325112869605, 1.000000000000000000, 0.9238795325112869605, 1.000000000000000000, 0.9238795325112869605, 1.000000000000000000, 0.9238795325112869605, 1.000000000000000000, 0.9238795325112869605, 1.000000000000000000, 0.9238795325112869605, 1.000000000000000000, 0.9238795325112869605, 1.000000000000000000, 0.9238795325112869605, 1.000000000000000000, 0.9238795325112869605, 1.000000000000000000, 0.9238795325112869605, 1.000000000000000000, 0.9238795325112869605, 1.000000000000000000, 0.9238795325112869605, 1.000000000000000000, 0.9238795325112869605, 1.000000000000000000, 0.9238795325112869605, 1.000000000000000000, 0.9238795325112869605, 1.000000000000000000, 0.9238795325112869605, 1.000000000000000000, 0.9238795325112869605, 1.000000000000000000, 0.9238795325112869605, 1.000000000000000000, 0.9238795325112869605, 1.000000000000000000, 0.9238795325112869605, 1.000000000000000000, 0.9238795325112869605, 1.000000000000000000, 0.9238795325112869605, 1.000000000000000000, 0.9238795325112869605, 1.000000000000000000, 0.9238795325112869605, 1.000000000000000000, 0.9238795325112869605, 1.000000000000000000, 0.9238795325112869605, 1.000000000000000000, 0.9238795325112869605, 1.000000000000000000, 0.9238795325112869605, 1.000000000000000000, 0.9238795325112869605, 1.000000000000000000, 0.9238795325112869605, 1.000000000000000000, 0.9238795325112869605, 1.000000000000000000, 0.9238795325112869605, 1.000000000000000000, 0.9238795325112869605, 1.000000000000000000, 0.9238795325112869605, 1.000000000000000000, 0.9238795325112869605, 1.000000000000000000),
 ( 1.000000000000000000, 0.9238795325112869605, 1.000000000000000000, 0.9238795325112869605, 1.000000000000000000, 0.9238795325112869605, 1.000000000000000000, 0.9238795325112869605, 1.000000000000000000, 0.9238795325112869605, 1.000000000000000000, 0.9238795325112869605, 1.000000000000000000, 0.9238795325112869605, 1.000000000000000000, 0.9238795325112869605, 1.000000000000000000, 0.9238795325112869605, 1.000000000000000000, 0.9238795325112869605, 1.000000000000000000, 0.9238795325112869605, 1.000000000000000000, 0.9238795325112869605, 1.000000000000000000, 0.9238795325112869605, 1.000000000000000000, 0.9238795325112869605, 1.000000000000000000, 0.9238795325112869605, 1.000000000000000000, 0.9238795325112869605, 1.000000000000000000, 0.9238795325112869605, 1.000000000000000000, 0.9238795325112869605, 1.000000000000000000, 0.9238795325112869605, 1.000000000000000000, 0.9238795325112869605, 1.000000000000000000, 0.9238795325112869605, 1.000000000000000000, 0.9238795325112869605, 1.000000000000000000, 0.9238795325112869605, 1.000000000000000000, 0.9238795325112869605, 1.000000000000000000, 0.9238795325112869605, 1.000000000000000000, 0.9238795325112869605, 1.000000000000000000, 0.9238795325112869605, 1.000000000000000000, 0.9238795325112869605, 1.000000000000000000, 0.9238795325112869605, 1.000000000000000000, 0.9238795325112869605, 1.000000000000000000, 0.9238795325112869605, 1.000000000000000000, 0.9238795325112869605, 1.000000000000000000, 0.9238795325112869605, 1.000000000000000000, 0.9238795325112869605, 1.000000000000000000, 0.9238795325112869605, 1.000000000000000000, 0.9238795325112869605, 1.000000000000000000, 0.9238795325112869605, 1.000000000000000000, 0.9238795325112869605, 1.000000000000000000, 0.9238795325112869605, 1.000000000000000000, 0.9238795325112869605, 1.000000000000000000, 0.9238795325112869605, 1.000000000000000000, 0.9238795325112869605, 1.000000000000000000, 0.9238795325112869605, 1.000000000000000000, 0.9238795325112869605, 1.000000000000000000, 0.9238795325112869605, 1.000000000000000000, 0.9238795325112869605, 1.000000000000000000, 0.9238795325112869605, 1.000000000000000000, 0.9238795325112869605, 1.000000000000000000, 0.9238795325112869605, 1.000000000000000000, 0.9238795325112869605, 1.000000000000000000, 0.9238795325112869605, 1.000000000000000000, 0.9238795325112869605, 1.000000000000000000, 0.9238795325112869605, 1.000000000000000000, 0.9238795325112869605, 1.000000000000000000, 0.9238795325112869605, 1.000000000000000000, 0.9238795325112869605, 1.000000000000000000, 0.9238795325112869605, 1.000000000000000000, 0.9238795325112869605, 1.000000000000000000, 0.9238795325112869605, 1.000000000000000000, 0.9238795325112869605, 1.000000000000000000, 0.9238795325112869605, 1.000000000000000000, 0.9238795325112869605, 1.000000000000000000, 0.9238795325112869605, 1.000000000000000000, 0.9238795325112869605, 1.000000000000000000, 0.9238795325112869605, 1.000000000000000000, 0.9238795325112869605, 1.000000000000000000, 0.9238795325112869605, 1.000000000000000000, 0.9238795325112869605, 1.000000000000000000, 0.9238795325112869605, 1.000000000000000000, 0.9238795325112869605, 1.000000000000000000, 0.9238795325112869605, 1.000000000000000000, 0.9238795325112869605, 1.000000000000000000, 0.9238795325112869605, 1.000000000000000000, 0.9238795325112869605, 1.000000000000000000, 0.9238795325112869605, 1.000000000000000000, 0.9238795325112869605, 1.000000000000000000, 0.9238795325112869605, 1.000000000000000000, 0.9238795325112869605, 1.000000000000000000, 0.9238795325112869605, 1.000000000000000000, 0.9238795325112869605, 1.000000000000000000, 0.9238795325112869605, 1.000000000000000000, 0.9238795325112869605, 1.000000000000000000, 0.9238795325112869605, 1.000000000000000000, 0.9238795325112869605, 1.000000000000000000, 0.9238795325112869605, 1.000000000000000000, 0.9238795325112869605, 1.000000000000000000, 0.9238795325112869605, 1.000000000000000000, 0.9238795325112869605, 1.000000000000000000, 0.9238795325112869605, 1.000000000000000000, 0.9238795325112869605, 1.000000000000000000, 0.9238795325112869605, 1.000000000000000000, 0.9238795325112869605, 1.000000000000000000, 0.9238795325112869605, 1.000000000000000000, 0.9238795325112869605, 1.000000000000000000, 0.9238795325112869605, 1.000000000000000000, 0.9238795325112869605, 1.000000000000000000, 0.9238795325112869605, 1.000000000000000000, 0.9238795325112869605, 1.000000000000000000, 0.9238795325112869605, 1.000000000000000000, 0.9238795325112869605, 1.000000000000000000, 0.9238795325112869605, 1.000000000000000000, 0.9238795325112869605, 1.000000000000000000, 0.9238795325112869605, 1.000000000000000000, 0.9238795325112869605, 1.000000000000000000, 0.9238795325112869605, 1.000000000000000000, 0.9238795325112869605, 1.000000000000000000, 0.9238795325112869605, 1.000000000000000000, 0.9238795325112869605, 1.000000000000000000, 0.9238795325112869605, 1.000000000000000000, 0.9238795325112869605, 1.000000000000000000, 0.9238795325112869605, 1.000000000000000000, 0.9238795325112869605, 1.000000000000000000, 0.9238795325112869605, 1.000000000000000000, 0.9238795325112869605, 1.000000000000000000, 0.9238795325112869605, 1.000000000000000000, 0.9238795325112869605, 1.000000000000000000, 0.9238795325112869605, 1.000000000000000000, 0.9238795325112869605, 1.000000000000000000, 0.9238795325112869605, 1.000000000000000000, 0.9238795325112869605, 1.000000000000000000, 0.9238795325112869605, 1.000000000000000000, 0.9238795325112869605, 1.000000000000000000, 0.9238795325112869605, 1.000000000000000000, 0.9238795325112869605, 1.000000000000000000, 0.9238795325112869605, 1.000000000000000000, 0.9238795325112869605, 1.000000000000000000, 0.9238795325112869605, 1.000000000000000000, 0.9238795325112869605, 1.000000000000000000) ) ) 
 REPRESENTATION_ITEM ( '' )  SURFACE ( )  );
#7792 = CARTESIAN_POINT ( 'NONE',  ( 138.2184548109119930, -5.849744126848086090, -20.32346094940048786 ) ) ;
#7793 = DIRECTION ( 'NONE',  ( -0.000000000000000000, -0.9284778069183721172, -0.3713878862591650232 ) ) ;
#7794 = CARTESIAN_POINT ( 'NONE',  ( 116.0864081442453113, -9.988377603198976828, -10.36322818467138340 ) ) ;
#7795 = CARTESIAN_POINT ( 'NONE',  ( 113.6774108795247997, -8.938348069036489818, -9.318865927141430916 ) ) ;
#7796 = CARTESIAN_POINT ( 'NONE',  ( 109.7185827545247889, -6.936859964151250502, -8.388885654883777576 ) ) ;
#7797 = ORIENTED_EDGE ( 'NONE', *, *, #17908, .T. ) ;
#7798 = CARTESIAN_POINT ( 'NONE',  ( 79.72353890764954087, 4.236894767232761261, -4.893215200338314474 ) ) ;
#7799 = CARTESIAN_POINT ( 'NONE',  ( 115.7460481442453357, -10.15424416112533912, -14.75197769757731336 ) ) ;
#7800 = CARTESIAN_POINT ( 'NONE',  ( 117.2776681442452968, -5.638512984488999180, -18.83840828888717311 ) ) ;
#7801 = AXIS2_PLACEMENT_3D ( 'NONE', #15103, #965, #1848 ) ;
#7802 = FACE_OUTER_BOUND ( 'NONE', #4773, .T. ) ;
#7803 = CARTESIAN_POINT ( 'NONE',  ( 125.7299414775786346, -10.15424416112533912, -14.75197769757731336 ) ) ;
#7804 = CARTESIAN_POINT ( 'NONE',  ( 121.4754414775786131, -1.833838273342659697, -17.42832698103878286 ) ) ;
#7805 = CARTESIAN_POINT ( 'NONE',  ( 117.2209414775786485, -2.084020599724406786, -8.691656652584148546 ) ) ;
#7806 = EDGE_LOOP ( 'NONE', ( #39921, #42179, #16867, #17002 ) ) ;
#7807 = CIRCLE ( 'NONE', #15814, 2.000000000000000444 ) ;
#7808 = CARTESIAN_POINT ( 'NONE',  ( 122.1048610609119720, -6.340755971794695078, -8.611740276972781771 ) ) ;
#7809 = CARTESIAN_POINT ( 'NONE',  ( 70.19189222814998175, -60.04498257489500190, -37.22079287717834717 ) ) ;
#7810 = CARTESIAN_POINT ( 'NONE',  ( 118.8660148109119774, 0.1319031606808879209, -14.10382304977623669 ) ) ;
#7811 = ORIENTED_EDGE ( 'NONE', *, *, #7243, .F. ) ;
#7812 = CARTESIAN_POINT ( 'NONE',  ( 65.22670707961066228, -15.48412389236482412, -10.39321520033830737 ) ) ;
#7813 = EDGE_CURVE ( 'NONE', #40452, #34050, #27414, .T. ) ;
#7814 = CARTESIAN_POINT ( 'NONE',  ( 112.0020881442453344, 0.2603800115204892296, -16.42320221600525088 ) ) ;
#7815 = AXIS2_PLACEMENT_3D ( 'NONE', #12270, #19325, #36858 ) ;
#7816 = CARTESIAN_POINT ( 'NONE',  ( 114.9970202545248412, -10.62599879583958717, -15.77991374673208469 ) ) ;
#7817 = CARTESIAN_POINT ( 'NONE',  ( 113.5904348109119866, -2.084020599724406786, -8.691656652584148546 ) ) ;
#7818 = ORIENTED_EDGE ( 'NONE', *, *, #29071, .F. ) ;
#7819 = ORIENTED_EDGE ( 'NONE', *, *, #2184, .F. ) ;
#7820 = CARTESIAN_POINT ( 'NONE',  ( 118.9794681442453026, -0.8288870151387760510, -10.36305467784173118 ) ) ;
#7821 = CARTESIAN_POINT ( 'NONE',  ( 116.4267681442453153, -6.222761293078241884, -8.102969835052219238 ) ) ;
#7822 = EDGE_CURVE ( 'NONE', #12720, #14709, #35539, .T. ) ;
#7823 = CARTESIAN_POINT ( 'NONE',  ( 124.5380943420727249, -9.841908302772747419, -12.91703728233334125 ) ) ;
#7824 = CARTESIAN_POINT ( 'NONE',  ( 121.5492360609119800, -6.564341423271550902, -7.887810678476487425 ) ) ;
#7825 = ORIENTED_EDGE ( 'NONE', *, *, #33475, .T. ) ;
#7826 = DIRECTION ( 'NONE',  ( -1.000000000000000000, 1.352015467487876840E-15, 0.000000000000000000 ) ) ;
#7827 = CARTESIAN_POINT ( 'NONE',  ( 119.7434548109119703, -2.578558445503555951, -8.944152590684078419 ) ) ;
#7828 = CARTESIAN_POINT ( 'NONE',  ( 109.1629577545248395, -7.250697342233347165, -7.631215200338321125 ) ) ;
#7829 = AXIS2_PLACEMENT_3D ( 'NONE', #11309, #34991, #17923 ) ;
#7830 = CARTESIAN_POINT ( 'NONE',  ( 112.0020881442453344, 0.2603800115204892296, -16.42320221600525088 ) ) ;
#7831 = CARTESIAN_POINT ( 'NONE',  ( 126.6375681442452930, -10.15424416112533912, -14.75197769757731336 ) ) ;
#7832 = CARTESIAN_POINT ( 'NONE',  ( 118.1852948109119836, -4.153390946401325223, -8.397313243818185668 ) ) ;
#7833 = CYLINDRICAL_SURFACE ( 'NONE', #8286, 5.999999999999997335 ) ;
#7834 = ORIENTED_EDGE ( 'NONE', *, *, #5344, .F. ) ;
#7835 = CARTESIAN_POINT ( 'NONE',  ( 114.7816948109119863, -9.859900752359374465, -12.68260735090039404 ) ) ;
#7836 = FACE_OUTER_BOUND ( 'NONE', #16378, .T. ) ;
#7837 = CARTESIAN_POINT ( 'NONE',  ( 84.39081516114468684, -30.32262605123988664, -11.80406037722653600 ) ) ;
#7838 = CARTESIAN_POINT ( 'NONE',  ( 115.8304577545247582, -7.250697342233347165, -7.631215200338321125 ) ) ;
#7839 = CARTESIAN_POINT ( 'NONE',  ( 115.5191414775786569, -3.383040157471821630, -19.15922257007629170 ) ) ;
#7840 = ORIENTED_EDGE ( 'NONE', *, *, #32648, .T. ) ;
#7841 = CARTESIAN_POINT ( 'NONE',  ( 116.8805814775786445, -6.344957434206662583, -7.627207830600332805 ) ) ;
#7842 = CARTESIAN_POINT ( 'NONE',  ( 90.48265143217095385, -26.32847964148556485, -12.58579976615069818 ) ) ;
#7843 = CARTESIAN_POINT ( 'NONE',  ( 113.8163171295247764, -10.62599879583958540, -13.39321520033831447 ) ) ;
#7844 = CARTESIAN_POINT ( 'NONE',  ( 115.7460481442453357, 0.9020085738987339008, -11.91225656197089222 ) ) ;
#7845 = CARTESIAN_POINT ( 'NONE',  ( 114.7816948109119863, 0.5811942927096154232, -14.16772938898807155 ) ) ;
#7846 = CONICAL_SURFACE ( 'NONE', #4188, 2.000000000000000444, 0.9599310885968830309 ) ;
#7847 = CARTESIAN_POINT ( 'NONE',  ( 126.6827570900308473, -10.09576517521262495, -13.46436818452763973 ) ) ;
#7848 = CARTESIAN_POINT ( 'NONE',  ( 111.9410827545248708, -6.936859964151250502, -8.388885654883788234 ) ) ;
#7849 = CARTESIAN_POINT ( 'NONE',  ( 107.3571765045248299, -2.791137627527939813, -8.388885654883777576 ) ) ;
#7850 = ORIENTED_EDGE ( 'NONE', *, *, #212, .T. ) ;
#7851 = CARTESIAN_POINT ( 'NONE',  ( 112.1609860002551216, -2.334846009198400019, -18.01015021110789149 ) ) ;
#7852 = CARTESIAN_POINT ( 'NONE',  ( 109.2294272264277026, -3.501945941663147099, -18.33763782056176694 ) ) ;
#7853 = CARTESIAN_POINT ( 'NONE',  ( 117.1642148109119859, -0.8288870151387760510, -10.36305467784173118 ) ) ;
#7854 = CARTESIAN_POINT ( 'NONE',  ( 65.55689610126231059, -13.67296395165911704, -12.39321520033831447 ) ) ;
#7855 = CARTESIAN_POINT ( 'NONE',  ( 114.9970202545248412, 0.1403307496149616695, -11.32035403202665336 ) ) ;
#7856 = CARTESIAN_POINT ( 'NONE',  ( 105.9681140045248355, -10.62599879583958717, -11.00651665394454604 ) ) ;
#7857 = DIRECTION ( 'NONE',  ( 0.000000000000000000, -0.9242245927363028635, -0.3818493186865930533 ) ) ;
#7858 = CARTESIAN_POINT ( 'NONE',  ( 114.6682414775786469, -7.894159318335828068, -9.358103419637847864 ) ) ;
#7859 = CARTESIAN_POINT ( 'NONE',  ( 135.6651611124131875, 1.068746826064125965, -12.64546014822358799 ) ) ;
#7860 = CARTESIAN_POINT ( 'NONE',  ( 123.9714148109119805, -0.4660016031367893996, -10.09054647747474043 ) ) ;
#7861 = CARTESIAN_POINT ( 'NONE',  ( 121.6456214775786293, -10.63000616557722466, -14.87417383870573495 ) ) ;
#7863 = ORIENTED_EDGE ( 'NONE', *, *, #29071, .T. ) ;
#7862 = EDGE_CURVE ( 'NONE', #11704, #12164, #42204, .T. ) ;
#7864 = CARTESIAN_POINT ( 'NONE',  ( 117.4478481442453131, -9.565557343593413364, -10.61323700422348004 ) ) ;
#7865 = CARTESIAN_POINT ( 'NONE',  ( 112.2289948109119848, -1.834011780172310813, -8.268836392978581529 ) ) ;
#7866 = CARTESIAN_POINT ( 'NONE',  ( 118.6391081442452986, -4.089484607189486809, -7.948022111789456723 ) ) ;
#7867 = CARTESIAN_POINT ( 'NONE',  ( 120.5678148109119832, -1.833838273342659253, -17.42832698103878286 ) ) ;
#7868 = EDGE_LOOP ( 'NONE', ( #22553, #20354, #32686, #29684, #6228 ) ) ;
#7869 = CARTESIAN_POINT ( 'NONE',  ( 122.8936081442453059, -9.565557343593413364, -10.61323700422348004 ) ) ;
#7870 = CARTESIAN_POINT ( 'NONE',  ( 120.3976348109119812, -1.834011780172310813, -8.268836392978581529 ) ) ;
#7871 = EDGE_CURVE ( 'NONE', #38683, #14232, #23258, .T. ) ;
#7872 = CARTESIAN_POINT ( 'NONE',  ( 136.4644009991209828, 0.4694575037963671926, -15.58432930555171758 ) ) ;
#7873 = CARTESIAN_POINT ( 'NONE',  ( 111.3160046295247838, -4.863998795839590272, -7.631215200338315796 ) ) ;
#7874 = LINE ( 'NONE', #25433, #22792 ) ;
#7875 = CARTESIAN_POINT ( 'NONE',  ( 126.8120025794041652, 0.4302159796464454788, -13.22856333804064732 ) ) ;
#7876 = CARTESIAN_POINT ( 'NONE',  ( 115.8999108795247821, -1.325403438956436419, -16.93181055722141792 ) ) ;
#7877 = CARTESIAN_POINT ( 'NONE',  ( 117.7314814775786260, -4.089484607189486809, -7.948022111789456723 ) ) ;
#7878 = DIRECTION ( 'NONE',  ( 0.5735764363510498232, -0.3127926500124802445, 0.7570804645221007600 ) ) ;
#7879 = CARTESIAN_POINT ( 'NONE',  ( 114.4980614775786734, -2.084020599724406786, -8.691656652584148546 ) ) ;
#7880 = DIRECTION ( 'NONE',  ( 1.000000000000000000, 0.000000000000000000, -0.000000000000000000 ) ) ;
#7881 = CARTESIAN_POINT ( 'NONE',  ( -13.49829988753201881, -3.924578376762261733, -7.963090618125084674 ) ) ;
#7882 = CARTESIAN_POINT ( 'NONE',  ( 109.9963952545248134, -9.868328341294098749, -15.46607636864997204 ) ) ;
#7883 = DIRECTION ( 'NONE',  ( 0.000000000000000000, 0.000000000000000000, 1.000000000000000000 ) ) ;
#7884 = DIRECTION ( 'NONE',  ( -0.2768435750659241079, -0.3568721902840695792, 0.8921882507333129819 ) ) ;
#7886 = CARTESIAN_POINT ( 'NONE',  ( 118.1285681442453068, -7.893985811506177619, -18.51759400769804742 ) ) ;
#7885 = CARTESIAN_POINT ( 'NONE',  ( 64.20808384960839987, -15.18003272038575524, -10.58763554360807646 ) ) ;
#7887 = AXIS2_PLACEMENT_3D ( 'NONE', #12742, #40558, #9318 ) ;
#7888 = CARTESIAN_POINT ( 'NONE',  ( 120.7379948109119709, 0.4262465694468514643, -12.03445270309931736 ) ) ;
#7889 = CARTESIAN_POINT ( 'NONE',  ( 111.4915481442453142, -1.833838273342658365, -17.42832698103878286 ) ) ;
#7890 = ORIENTED_EDGE ( 'NONE', *, *, #16982, .T. ) ;
#7891 = CARTESIAN_POINT ( 'NONE',  ( 137.4282737236246419, -7.497609102793218128, -9.036577839788058952 ) ) ;
#7892 = CARTESIAN_POINT ( 'NONE',  ( 124.7655881442452852, 0.5811942927096110934, -14.16772938898807510 ) ) ;
#7893 = CARTESIAN_POINT ( 'NONE',  ( 113.6774108795247997, -1.325403438956436419, -16.93181055722141792 ) ) ;
#7894 = CARTESIAN_POINT ( 'NONE',  ( 120.2841814775786276, -10.15424416112533912, -14.75197769757731336 ) ) ;
#7895 = CARTESIAN_POINT ( 'NONE',  ( 117.4478481442453131, -9.565557343593413364, -10.61323700422348004 ) ) ;
#7896 = CARTESIAN_POINT ( 'NONE',  ( 86.38598499330589675, -26.29959636144449675, -8.402972644559891791 ) ) ;
#7897 = CARTESIAN_POINT ( 'NONE',  ( 109.3018640045248304, -10.62599879583958717, -11.00651665394454604 ) ) ;
#7898 = CARTESIAN_POINT ( 'NONE',  ( 121.9292548109119849, -7.894159318335828068, -9.358103419637847864 ) ) ;
#7899 = CARTESIAN_POINT ( 'NONE',  ( 125.7299414775786346, -10.15424416112533912, -14.75197769757731336 ) ) ;
#7900 = CARTESIAN_POINT ( 'NONE',  ( 114.8951481442453115, -8.899110576539717599, -16.42337572283489067 ) ) ;
#7901 = CARTESIAN_POINT ( 'NONE',  ( 109.2294671201922966, -5.181012237870030290, -7.812175924317291908 ) ) ;
#7902 = CARTESIAN_POINT ( 'NONE',  ( 121.4103298109119748, -7.200787124940443817, -17.81845355600750835 ) ) ;
#7903 = CARTESIAN_POINT ( 'NONE',  ( 113.1217858795247935, -0.7896495226426338832, -17.46756447353520159 ) ) ;
#7904 = DIRECTION ( 'NONE',  ( 0.000000000000000000, -0.3818493186865927203, 0.9242245927363029745 ) ) ;
#7905 = CARTESIAN_POINT ( 'NONE',  ( 84.10271796608054728, -31.10763468207612092, -21.89321520033831447 ) ) ;
#7906 = CARTESIAN_POINT ( 'NONE',  ( 117.6180281442453150, -0.4660016031367893996, -10.09054647747474043 ) ) ;
#7907 = CARTESIAN_POINT ( 'NONE',  ( 119.6034614775786196, -6.344957434206665248, -7.627207830600338134 ) ) ;
#7908 = CARTESIAN_POINT ( 'NONE',  ( 109.4407702545248355, -10.62599879583958717, -15.77991374673208469 ) ) ;
#7909 = CARTESIAN_POINT ( 'NONE',  ( 112.9097148109120070, 0.2603800115204892296, -16.42320221600525088 ) ) ;
#7910 = ORIENTED_EDGE ( 'NONE', *, *, #7752, .F. ) ;
#7911 = CARTESIAN_POINT ( 'NONE',  ( 61.77615262425602793, -2.025327440714448812, -17.89321520033831447 ) ) ;
#7912 = CARTESIAN_POINT ( 'NONE',  ( 115.6325948109119821, 0.2603800115204892296, -16.42320221600525088 ) ) ;
#7913 = CARTESIAN_POINT ( 'NONE',  ( 120.2274548109119934, -9.859900752359374465, -12.68260735090039404 ) ) ;
#7914 = APPLICATION_PROTOCOL_DEFINITION ( 'draft international standard', 'automotive_design', 1998, #16044 ) ;
#7915 = CARTESIAN_POINT ( 'NONE',  ( 126.2404814775786264, -9.261995988541697145, -16.69588392320189030 ) ) ;
#7916 = CARTESIAN_POINT ( 'NONE',  ( 121.7590748109119687, -7.893985811506177619, -18.51759400769804742 ) ) ;
#7917 = CARTESIAN_POINT ( 'NONE',  ( 111.9410827545248708, -2.477300249445798297, -19.15521520033831138 ) ) ;
#7918 = ADVANCED_FACE ( 'NONE', ( #37681 ), #31256, .T. ) ;
#7919 = CARTESIAN_POINT ( 'NONE',  ( 117.7882081442453170, -3.505236298600246325, -18.68346056562440793 ) ) ;
#7920 = CARTESIAN_POINT ( 'NONE',  ( 121.7575954359119805, -11.07370829466463569, -12.81314460846529002 ) ) ;
#7921 = FACE_OUTER_BOUND ( 'NONE', #16008, .T. ) ;
#7922 = ORIENTED_EDGE ( 'NONE', *, *, #4258, .T. ) ;
#7923 = CARTESIAN_POINT ( 'NONE',  ( 122.1743141859119817, -0.8832429491016019485, -18.19431474523657855 ) ) ;
#7924 = CARTESIAN_POINT ( 'NONE',  ( 119.0929214775786278, -5.638512984488999180, -18.83840828888717311 ) ) ;
#7925 = VERTEX_POINT ( 'NONE', #40891 ) ;
#7926 = CARTESIAN_POINT ( 'NONE',  ( 122.3253830209070259, -6.157706758239399392, -18.56290235964623392 ) ) ;
#7927 = CARTESIAN_POINT ( 'NONE',  ( -12.52970885032985748, -4.316676466568440063, -7.393215200338314474 ) ) ;
#7928 = CYLINDRICAL_SURFACE ( 'NONE', #24522, 0.4999999999999970024 ) ;
#7929 = CARTESIAN_POINT ( 'NONE',  ( 117.5613014775786525, -10.15424416112533912, -14.75197769757731336 ) ) ;
#7930 = DIRECTION ( 'NONE',  ( -0.9609149988134837450, 0.1028163501681639419, -0.2570431154366518145 ) ) ;
#7931 = CARTESIAN_POINT ( 'NONE',  ( 86.36631847702263087, -25.23119213852205789, -15.24166438581092109 ) ) ;
#7932 = CARTESIAN_POINT ( 'NONE',  ( 119.5467348109119712, -5.574606645277164318, -18.38911715685844683 ) ) ;
#7933 = CARTESIAN_POINT ( 'NONE',  ( 68.80767435282035649, -72.12455157026508346, -36.87789895383100003 ) ) ;
#7934 = CARTESIAN_POINT ( 'NONE',  ( 121.3052614775786111, -7.643976991954077427, -18.09477374809248928 ) ) ;
#7935 = CARTESIAN_POINT ( 'NONE',  ( 124.9542645564618510, -12.06356186585028745, -10.89038081117960033 ) ) ;
#7936 = CARTESIAN_POINT ( 'NONE',  ( 123.5176014775786228, -0.8288870151387760510, -10.36305467784173118 ) ) ;
#7937 = CARTESIAN_POINT ( 'NONE',  ( 114.7249681442453237, 0.2603800115204892296, -16.42320221600525088 ) ) ;
#7938 = CARTESIAN_POINT ( 'NONE',  ( 119.3198281442452924, 0.5811942927096110934, -14.16772938898807510 ) ) ;
#7939 = CARTESIAN_POINT ( 'NONE',  ( 111.9453614775786434, -1.561330072975668060, -17.79121239304076596 ) ) ;
#7940 = LINE ( 'NONE', #8173, #40186 ) ;
#7941 = CARTESIAN_POINT ( 'NONE',  ( 121.0216281442452981, -7.894159318335828068, -9.358103419637847864 ) ) ;
#7942 = VERTEX_POINT ( 'NONE', #16493 ) ;
#7943 = CARTESIAN_POINT ( 'NONE',  ( 118.8092881442453290, -9.988377603198976828, -10.36322818467138340 ) ) ;
#7944 = CARTESIAN_POINT ( 'NONE',  ( 113.0523327545247838, -6.936859964151250502, -8.388885654883777576 ) ) ;
#7945 = CARTESIAN_POINT ( 'NONE',  ( 69.69189222815028018, -41.76310523276638520, -16.39321520033831447 ) ) ;
#7946 = CARTESIAN_POINT ( 'NONE',  ( 114.1635827545248247, -6.936859964151250502, -8.388885654883788234 ) ) ;
#7947 = AXIS2_PLACEMENT_3D ( 'NONE', #21368, #619, #42355 ) ;
#7948 = DIRECTION ( 'NONE',  ( -0.000000000000000000, -0.9284778069183721172, -0.3713878862591650232 ) ) ;
#7949 = CARTESIAN_POINT ( 'NONE',  ( 125.6732148109119862, 0.5811942927096110934, -14.16772938898807510 ) ) ;
#7950 = ORIENTED_EDGE ( 'NONE', *, *, #767, .T. ) ;
#7951 = DIRECTION ( 'NONE',  ( 0.000000000000000000, 0.000000000000000000, 1.000000000000000000 ) ) ;
#7952 = CIRCLE ( 'NONE', #12325, 2.000000000000001776 ) ;
#7953 = CARTESIAN_POINT ( 'NONE',  ( 122.2128881442453263, -7.643976991954077427, -18.09477374809248928 ) ) ;
#7954 = CARTESIAN_POINT ( 'NONE',  ( 120.5074391859119913, -8.844754642576884152, -8.592115655440050404 ) ) ;
#7955 = CARTESIAN_POINT ( 'NONE',  ( 59.75121349346654398, -13.58877957849836093, -19.38162691376808411 ) ) ;
#7956 = CARTESIAN_POINT ( 'NONE',  ( 125.7299414775786346, 0.9020085738987339008, -11.91225656197089222 ) ) ;
#7957 = CARTESIAN_POINT ( 'NONE',  ( 108.7462390045248242, -9.868328341294098749, -11.32035403202665869 ) ) ;
#7958 = ORIENTED_EDGE ( 'NONE', *, *, #32029, .T. ) ;
#7959 = CARTESIAN_POINT ( 'NONE',  ( 115.4056881442453459, -7.893985811506177619, -18.51759400769804742 ) ) ;
#7960 = CARTESIAN_POINT ( 'NONE',  ( 113.5337081442453240, -9.261995988541697145, -16.69588392320189030 ) ) ;
#7961 = CARTESIAN_POINT ( 'NONE',  ( 88.28425963449630842, -11.60945497031996787, -13.33030055912934486 ) ) ;
#7962 = CARTESIAN_POINT ( 'NONE',  ( 121.1918081442452859, -10.15424416112533912, -14.75197769757731336 ) ) ;
#7963 = CARTESIAN_POINT ( 'NONE',  ( 116.9582927111058552, -1.267766418764730840, -16.93314635290706605 ) ) ;
#7964 = PRODUCT_DEFINITION ( 'UNKNOWN', '', #12593, #10563 ) ;
#7965 =( LENGTH_UNIT ( ) NAMED_UNIT ( * ) SI_UNIT ( .MILLI., .METRE. ) );
#7966 = CARTESIAN_POINT ( 'NONE',  ( 122.1561614775786353, -0.4660016031367893996, -10.09054647747474043 ) ) ;
#7967 = CARTESIAN_POINT ( 'NONE',  ( 123.6310548109119765, -4.153390946401271933, -8.397313243818190998 ) ) ;
#7968 = B_SPLINE_CURVE_WITH_KNOTS ( 'NONE', 3,
 ( #27935, #21076, #28826, #38609, #39305, #8076, #21977, #554, #34953, #3739, #14239, #42066, #10823, #24721 ),
 .UNSPECIFIED., .F., .F.,
 ( 4, 2, 2, 2, 2, 2, 4 ),
 ( 6.938893903907228378E-18, 0.001308732638115193449, 0.001963098957172786704, 0.002617465276230379959, 0.003271831595287972780, 0.003926197914345566468, 0.005234930552460722621 ),
 .UNSPECIFIED. ) ;
#7969 = LINE ( 'NONE', #671, #39773 ) ;
#7970 = FACE_OUTER_BOUND ( 'NONE', #16976, .T. ) ;
#7971 = SURFACE_STYLE_USAGE ( .BOTH. , #28953 ) ;
#7972 = VERTEX_POINT ( 'NONE', #33558 ) ;
#7973 = FACE_OUTER_BOUND ( 'NONE', #19915, .T. ) ;
#7974 = CARTESIAN_POINT ( 'NONE',  ( 119.8870948109119752, -9.261995988541697145, -16.69588392320189030 ) ) ;
#7975 = CARTESIAN_POINT ( 'NONE',  ( 65.70844687201810075, -0.1919082892013201924, -16.07106790048558054 ) ) ;
#7976 = EDGE_LOOP ( 'NONE', ( #20057, #10055, #41376, #11804 ) ) ;
#7977 = CARTESIAN_POINT ( 'NONE',  ( 111.8886348109120092, -3.383040157471821630, -19.15922257007629170 ) ) ;
#7978 = CARTESIAN_POINT ( 'NONE',  ( 126.0703014775786102, -9.988377603198980381, -10.36322818467138518 ) ) ;
#7979 = DIRECTION ( 'NONE',  ( -0.8636456077245080465, 0.5040994586965603652, 0.000000000000000000 ) ) ;
#7980 = CARTESIAN_POINT ( 'NONE',  ( 123.9146881442452894, -10.15424416112533912, -14.75197769757731336 ) ) ;
#7981 = EDGE_LOOP ( 'NONE', ( #4086, #3955, #44211, #39839, #37228 ) ) ;
#7982 = CARTESIAN_POINT ( 'NONE',  ( 117.6747548109119919, -1.834011780172310813, -8.268836392978581529 ) ) ;
#7983 = CIRCLE ( 'NONE', #27667, 0.5000000000000004441 ) ;
#7984 = CARTESIAN_POINT ( 'NONE',  ( 116.5034398309151129, -2.215723800389698184, -18.16877924232191788 ) ) ;
#7985 = CARTESIAN_POINT ( 'NONE',  ( 70.19189222814998175, -100.0979043305785581, -53.24182196210380624 ) ) ;
#7986 = CARTESIAN_POINT ( 'NONE',  ( 137.3019930433568447, -4.908147610492624935, -8.177672544428061130 ) ) ;
#7987 = CARTESIAN_POINT ( 'NONE',  ( 126.0703014775786102, -9.988377603198980381, -10.36322818467138518 ) ) ;
#7988 = CARTESIAN_POINT ( 'NONE',  ( 72.30589087944665039, -67.07702721507251908, -42.22679270393576445 ) ) ;
#7989 = CIRCLE ( 'NONE', #24127, 2.000000000000000444 ) ;
#7990 = FACE_OUTER_BOUND ( 'NONE', #2760, .T. ) ;
#7991 = CARTESIAN_POINT ( 'NONE',  ( 123.2906948109119867, -8.166667518702819706, -8.995218007635861213 ) ) ;
#7992 = CARTESIAN_POINT ( 'NONE',  ( 123.6310548109119765, -4.153390946401325223, -8.397313243818185668 ) ) ;
#7993 = CARTESIAN_POINT ( 'NONE',  ( 116.6749492131033747, -8.511528440524470440, -16.92981788454075698 ) ) ;
#7994 = CARTESIAN_POINT ( 'NONE',  ( 124.5386814775786206, -4.153390946401325223, -8.397313243818185668 ) ) ;
#7995 = CARTESIAN_POINT ( 'NONE',  ( 112.7962614775786676, -6.222761293078241884, -8.102969835052219238 ) ) ;
#7996 = CARTESIAN_POINT ( 'NONE',  ( 121.1918081442452859, 0.9020085738987339008, -11.91225656197089222 ) ) ;
#7997 = ORIENTED_EDGE ( 'NONE', *, *, #1177, .T. ) ;
#7998 = VERTEX_POINT ( 'NONE', #26524 ) ;
#7999 = DIRECTION ( 'NONE',  ( -0.9908103287288504424, 0.1352586133457951423, 0.000000000000000000 ) ) ;
#8000 = CARTESIAN_POINT ( 'NONE',  ( 115.6220983795247861, -0.7896495226426338832, -9.318865927141430916 ) ) ;
#8001 = CARTESIAN_POINT ( 'NONE',  ( 115.8304577545247582, -2.791137627527939813, -18.39754474579286025 ) ) ;
#8002 = CARTESIAN_POINT ( 'NONE',  ( 114.0941296295247867, -4.863998795839590272, -8.388885654883775800 ) ) ;
#8003 = CARTESIAN_POINT ( 'NONE',  ( 126.2184548109105435, -9.814174330883648878, -12.68911139247483710 ) ) ;
#8004 = CARTESIAN_POINT ( 'NONE',  ( 114.0442481442453300, -1.834011780172310813, -8.268836392978581529 ) ) ;
#8005 = ORIENTED_EDGE ( 'NONE', *, *, #40657, .T. ) ;
#8006 = CARTESIAN_POINT ( 'NONE',  ( 111.3213681442453264, -7.643976991954077427, -18.09477374809248928 ) ) ;
#8007 = CARTESIAN_POINT ( 'NONE',  ( 106.2459265045248173, -7.250697342233347165, -19.15521520033831138 ) ) ;
#8008 = DIRECTION ( 'NONE',  ( -0.000000000000000000, -0.9284778069183720062, -0.3713878862591650232 ) ) ;
#8009 = CARTESIAN_POINT ( 'NONE',  ( 112.2289948109119848, -7.643976991954077427, -18.09477374809248928 ) ) ;
#8010 = EDGE_CURVE ( 'NONE', #18562, #32667, #21070, .T. ) ;
#8011 = ADVANCED_FACE ( 'NONE', ( #12626 ), #34280, .T. ) ;
#8012 = DIRECTION ( 'NONE',  ( 0.3445294493088594256, 0.9387755102040817867, 0.000000000000000000 ) ) ;
#8013 = DIRECTION ( 'NONE',  ( 0.000000000000000000, 0.6004852223388321697, -0.7996358532186279566 ) ) ;
#8014 = CARTESIAN_POINT ( 'NONE',  ( 116.3700414775786527, -5.638512984488999180, -18.83840828888717311 ) ) ;
#8015 = CARTESIAN_POINT ( 'NONE',  ( 113.3995983795247895, -0.7896495226426338832, -9.318865927141430916 ) ) ;
#8016 = CARTESIAN_POINT ( 'NONE',  ( 113.4690515045247992, -6.936859964151250502, -18.39754474579286025 ) ) ;
#8017 = EDGE_LOOP ( 'NONE', ( #35997, #5690, #12699 ) ) ;
#8018 = CARTESIAN_POINT ( 'NONE',  ( 126.4750299824229671, -7.440601375365601733, -8.959200753400851980 ) ) ;
#8019 = CARTESIAN_POINT ( 'NONE',  ( 119.8870948109119752, -0.8288870151387760510, -10.36305467784173118 ) ) ;
#8020 = CARTESIAN_POINT ( 'NONE',  ( 114.3846081442453197, -10.63000616557722466, -14.87417383870573495 ) ) ;
#8021 = AXIS2_PLACEMENT_3D ( 'NONE', #19169, #39694, #18722 ) ;
#8022 = DIRECTION ( 'NONE',  ( 0.000000000000000000, -0.9284778069183722282, -0.3713878862591645791 ) ) ;
#8023 = CARTESIAN_POINT ( 'NONE',  ( 121.9470836909669913, -25.99489077589524300, -13.39321520033831447 ) ) ;
#8024 = CARTESIAN_POINT ( 'NONE',  ( 120.2841814775786276, -10.15424416112533912, -14.75197769757731336 ) ) ;
#8025 = CARTESIAN_POINT ( 'NONE',  ( 115.7460481442453357, -10.15424416112533912, -14.75197769757731336 ) ) ;
#8026 = ORIENTED_EDGE ( 'NONE', *, *, #25222, .F. ) ;
#8027 = CARTESIAN_POINT ( 'NONE',  ( 122.3132204359119868, -10.25716656981731489, -12.88942061488890545 ) ) ;
#8028 = CIRCLE ( 'NONE', #24057, 2.999999999999999556 ) ;
#8029 = CARTESIAN_POINT ( 'NONE',  ( 75.95778847736481509, -3.256761025687722189, -7.993215200338315007 ) ) ;
#8030 = CARTESIAN_POINT ( 'NONE',  ( 117.3343948109119737, -6.222761293078241884, -8.102969835052219238 ) ) ;
#8031 = ORIENTED_EDGE ( 'NONE', *, *, #8110, .F. ) ;
#8032 = AXIS2_PLACEMENT_3D ( 'NONE', #7767, #28749, #43099 ) ;
#8033 = CARTESIAN_POINT ( 'NONE',  ( 127.3434826497788492, -9.951987873813537888, -15.64804239197681035 ) ) ;
#8034 = B_SPLINE_CURVE_WITH_KNOTS ( 'NONE', 3,
 ( #19318, #26157, #12485, #13555, #6932, #20401, #9059, #12262, #33203, #45020, #34501, #38157, #15903, #43494, #34285, #23829, #44571, #43716, #37716, #5620, #13778, #41155, #20177, #27689, #41603, #6486, #40295, #8826, #22959, #27465, #20839, #3057, #36852, #22729, #34061, #10362 ),
 .UNSPECIFIED., .F., .F.,
 ( 4, 2, 2, 2, 2, 1, 2, 2, 2, 2, 2, 2, 2, 1, 2, 2, 2, 2, 4 ),
 ( 0.000000000000000000, 0.06249999999995659028, 0.1249999999999131806, 0.1874999999998697708, 0.2187499999998515632, 0.2343749999998424594, 0.2421874999998402667, 0.2499999999998380740, 0.3749999999998612221, 0.4999999999998843148, 0.6249999999999074074, 0.6874999999999189537, 0.7187499999999243938, 0.7343749999999275024, 0.7421874999999237277, 0.7499999999999199529, 0.8124999999999399369, 0.8749999999999599209, 1.000000000000000000 ),
 .UNSPECIFIED. ) ;
#8035 = CARTESIAN_POINT ( 'NONE',  ( 113.4202548109119846, -10.30919188438810075, -12.61870101168855918 ) ) ;
#8036 = CARTESIAN_POINT ( 'NONE',  ( 116.2471765045247594, -7.250697342233347165, -19.15521520033831138 ) ) ;
#8037 = CARTESIAN_POINT ( 'NONE',  ( 112.9664414775786412, -9.859900752359374465, -12.68260735090039404 ) ) ;
#8038 = EDGE_CURVE ( 'NONE', #38783, #19531, #27631, .T. ) ;
#8039 = EDGE_LOOP ( 'NONE', ( #28305, #29492, #32787, #16315, #1338, #37364, #44950, #36108, #10743, #30641, #8524 ) ) ;
#8040 = ORIENTED_EDGE ( 'NONE', *, *, #7045, .T. ) ;
#8041 = CARTESIAN_POINT ( 'NONE',  ( 121.0216281442452981, -7.894159318335828068, -9.358103419637847864 ) ) ;
#8042 = CARTESIAN_POINT ( 'NONE',  ( 118.3554748109119998, -9.565557343593413364, -10.61323700422348004 ) ) ;
#8043 = DIRECTION ( 'NONE',  ( -0.5735764363510450492, -0.3127926500124816878, 0.7570804645221038687 ) ) ;
#8044 = EDGE_CURVE ( 'NONE', #15763, #35799, #31323, .T. ) ;
#8045 = CARTESIAN_POINT ( 'NONE',  ( 120.7157985609119635, -10.36940331770106916, -15.09355782777062061 ) ) ;
#8046 = ORIENTED_EDGE ( 'NONE', *, *, #2612, .T. ) ;
#8047 = CARTESIAN_POINT ( 'NONE',  ( 112.1294530610591380, -8.919641830227062584, -16.32749078332169290 ) ) ;
#8048 = CARTESIAN_POINT ( 'NONE',  ( 123.9584548109119737, -2.421111938423274879, -5.775321541204940345 ) ) ;
#8049 = ADVANCED_FACE ( 'NONE', ( #23842 ), #17652, .T. ) ;
#8050 = CARTESIAN_POINT ( 'NONE',  ( 113.1912390045248031, 0.8980012041604421569, -15.77991374673208469 ) ) ;
#8051 = CIRCLE ( 'NONE', #2939, 18.00000000000000000 ) ;
#8052 = CARTESIAN_POINT ( 'NONE',  ( 112.4559014775786494, -9.988377603198976828, -10.36322818467138340 ) ) ;
#8053 = CARTESIAN_POINT ( 'NONE',  ( 126.2404814775786264, -0.8288870151387760510, -10.36305467784173118 ) ) ;
#8054 =( BOUNDED_CURVE ( )  B_SPLINE_CURVE ( 2, ( #27374, #41296, #10494, #37395, #16665, #30789, #6402, #6620, #17336, #30338, #20533, #24178, #44263 ),
 .UNSPECIFIED., .F., .T. ) 
 B_SPLINE_CURVE_WITH_KNOTS ( ( 3, 2, 2, 2, 2, 2, 3 ),
 ( 0.8296282416568590001, 0.8359375000000000000, 0.8437500000000000000, 0.8515625000000000000, 0.8593750000000000000, 0.8671875000000000000, 0.8750000000000000000 ),
 .UNSPECIFIED. ) 
 CURVE ( )  GEOMETRIC_REPRESENTATION_ITEM ( )  RATIONAL_B_SPLINE_CURVE ( ( 0.9763430640195970289, 0.9385262470928680267, 1.000000000000000000, 0.9238795325112869605, 1.000000000000000000, 0.9238795325112869605, 1.000000000000000000, 0.9238795325112869605, 1.000000000000000000, 0.9238795325112869605, 1.000000000000000000, 0.9238795325112669765, 1.000000000000019984 ) ) 
 REPRESENTATION_ITEM ( '' )  );
#8055 = CARTESIAN_POINT ( 'NONE',  ( 120.1140014775786398, -7.894159318335828068, -9.358103419637847864 ) ) ;
#8056 = LINE ( 'NONE', #29031, #42250 ) ;
#8057 = ORIENTED_EDGE ( 'NONE', *, *, #17794, .F. ) ;
#8058 = CARTESIAN_POINT ( 'NONE',  ( 120.9649014775786355, -6.222761293078241884, -8.102969835052219238 ) ) ;
#8059 = EDGE_CURVE ( 'NONE', #36514, #37519, #6499, .T. ) ;
#8060 = FACE_OUTER_BOUND ( 'NONE', #5337, .T. ) ;
#8061 = AXIS2_PLACEMENT_3D ( 'NONE', #29277, #35877, #36326 ) ;
#8062 = DIRECTION ( 'NONE',  ( 0.000000000000000000, 0.000000000000000000, 1.000000000000000000 ) ) ;
#8063 = CARTESIAN_POINT ( 'NONE',  ( 114.7192077545248594, -7.250697342233347165, -7.631215200338321125 ) ) ;
#8064 = CARTESIAN_POINT ( 'NONE',  ( 113.9307948109119906, 0.9020085738987339008, -11.91225656197089222 ) ) ;
#8065 = ORIENTED_EDGE ( 'NONE', *, *, #31406, .T. ) ;
#8066 = VECTOR ( 'NONE', #26358, 1000.000000000000114 ) ;
#8067 = EDGE_CURVE ( 'NONE', #42470, #42269, #17000, .T. ) ;
#8068 = CARTESIAN_POINT ( 'NONE',  ( 116.3700414775786527, -5.638512984488999180, -18.83840828888717311 ) ) ;
#8069 = CARTESIAN_POINT ( 'NONE',  ( 63.04939936085997232, -37.71678474238356671, -4.998464946505073669 ) ) ;
#8070 = CARTESIAN_POINT ( 'NONE',  ( 110.2047546295247855, -4.863998795839590272, -7.631215200338315796 ) ) ;
#8071 = CARTESIAN_POINT ( 'NONE',  ( 115.4624148109119943, -5.638512984488999180, -18.83840828888717311 ) ) ;
#8072 = EDGE_CURVE ( 'NONE', #37642, #35430, #22535, .T. ) ;
#8073 = ADVANCED_FACE ( 'NONE', ( #38382 ), #21065, .T. ) ;
#8074 = CARTESIAN_POINT ( 'NONE',  ( 118.5256548109119876, -0.4660016031367893996, -10.09054647747474043 ) ) ;
#8075 = CARTESIAN_POINT ( 'NONE',  ( 125.5597614775786326, -7.894159318335828068, -9.358103419637847864 ) ) ;
#8076 = CARTESIAN_POINT ( 'NONE',  ( 62.16677121967738628, -14.49431128105000610, -17.68377221324302795 ) ) ;
#8077 = DIRECTION ( 'NONE',  ( 1.000000000000000000, 0.000000000000000000, -0.000000000000000000 ) ) ;
#8078 = ORIENTED_EDGE ( 'NONE', *, *, #41778, .F. ) ;
#8079 = CARTESIAN_POINT ( 'NONE',  ( 111.2647102085435193, -8.897589485953298905, -16.42540022429002633 ) ) ;
#8080 = CARTESIAN_POINT ( 'NONE',  ( 109.2294421468926799, -10.01755377227571664, -11.02232003854844145 ) ) ;
#8081 = CARTESIAN_POINT ( 'NONE',  ( 118.8092881442453290, -0.1624402480850797581, -16.17319339645315424 ) ) ;
#8082 = CARTESIAN_POINT ( 'NONE',  ( 112.0105358795247810, -8.402594152722688392, -9.854619843455216355 ) ) ;
#8083 = CARTESIAN_POINT ( 'NONE',  ( 107.0099108795247815, -8.938348069036489818, -9.318865927141430916 ) ) ;
#8084 = CARTESIAN_POINT ( 'NONE',  ( 127.0400190879719986, -5.168639390464125682, -7.991015206380699176 ) ) ;
#8085 = CARTESIAN_POINT ( 'NONE',  ( 115.2922348109119781, 0.4262465694468514643, -12.03445270309931736 ) ) ;
#8086 = CARTESIAN_POINT ( 'NONE',  ( 31.33087284928346605, -19.31933043625825874, -18.19321520033831519 ) ) ;
#8087 = CARTESIAN_POINT ( 'NONE',  ( 122.7234281442452755, -5.638512984488999180, -18.83840828888717311 ) ) ;
#8088 = CARTESIAN_POINT ( 'NONE',  ( 118.5823814775786360, -1.834011780172310813, -8.268836392978581529 ) ) ;
#8089 = VERTEX_POINT ( 'NONE', #7155 ) ;
#8090 = CARTESIAN_POINT ( 'NONE',  ( 116.9373081442452929, -1.833838273342659253, -17.42832698103878286 ) ) ;
#8091 = DIRECTION ( 'NONE',  ( 1.000000000000000000, 0.000000000000000000, -0.000000000000000000 ) ) ;
#8092 = AXIS2_PLACEMENT_3D ( 'NONE', #36426, #1771, #1548 ) ;
#8093 = CARTESIAN_POINT ( 'NONE',  ( 117.4478481442453131, 0.2603800115204892296, -16.42320221600525088 ) ) ;
#8094 = CARTESIAN_POINT ( 'NONE',  ( 118.8092881442453290, -0.1624402480850797581, -16.17319339645315424 ) ) ;
#8095 = ORIENTED_EDGE ( 'NONE', *, *, #37552, .T. ) ;
#8096 = CARTESIAN_POINT ( 'NONE',  ( 124.4819548109119722, -2.084020599724406786, -8.691656652584148546 ) ) ;
#8097 = CIRCLE ( 'NONE', #5901, 2.000000000000000444 ) ;
#8098 = CARTESIAN_POINT ( 'NONE',  ( 120.2841814775786276, 0.9020085738987339008, -11.91225656197089222 ) ) ;
#8099 = CARTESIAN_POINT ( 'NONE',  ( 122.6009548109119720, -3.874292970208447873, -21.33175929725637587 ) ) ;
#8100 = CARTESIAN_POINT ( 'NONE',  ( 109.0935046295247872, -4.863998795839590272, -7.631215200338315796 ) ) ;
#8101 = AXIS2_PLACEMENT_3D ( 'NONE', #19558, #30045, #43961 ) ;
#8102 = DIRECTION ( 'NONE',  ( -0.9609149988134836340, 0.1028163501681645525, -0.2570431154366521476 ) ) ;
#8103 = CARTESIAN_POINT ( 'NONE',  ( 127.5540300678602819, 0.7775483060884187392, -12.84556817354802760 ) ) ;
#8104 = CARTESIAN_POINT ( 'NONE',  ( 112.9134265045247645, -2.791137627527939813, -8.388885654883777576 ) ) ;
#8105 = CARTESIAN_POINT ( 'NONE',  ( 119.4900081442453086, -1.834011780172310813, -8.268836392978581529 ) ) ;
#8106 = CARTESIAN_POINT ( 'NONE',  ( 137.2618751060949762, -9.878515410958410570, -11.82152439363173357 ) ) ;
#8107 = CARTESIAN_POINT ( 'NONE',  ( 115.8595014775786609, -7.643976991954077427, -18.09477374809248928 ) ) ;
#8108 = CARTESIAN_POINT ( 'NONE',  ( 111.9453614775786434, -7.894159318335828068, -9.358103419637847864 ) ) ;
#8109 = CARTESIAN_POINT ( 'NONE',  ( 126.2275303246276934, -0.7934555298964990344, -10.48169931380525632 ) ) ;
#8110 = EDGE_CURVE ( 'NONE', #26941, #10499, #24282, .T. ) ;
#8111 = CARTESIAN_POINT ( 'NONE',  ( 117.7314814775786260, -5.574606645277192740, -18.38911715685844328 ) ) ;
#8112 = CARTESIAN_POINT ( 'NONE',  ( 108.5378796295247810, -4.863998795839590272, -8.388885654883775800 ) ) ;
#8113 = CARTESIAN_POINT ( 'NONE',  ( 122.2897060817262513, -2.423081321603731908, -17.89265170041263175 ) ) ;
#8114 = CARTESIAN_POINT ( 'NONE',  ( 112.8337832127138682, -2.191907684172563986, -18.20049396185734025 ) ) ;
#8115 = AXIS2_PLACEMENT_3D ( 'NONE', #35299, #4071, #17995 ) ;
#8116 = LINE ( 'NONE', #43221, #36941 ) ;
#8118 = CARTESIAN_POINT ( 'NONE',  ( 118.9227414775786400, -10.63000616557722466, -14.87417383870573495 ) ) ;
#8117 = CARTESIAN_POINT ( 'NONE',  ( 62.28506180665693392, -13.31920281343605339, -7.834338051647534940 ) ) ;
#8119 = CARTESIAN_POINT ( 'NONE',  ( 119.4332814775786318, -8.899110576539710493, -16.42337572283490132 ) ) ;
#8120 = CARTESIAN_POINT ( 'NONE',  ( 113.8740681442453138, -9.859900752359374465, -12.68260735090039404 ) ) ;
#8121 = EDGE_LOOP ( 'NONE', ( #15938, #41978 ) ) ;
#8122 = CARTESIAN_POINT ( 'NONE',  ( 137.1799701741868205, -8.769776793597710451, -9.774222394608035103 ) ) ;
#8123 = CARTESIAN_POINT ( 'NONE',  ( 121.9859814775786333, 0.2603800115204892296, -16.42320221600525088 ) ) ;
#8124 = CARTESIAN_POINT ( 'NONE',  ( 115.3442858795247759, -8.402594152722688392, -9.854619843455216355 ) ) ;
#8125 = CARTESIAN_POINT ( 'NONE',  ( 117.8449348109119938, -1.833838273342659253, -17.42832698103878286 ) ) ;
#8126 = CARTESIAN_POINT ( 'NONE',  ( 121.5888948109119809, 0.1319031606808879209, -14.10382304977623669 ) ) ;
#8127 = CARTESIAN_POINT ( 'NONE',  ( 117.7882081442453170, -3.505236298600246325, -18.68346056562440793 ) ) ;
#8128 = CARTESIAN_POINT ( 'NONE',  ( 123.9584548109119737, 2.753894863294152007, -15.83610205775420177 ) ) ;
#8129 = CARTESIAN_POINT ( 'NONE',  ( 106.4542858795248179, -0.7896495226426338832, -17.46756447353520159 ) ) ;
#8130 = CARTESIAN_POINT ( 'NONE',  ( 124.7088614775786226, -9.565557343593413364, -10.61323700422348004 ) ) ;
#8131 = VECTOR ( 'NONE', #44261, 1000.000000000000000 ) ;
#8132 = CARTESIAN_POINT ( 'NONE',  ( 122.3830681442452857, -1.833838273342659697, -17.42832698103878286 ) ) ;
#8133 = CARTESIAN_POINT ( 'NONE',  ( 116.0829010812576882, -0.01829820670803256055, -12.14321520033834290 ) ) ;
#8134 = CARTESIAN_POINT ( 'NONE',  ( 70.19189222814998175, -56.12358456014947450, -35.65224734057483857 ) ) ;
#8135 = CARTESIAN_POINT ( 'NONE',  ( 119.5350954359119839, 0.5291689781388270175, -13.89700978578772705 ) ) ;
#8136 = CARTESIAN_POINT ( 'NONE',  ( 115.6220983795247861, -0.7896495226426338832, -9.318865927141430916 ) ) ;
#8137 = CARTESIAN_POINT ( 'NONE',  ( 116.7648838078721525, 2.033349373364758961, -20.84824896580845177 ) ) ;
#8138 = CARTESIAN_POINT ( 'NONE',  ( 83.88969763788190903, -31.68807350287827163, -22.38302129830086784 ) ) ;
#8139 = CARTESIAN_POINT ( 'NONE',  ( 118.0151148109119816, -10.63000616557722466, -14.87417383870573495 ) ) ;
#8140 = CARTESIAN_POINT ( 'NONE',  ( 118.9227414775786400, -10.63000616557722466, -14.87417383870573495 ) ) ;
#8141 = DIRECTION ( 'NONE',  ( 0.000000000000000000, 0.000000000000000000, -1.000000000000000000 ) ) ;
#8142 = EDGE_CURVE ( 'NONE', #30086, #33919, #40989, .T. ) ;
#8143 = CARTESIAN_POINT ( 'NONE',  ( 113.8173414775786512, 0.2603800115204892296, -16.42320221600525088 ) ) ;
#8144 = ORIENTED_EDGE ( 'NONE', *, *, #20311, .F. ) ;
#8145 = CARTESIAN_POINT ( 'NONE',  ( 116.5944421295247793, -9.863109299026486809, -13.29890625629612622 ) ) ;
#8146 = CARTESIAN_POINT ( 'NONE',  ( 116.3133148109119759, -7.893985811506177619, -18.51759400769804742 ) ) ;
#8147 = CARTESIAN_POINT ( 'NONE',  ( 121.0216281442452981, -7.894159318335828068, -9.358103419637847864 ) ) ;
#8148 = CARTESIAN_POINT ( 'NONE',  ( 113.5904348109119866, -2.084020599724406786, -8.691656652584148546 ) ) ;
#8149 = CARTESIAN_POINT ( 'NONE',  ( 121.8725281442453223, -3.383040157471821630, -19.15922257007629170 ) ) ;
#8150 = CARTESIAN_POINT ( 'NONE',  ( 115.5526452545247622, 0.8980012041604421569, -11.00651665394454071 ) ) ;
#8151 = AXIS2_PLACEMENT_3D ( 'NONE', #40976, #11239, #31751 ) ;
#8152 = CARTESIAN_POINT ( 'NONE',  ( 115.2355081442453155, 0.1319031606808879209, -14.10382304977623669 ) ) ;
#8153 = CARTESIAN_POINT ( 'NONE',  ( 121.9659548109119811, -7.554583864224885481, -18.48844787311982785 ) ) ;
#8154 = DIRECTION ( 'NONE',  ( -1.000000000000000000, 0.000000000000000000, 0.000000000000000000 ) ) ;
#8155 = ORIENTED_EDGE ( 'NONE', *, *, #2158, .F. ) ;
#8156 = CARTESIAN_POINT ( 'NONE',  ( 122.0354079359119908, -5.444069387712269226, -19.60292469916370450 ) ) ;
#8157 = CARTESIAN_POINT ( 'NONE',  ( 121.1350814775786233, 0.5811942927096110934, -14.16772938898807510 ) ) ;
#8158 = ORIENTED_EDGE ( 'NONE', *, *, #35297, .F. ) ;
#8159 = CARTESIAN_POINT ( 'NONE',  ( 125.7866681442452688, -8.899110576539710493, -16.42337572283490132 ) ) ;
#8160 = CARTESIAN_POINT ( 'NONE',  ( -13.88569750198904806, -4.361307444782807075, -8.573647932902863644 ) ) ;
#8161 = CARTESIAN_POINT ( 'NONE',  ( 70.19189222814998175, -100.0979043305785581, -53.24182196210380624 ) ) ;
#8162 = CARTESIAN_POINT ( 'NONE',  ( 114.6682414775786469, -7.894159318335828068, -9.358103419637847864 ) ) ;
#8163 = CARTESIAN_POINT ( 'NONE',  ( 66.82983677891284913, -0.05992252863833068266, -16.39321520033831803 ) ) ;
#8164 = CARTESIAN_POINT ( 'NONE',  ( 123.7253032127138397, -2.191907684172563986, -18.20049396185734025 ) ) ;
#8165 = CARTESIAN_POINT ( 'NONE',  ( 123.4041481442452834, 0.1319031606808879209, -14.10382304977623669 ) ) ;
#8166 = CARTESIAN_POINT ( 'NONE',  ( 111.7184548109119788, -9.162420673101799196, -15.99582338542316151 ) ) ;
#8167 = CARTESIAN_POINT ( 'NONE',  ( 120.9649014775786355, -6.222761293078241884, -8.102969835052219238 ) ) ;
#8168 = DIRECTION ( 'NONE',  ( -0.000000000000000000, -0.9284778069183718952, -0.3713878862591649677 ) ) ;
#8169 = CARTESIAN_POINT ( 'NONE',  ( 123.3474214775786209, -0.1624402480850797581, -16.17319339645315424 ) ) ;
#8170 = CARTESIAN_POINT ( 'NONE',  ( 113.9307948109119906, 0.9020085738987339008, -11.91225656197089222 ) ) ;
#8171 = CARTESIAN_POINT ( 'NONE',  ( 120.9649014775786355, -3.383040157471821630, -19.15922257007629170 ) ) ;
#8172 = CARTESIAN_POINT ( 'NONE',  ( 113.7606148109119886, -1.561330072975668060, -17.79121239304076596 ) ) ;
#8173 = CARTESIAN_POINT ( 'NONE',  ( 143.3676850761856940, -69.76310523276724496, -32.79321520033831661 ) ) ;
#8174 = CARTESIAN_POINT ( 'NONE',  ( 121.3619881442452879, -5.574606645277164318, -18.38911715685844683 ) ) ;
#8175 = ORIENTED_EDGE ( 'NONE', *, *, #29512, .F. ) ;
#8176 = CARTESIAN_POINT ( 'NONE',  ( 121.7590748109119687, -7.893985811506177619, -18.51759400769804742 ) ) ;
#8177 = CARTESIAN_POINT ( 'NONE',  ( 114.0246765045248196, -2.791137627527939813, -8.388885654883777576 ) ) ;
#8178 = FACE_OUTER_BOUND ( 'NONE', #39672, .T. ) ;
#8179 = DIRECTION ( 'NONE',  ( 0.000000000000000000, 0.000000000000000000, 1.000000000000000000 ) ) ;
#8180 = AXIS2_PLACEMENT_3D ( 'NONE', #6100, #33903, #30498 ) ;
#8181 = EDGE_CURVE ( 'NONE', #20803, #24054, #11263, .T. ) ;
#8182 = LINE ( 'NONE', #22532, #16758 ) ;
#8183 = CARTESIAN_POINT ( 'NONE',  ( 116.0388171295248014, 0.1403307496149613920, -13.39321520033831447 ) ) ;
#8184 = ORIENTED_EDGE ( 'NONE', *, *, #40198, .T. ) ;
#8185 = CARTESIAN_POINT ( 'NONE',  ( 120.7379948109119709, 0.4262465694468514643, -12.03445270309931736 ) ) ;
#8186 = CARTESIAN_POINT ( 'NONE',  ( 121.1325173109119788, 0.2312338769422704887, -16.08380026872395874 ) ) ;
#8187 = CARTESIAN_POINT ( 'NONE',  ( 121.4797829359119987, -4.283928203966213211, -7.183505701512925334 ) ) ;
#8188 = CARTESIAN_POINT ( 'NONE',  ( 120.3988246589382243, -8.341213398351554176, -17.25835129106724608 ) ) ;
#8189 = CARTESIAN_POINT ( 'NONE',  ( 107.5655358795247736, -8.402594152722688392, -9.854619843455216355 ) ) ;
#8190 = ORIENTED_EDGE ( 'NONE', *, *, #27230, .F. ) ;
#8191 = VECTOR ( 'NONE', #45119, 1000.000000000000227 ) ;
#8192 = CARTESIAN_POINT ( 'NONE',  ( 113.5904348109119866, -7.893985811506177619, -18.51759400769804742 ) ) ;
#8193 = CARTESIAN_POINT ( 'NONE',  ( 73.07463722459043254, -59.42495381848112856, -36.07827564460922787 ) ) ;
#8194 = CARTESIAN_POINT ( 'NONE',  ( 122.0427081442452817, -9.859900752359378018, -12.68260735090039759 ) ) ;
#8195 = CARTESIAN_POINT ( 'NONE',  ( 112.7962614775786676, -6.222761293078241884, -8.102969835052219238 ) ) ;
#8196 = CARTESIAN_POINT ( 'NONE',  ( 122.6009548109119720, -12.48189245497263755, -10.95032834292243074 ) ) ;
#8197 = DIRECTION ( 'NONE',  ( 0.000000000000000000, 0.6004852223388321697, -0.7996358532186279566 ) ) ;
#8198 = LINE ( 'NONE', #1123, #39744 ) ;
#8199 = ORIENTED_EDGE ( 'NONE', *, *, #11652, .T. ) ;
#8200 = CARTESIAN_POINT ( 'NONE',  ( 115.2748327545248657, -6.936859964151250502, -8.388885654883777576 ) ) ;
#8201 = ADVANCED_FACE ( 'NONE', ( #4857 ), #10814, .T. ) ;
#8202 = CARTESIAN_POINT ( 'NONE',  ( 122.2696148109119889, -4.089484607189486809, -7.948022111789456723 ) ) ;
#8203 = CARTESIAN_POINT ( 'NONE',  ( 137.3374356171242425, -9.397741642277191332, -15.90269339653739600 ) ) ;
#8204 = VERTEX_POINT ( 'NONE', #14455 ) ;
#8205 = CARTESIAN_POINT ( 'NONE',  ( 121.0415731642484474, -2.215723800389698184, -18.16877924232191788 ) ) ;
#8206 = B_SPLINE_CURVE_WITH_KNOTS ( 'NONE', 3,
 ( #29035, #25396, #26063, #15575, #1214, #8510, #39967, #32441, #33104, #19224 ),
 .UNSPECIFIED., .F., .F.,
 ( 4, 3, 3, 4 ),
 ( 1.226634733346699927E-18, 0.0001671877548681270013, 0.0003343755096277674864, 0.0006463528481650609656 ),
 .UNSPECIFIED. ) ;
#8207 = CARTESIAN_POINT ( 'NONE',  ( 124.7088614775786226, 0.2603800115204892296, -16.42320221600525088 ) ) ;
#8208 = AXIS2_PLACEMENT_3D ( 'NONE', #30799, #20985, #38081 ) ;
#8209 = FACE_OUTER_BOUND ( 'NONE', #6929, .T. ) ;
#8210 = CARTESIAN_POINT ( 'NONE',  ( 123.0070614775786169, -10.15424416112533912, -14.75197769757731336 ) ) ;
#8211 = ORIENTED_EDGE ( 'NONE', *, *, #26672, .F. ) ;
#8212 = CARTESIAN_POINT ( 'NONE',  ( 119.5467348109119712, -4.089484607189486809, -7.948022111789456723 ) ) ;
#8213 = DIRECTION ( 'NONE',  ( 1.000000000000000000, 0.000000000000000000, -0.000000000000000000 ) ) ;
#8214 = CARTESIAN_POINT ( 'NONE',  ( 116.5425841868944730, -2.239543233855044058, -18.13706010537467606 ) ) ;
#8215 = CARTESIAN_POINT ( 'NONE',  ( 112.0588148109119828, -9.859900752359374465, -12.68260735090038693 ) ) ;
#8216 = CARTESIAN_POINT ( 'NONE',  ( 116.1998614775786649, -10.63000616557722111, -14.87417383870573850 ) ) ;
#8217 = CARTESIAN_POINT ( 'NONE',  ( 136.5847729262639518, -5.440308620034753240, -7.712429856759469793 ) ) ;
#8218 = CARTESIAN_POINT ( 'NONE',  ( 126.1270281442452870, -10.30919188438810075, -12.61870101168855918 ) ) ;
#8219 = DIRECTION ( 'NONE',  ( 0.000000000000000000, 0.000000000000000000, 1.000000000000000000 ) ) ;
#8220 = AXIS2_PLACEMENT_3D ( 'NONE', #8548, #22449, #32915 ) ;
#8221 = FACE_OUTER_BOUND ( 'NONE', #22666, .T. ) ;
#8222 = CARTESIAN_POINT ( 'NONE',  ( 112.1722681442453222, -8.899110576539710493, -16.42337572283490132 ) ) ;
#8223 = CARTESIAN_POINT ( 'NONE',  ( 125.4463081442452932, -4.153390946401325223, -8.397313243818185668 ) ) ;
#8224 = CARTESIAN_POINT ( 'NONE',  ( 116.5987716749792895, -9.866677412677834269, -13.52174868289714027 ) ) ;
#8225 = CARTESIAN_POINT ( 'NONE',  ( 122.1561614775786353, -8.899110576539710493, -16.42337572283490132 ) ) ;
#8226 = FACE_OUTER_BOUND ( 'NONE', #39995, .T. ) ;
#8227 = CARTESIAN_POINT ( 'NONE',  ( 119.1496481442453046, -3.383040157471821630, -19.15922257007629170 ) ) ;
#8228 = EDGE_LOOP ( 'NONE', ( #11434, #22844, #16388, #18425 ) ) ;
#8229 = CARTESIAN_POINT ( 'NONE',  ( 114.5549666496844878, 0.5600166689815611054, -12.14321520033831625 ) ) ;
#8230 = CARTESIAN_POINT ( 'NONE',  ( 125.7299414775786488, -10.15424416112507799, -14.75197769757834543 ) ) ;
#8231 = CARTESIAN_POINT ( 'NONE',  ( 111.3160046295247838, -4.863998795839590272, -18.39754474579285315 ) ) ;
#8232 = CARTESIAN_POINT ( 'NONE',  ( 112.7050671295247923, 0.1403307496149613920, -13.39321520033831447 ) ) ;
#8233 = CARTESIAN_POINT ( 'NONE',  ( 126.9733055311784113, -9.947468459844838407, -11.63960890282051430 ) ) ;
#8234 = CARTESIAN_POINT ( 'NONE',  ( 115.7460481442453357, 0.9020085738987339008, -11.91225656197089222 ) ) ;
#8235 = ORIENTED_EDGE ( 'NONE', *, *, #43431, .F. ) ;
#8236 = CARTESIAN_POINT ( 'NONE',  ( 115.3489614775786407, -0.8288870151387760510, -10.36305467784173118 ) ) ;
#8237 = CARTESIAN_POINT ( 'NONE',  ( 107.4960827545248350, -2.477300249445798297, -19.15521520033831138 ) ) ;
#8238 = CARTESIAN_POINT ( 'NONE',  ( 75.95778847736481509, -3.256761025687722189, -18.64321520033831803 ) ) ;
#8239 = CARTESIAN_POINT ( 'NONE',  ( 125.8433948109119456, -1.834011780172310813, -8.268836392978581529 ) ) ;
#8240 = CARTESIAN_POINT ( 'NONE',  ( 123.1205148109119563, -7.643976991954077427, -18.09477374809248218 ) ) ;
#8241 = CARTESIAN_POINT ( 'NONE',  ( -13.08039557466221048, -4.101515749868387850, -19.20787527460400312 ) ) ;
#8242 = CARTESIAN_POINT ( 'NONE',  ( 117.1642148109119859, -9.261995988541697145, -16.69588392320189030 ) ) ;
#8243 = CARTESIAN_POINT ( 'NONE',  ( 111.8716296295247901, -4.863998795839590272, -19.15521520033831493 ) ) ;
#8244 = CARTESIAN_POINT ( 'NONE',  ( 113.0523327545247838, -6.936859964151250502, -8.388885654883777576 ) ) ;
#8245 = ORIENTED_EDGE ( 'NONE', *, *, #36969, .F. ) ;
#8246 = CARTESIAN_POINT ( 'NONE',  ( 126.2333338125949354, -7.752129280697795721, -9.302501600808184890 ) ) ;
#8247 = CARTESIAN_POINT ( 'NONE',  ( 119.2631014775786298, -9.565557343593413364, -10.61323700422348004 ) ) ;
#8248 = CARTESIAN_POINT ( 'NONE',  ( 117.3911214775786505, -1.561330072975668504, -17.79121239304076951 ) ) ;
#8249 = CARTESIAN_POINT ( 'NONE',  ( 83.84865386347668448, -25.99489077589588604, -11.39321520033831447 ) ) ;
#8250 = CARTESIAN_POINT ( 'NONE',  ( 125.0492214775786266, -3.505236298600246325, -18.68346056562440793 ) ) ;
#8251 = UNCERTAINTY_MEASURE_WITH_UNIT (LENGTH_MEASURE( 1.000000000000000082E-05 ), #25752, 'distance_accuracy_value', 'NONE');
#8252 = CARTESIAN_POINT ( 'NONE',  ( 124.8790414775786246, -8.899110576539710493, -16.42337572283490132 ) ) ;
#8253 = CARTESIAN_POINT ( 'NONE',  ( 116.2565881442453133, -0.8288870151387760510, -10.36305467784173118 ) ) ;
#8254 = VERTEX_POINT ( 'NONE', #42503 ) ;
#8255 = CARTESIAN_POINT ( 'NONE',  ( 121.0630641859119976, -0.8832429491016019485, -18.19431474523657855 ) ) ;
#8256 = CIRCLE ( 'NONE', #20634, 2.000000000000000444 ) ;
#8257 = FACE_OUTER_BOUND ( 'NONE', #39943, .T. ) ;
#8258 = CARTESIAN_POINT ( 'NONE',  ( 116.9373081442452929, -1.833838273342659253, -17.42832698103878286 ) ) ;
#8259 = ORIENTED_EDGE ( 'NONE', *, *, #14994, .F. ) ;
#8260 = CARTESIAN_POINT ( 'NONE',  ( 111.0762212410415799, 0.7607806665037644134, -12.14321520033829316 ) ) ;
#8261 = CARTESIAN_POINT ( 'NONE',  ( 115.2355081442453155, -10.30919188438810075, -12.61870101168855918 ) ) ;
#8262 = CARTESIAN_POINT ( 'NONE',  ( 107.7044421295247929, -9.868328341294093420, -13.39321520033831447 ) ) ;
#8263 = CARTESIAN_POINT ( 'NONE',  ( 112.6260814775786514, -0.8288870151387760510, -10.36305467784173118 ) ) ;
#8264 = ORIENTED_EDGE ( 'NONE', *, *, #30047, .F. ) ;
#8265 = ORIENTED_EDGE ( 'NONE', *, *, #32837, .F. ) ;
#8266 = CARTESIAN_POINT ( 'NONE',  ( 120.9649014775786355, -6.222761293078241884, -8.102969835052219238 ) ) ;
#8267 = CARTESIAN_POINT ( 'NONE',  ( 116.4834948109119779, -7.894159318335828068, -9.358103419637847864 ) ) ;
#8268 = CARTESIAN_POINT ( 'NONE',  ( 124.5884359875738170, -9.769705091392824059, -14.37932942410840198 ) ) ;
#8269 = EDGE_CURVE ( 'NONE', #18421, #43489, #24709, .T. ) ;
#8270 = CARTESIAN_POINT ( 'NONE',  ( 116.5969481442453031, -9.859900752359374465, -12.68260735090039404 ) ) ;
#8271 = VERTEX_POINT ( 'NONE', #38835 ) ;
#8272 = AXIS2_PLACEMENT_3D ( 'NONE', #26139, #42178, #14356 ) ;
#8273 = CARTESIAN_POINT ( 'NONE',  ( 70.19189222814998175, -56.12358456014947450, -35.65224734057483857 ) ) ;
#8274 = CARTESIAN_POINT ( 'NONE',  ( 61.90822566489802625, -65.63993958762723935, -44.13121205742435649 ) ) ;
#8275 = CARTESIAN_POINT ( 'NONE',  ( 109.4407702545248355, -10.62599879583958717, -15.77991374673208469 ) ) ;
#8276 = CIRCLE ( 'NONE', #33750, 4.999999999999999112 ) ;
#8277 = CARTESIAN_POINT ( 'NONE',  ( 116.0296814775786345, -8.166667518702817929, -8.995218007635861213 ) ) ;
#8279 = CARTESIAN_POINT ( 'NONE',  ( 115.1220548109119761, -1.833838273342658809, -17.42832698103878286 ) ) ;
#8278 = CARTESIAN_POINT ( 'NONE',  ( 112.1155414775786454, 0.9020085738987339008, -11.91225656197089222 ) ) ;
#8280 = CARTESIAN_POINT ( 'NONE',  ( 122.3263414775786373, -3.505236298600246325, -18.68346056562440793 ) ) ;
#8281 = LINE ( 'NONE', #39736, #12372 ) ;
#8282 = ORIENTED_EDGE ( 'NONE', *, *, #44579, .T. ) ;
#8283 = CARTESIAN_POINT ( 'NONE',  ( 120.5110881442453206, -3.505236298600246325, -18.68346056562440793 ) ) ;
#8284 = CARTESIAN_POINT ( 'NONE',  ( 125.5597614775786326, -7.894159318335828068, -9.358103419637847864 ) ) ;
#8285 = CARTESIAN_POINT ( 'NONE',  ( 115.6220983795247861, -0.7896495226426338832, -9.318865927141430916 ) ) ;
#8286 = AXIS2_PLACEMENT_3D ( 'NONE', #19217, #28587, #21739 ) ;
#8287 = CARTESIAN_POINT ( 'NONE',  ( 67.30914723170953096, -52.10122428197148992, -34.93782514184813692 ) ) ;
#8288 = CARTESIAN_POINT ( 'NONE',  ( 114.3719421295247827, 0.8980012041604618078, -13.39321520033831447 ) ) ;
#8289 = CARTESIAN_POINT ( 'NONE',  ( 117.6180281442453150, -0.4660016031367893996, -10.09054647747474043 ) ) ;
#8290 = ORIENTED_EDGE ( 'NONE', *, *, #15239, .F. ) ;
#8291 = CARTESIAN_POINT ( 'NONE',  ( 117.5613014775786525, 0.9020085738987339008, -11.91225656197089222 ) ) ;
#8292 = DIRECTION ( 'NONE',  ( 1.000000000000000000, 0.000000000000000000, 0.000000000000000000 ) ) ;
#8293 = CARTESIAN_POINT ( 'NONE',  ( 105.4819421295248247, 0.8980012041604618078, -13.39321520033831447 ) ) ;
#8294 = CARTESIAN_POINT ( 'NONE',  ( 115.4056881442453459, -7.893985811506177619, -18.51759400769804742 ) ) ;
#8295 = CARTESIAN_POINT ( 'NONE',  ( 118.7525614775786380, -8.166667518702819706, -8.995218007635861213 ) ) ;
#8296 = CARTESIAN_POINT ( 'NONE',  ( -11.17889843615491685, -5.940389178047622565, -19.39321520033831447 ) ) ;
#8297 = DIRECTION ( 'NONE',  ( -0.1352586133457950590, -0.9908103287288504424, 0.000000000000000000 ) ) ;
#8298 = CARTESIAN_POINT ( 'NONE',  ( 104.9957702545248566, 0.1403307496149616695, -11.32035403202665336 ) ) ;
#8299 = EDGE_CURVE ( 'NONE', #31941, #2957, #34875, .T. ) ;
#8300 = ORIENTED_EDGE ( 'NONE', *, *, #39630, .F. ) ;
#8301 = DIRECTION ( 'NONE',  ( -0.1352586133457950590, -0.9908103287288504424, 0.000000000000000000 ) ) ;
#8302 = CARTESIAN_POINT ( 'NONE',  ( 109.2294421295247417, -9.077645375966321595, -9.469096113667132997 ) ) ;
#8303 = CARTESIAN_POINT ( 'NONE',  ( 118.6391081442452986, -5.574606645277164318, -18.38911715685844683 ) ) ;
#8304 = CARTESIAN_POINT ( 'NONE',  ( 111.0381921295247878, -9.868328341294093420, -13.39321520033831447 ) ) ;
#8305 = CARTESIAN_POINT ( 'NONE',  ( 105.5513952545248060, 0.8980012041604421569, -11.00651665394454071 ) ) ;
#8306 = CARTESIAN_POINT ( 'NONE',  ( 115.8027748109119841, -8.899110576539710493, -16.42337572283490132 ) ) ;
#8307 = CARTESIAN_POINT ( 'NONE',  ( 82.42995973409283295, -31.76308506831635725, -22.83422094025958415 ) ) ;
#8308 = EDGE_CURVE ( 'NONE', #21853, #25264, #13206, .T. ) ;
#8309 = CARTESIAN_POINT ( 'NONE',  ( 114.1009748109119784, -5.574606645277164318, -18.38911715685844683 ) ) ;
#8310 = CARTESIAN_POINT ( 'NONE',  ( 118.7525614775786380, -8.166667518702819706, -8.995218007635861213 ) ) ;
#8311 = EDGE_LOOP ( 'NONE', ( #33161, #14690, #16253, #17208 ) ) ;
#8312 = ADVANCED_FACE ( 'NONE', ( #991 ), #31355, .T. ) ;
#8313 = CARTESIAN_POINT ( 'NONE',  ( 118.5823814775786360, -7.643976991954077427, -18.09477374809248928 ) ) ;
#8314 = CARTESIAN_POINT ( 'NONE',  ( 115.9162281442453235, -4.089484607189486809, -7.948022111789456723 ) ) ;
#8315 = CARTESIAN_POINT ( 'NONE',  ( 121.1350814775786233, 0.5811942927096110934, -14.16772938898807510 ) ) ;
#8316 = CARTESIAN_POINT ( 'NONE',  ( 119.0361948109119652, -2.084020599724406786, -8.691656652584148546 ) ) ;
#8317 = ORIENTED_EDGE ( 'NONE', *, *, #11114, .T. ) ;
#8318 = CARTESIAN_POINT ( 'NONE',  ( 125.0492214775786266, -3.505236298600246325, -18.68346056562440793 ) ) ;
#8319 = CARTESIAN_POINT ( 'NONE',  ( 121.7023481442452777, -9.261995988541697145, -16.69588392320189030 ) ) ;
#8320 = CARTESIAN_POINT ( 'NONE',  ( 125.0480389746924885, -6.045022021006678514, -5.955407747331282309 ) ) ;
#8321 = EDGE_CURVE ( 'NONE', #18562, #25347, #40410, .T. ) ;
#8322 =( BOUNDED_CURVE ( )  B_SPLINE_CURVE ( 2, ( #3845, #20968, #7270, #17113, #17765, #35292, #31661, #4064, #17989, #31888, #29378, #35978, #40092, #42618, #11380, #35522, #8852 ),
 .UNSPECIFIED., .F., .T. ) 
 B_SPLINE_CURVE_WITH_KNOTS ( ( 3, 2, 2, 2, 2, 2, 2, 2, 3 ),
 ( 0.5102707595410509445, 0.5312500000000000000, 0.5625000000000000000, 0.5937500000000000000, 0.6250000000000000000, 0.6562500000000000000, 0.6875000000000000000, 0.7187500000000000000, 0.7397292404589489445 ),
 .UNSPECIFIED. ) 
 CURVE ( )  GEOMETRIC_REPRESENTATION_ITEM ( )  RATIONAL_B_SPLINE_CURVE ( ( 0.9664089390052280626, 0.9488976130786129781, 1.000000000000000000, 0.9238795325112869605, 1.000000000000000000, 0.9238795325112869605, 1.000000000000000000, 0.9238795325112869605, 1.000000000000000000, 0.9238795325112869605, 1.000000000000000000, 0.9238795325112869605, 1.000000000000000000, 0.9238795325112869605, 1.000000000000000000, 0.9488976130786129781, 0.9664089390052290618 ) ) 
 REPRESENTATION_ITEM ( '' )  );
#8323 = EDGE_CURVE ( 'NONE', #31933, #18860, #24171, .T. ) ;
#8324 = EDGE_CURVE ( 'NONE', #3191, #5950, #2733, .T. ) ;
#8325 = CARTESIAN_POINT ( 'NONE',  ( 121.9470836909669913, -25.99489077589524300, -13.39321520033831447 ) ) ;
#8326 = CARTESIAN_POINT ( 'NONE',  ( 118.9279538206745315, -2.348512537728035365, -17.99195118506215252 ) ) ;
#8327 = B_SPLINE_CURVE_WITH_KNOTS ( 'NONE', 3,
 ( #34774, #41438, #17470, #6988, #23885, #30709, #24755, #28190 ),
 .UNSPECIFIED., .F., .F.,
 ( 4, 2, 2, 4 ),
 ( 0.000000000000000000, 0.2500000000000000000, 0.5000000000000000000, 1.000000000000000000 ),
 .UNSPECIFIED. ) ;
#8328 = CARTESIAN_POINT ( 'NONE',  ( 114.1635827545248389, -6.936859964151250502, -8.388885654883777576 ) ) ;
#8329 = FACE_OUTER_BOUND ( 'NONE', #35749, .T. ) ;
#8330 = CARTESIAN_POINT ( 'NONE',  ( 115.3489614775786407, -0.8288870151387760510, -10.36305467784173118 ) ) ;
#8331 = CARTESIAN_POINT ( 'NONE',  ( 111.7184548109119788, -0.8288870151387760510, -10.36305467784173118 ) ) ;
#8332 = CARTESIAN_POINT ( 'NONE',  ( 64.83175385985305184, -13.24295385337449460, -15.23335304249422428 ) ) ;
#8333 = CARTESIAN_POINT ( 'NONE',  ( 117.4478481442452846, -9.565557343593393824, -10.61323700422345340 ) ) ;
#8334 = CARTESIAN_POINT ( 'NONE',  ( 112.5661608795247872, -1.325403438956436419, -16.93181055722141792 ) ) ;
#8335 = CARTESIAN_POINT ( 'NONE',  ( 115.5566632127138575, -2.191907684172563986, -18.20049396185734025 ) ) ;
#8336 = DIRECTION ( 'NONE',  ( -0.8636456077245080465, 0.5040994586965603652, 0.000000000000000000 ) ) ;
#8337 = CARTESIAN_POINT ( 'NONE',  ( 124.1014853070358868, -1.196538596002817867, -17.02799684832028504 ) ) ;
#8339 = CARTESIAN_POINT ( 'NONE',  ( 118.8660148109119774, -10.30919188438810075, -12.61870101168855918 ) ) ;
#8338 = CARTESIAN_POINT ( 'NONE',  ( 64.04456645099679690, -15.08556008563613204, -10.41505815062060236 ) ) ;
#8340 = CARTESIAN_POINT ( 'NONE',  ( 124.5954081442453116, -6.222761293078241884, -8.102969835052219238 ) ) ;
#8341 = VERTEX_POINT ( 'NONE', #30552 ) ;
#8342 = CARTESIAN_POINT ( 'NONE',  ( 137.3374356171252373, -7.373476992039340594, -8.859472353902042130 ) ) ;
#8343 = CARTESIAN_POINT ( 'NONE',  ( 124.8790414775786246, -0.4660016031367893996, -10.09054647747474043 ) ) ;
#8344 = CARTESIAN_POINT ( 'NONE',  ( 109.1629577545248395, -2.791137627527939813, -18.39754474579286025 ) ) ;
#8345 = CARTESIAN_POINT ( 'NONE',  ( 118.8660148109119774, 0.1319031606808879209, -14.10382304977623669 ) ) ;
#8346 = CARTESIAN_POINT ( 'NONE',  ( 122.7801548109119665, -6.222761293078241884, -8.102969835052219238 ) ) ;
#8347 = CARTESIAN_POINT ( 'NONE',  ( 116.9373081442452929, -1.833838273342659253, -17.42832698103878286 ) ) ;
#8348 = CARTESIAN_POINT ( 'NONE',  ( 111.7184548109119788, -8.862178061932382889, -16.39564131203247399 ) ) ;
#8349 = CARTESIAN_POINT ( 'NONE',  ( 108.0517077545248696, -7.250697342233347165, -7.631215200338321125 ) ) ;
#8350 = CARTESIAN_POINT ( 'NONE',  ( 124.5386814775786206, -4.153390946401325223, -8.397313243818185668 ) ) ;
#8351 = CARTESIAN_POINT ( 'NONE',  ( 123.8579614775786126, -9.859900752359378018, -12.68260735090039759 ) ) ;
#8352 = DIRECTION ( 'NONE',  ( -0.6836572958096082120, 0.7298031939408691215, 0.000000000000000000 ) ) ;
#8353 = CARTESIAN_POINT ( 'NONE',  ( 73.07463722459043254, -55.71104259080762233, -34.59272409957256400 ) ) ;
#8354 = CARTESIAN_POINT ( 'NONE',  ( 121.0630641859119976, -8.321307733199551748, -9.223433127585318303 ) ) ;
#8355 = CARTESIAN_POINT ( 'NONE',  ( 106.4542858795248179, -8.402594152722688392, -9.854619843455216355 ) ) ;
#8356 = CARTESIAN_POINT ( 'NONE',  ( 84.10862215250544693, -25.99489077589524300, -13.39321520033831625 ) ) ;
#8357 = CARTESIAN_POINT ( 'NONE',  ( 83.36817807618649567, -33.10911252753713541, -22.72403028787429591 ) ) ;
#8358 = CARTESIAN_POINT ( 'NONE',  ( 121.5888948109119809, -10.30919188438810075, -12.61870101168855918 ) ) ;
#8359 = CARTESIAN_POINT ( 'NONE',  ( 117.9016614775786280, -9.988377603198976828, -10.36322818467138340 ) ) ;
#8360 = CARTESIAN_POINT ( 'NONE',  ( 60.45894907855897316, -4.846173528048923096, -9.393215200338314474 ) ) ;
#8361 = CARTESIAN_POINT ( 'NONE',  ( 112.2857214775786474, -4.089484607189486809, -7.948022111789456723 ) ) ;
#8362 = CARTESIAN_POINT ( 'NONE',  ( 67.84197459855160162, -61.08251850740028033, -38.36497664958400122 ) ) ;
#8363 = ORIENTED_EDGE ( 'NONE', *, *, #16395, .F. ) ;
#8364 = CARTESIAN_POINT ( 'NONE',  ( 112.4711464071292824, 0.2518737723193609224, -14.64321520033832691 ) ) ;
#8365 = EDGE_CURVE ( 'NONE', #26397, #31784, #5924, .T. ) ;
#8366 = CARTESIAN_POINT ( 'NONE',  ( 117.5613014775786525, 0.9020085738987339008, -11.91225656197089222 ) ) ;
#8367 = CARTESIAN_POINT ( 'NONE',  ( 124.7655881442452852, -9.859900752359378018, -12.68260735090039759 ) ) ;
#8368 = PRODUCT_CONTEXT ( 'NONE', #6729, 'mechanical' ) ;
#8369 = CARTESIAN_POINT ( 'NONE',  ( 112.6260814775786514, -0.8288870151387760510, -10.36305467784173118 ) ) ;
#8370 = CARTESIAN_POINT ( 'NONE',  ( 124.9924948109119924, -4.089484607189486809, -7.948022111789456723 ) ) ;
#8371 = CIRCLE ( 'NONE', #42611, 2.999999999999999556 ) ;
#8372 = CARTESIAN_POINT ( 'NONE',  ( 111.6632702545248605, -10.62599879583958717, -15.77991374673208469 ) ) ;
#8373 = CARTESIAN_POINT ( 'NONE',  ( 118.7525614775786380, -1.833838273342659253, -17.42832698103878286 ) ) ;
#8374 = FACE_OUTER_BOUND ( 'NONE', #9618, .T. ) ;
#8375 = CARTESIAN_POINT ( 'NONE',  ( 70.19189222814998175, -52.61716011954800365, -34.24968978710501943 ) ) ;
#8376 = EDGE_LOOP ( 'NONE', ( #43299, #29528, #12858, #7272, #30359, #13405 ) ) ;
#8377 = EDGE_CURVE ( 'NONE', #7733, #39054, #44473, .T. ) ;
#8378 = CARTESIAN_POINT ( 'NONE',  ( 123.3550173109119612, 0.2312338769422704887, -16.08380026872395874 ) ) ;
#8379 = CARTESIAN_POINT ( 'NONE',  ( 119.1496481442453046, -3.383040157471821630, -19.15922257007629170 ) ) ;
#8380 = ORIENTED_EDGE ( 'NONE', *, *, #12193, .F. ) ;
#8381 = CARTESIAN_POINT ( 'NONE',  ( 125.6164881442453094, -9.565557343593413364, -10.61323700422348004 ) ) ;
#8382 = DIRECTION ( 'NONE',  ( 0.1736481776669305255, 0.9848077530122081313, 0.000000000000000000 ) ) ;
#8383 = ADVANCED_FACE ( 'NONE', ( #23503 ), #26089, .T. ) ;
#8384 = CARTESIAN_POINT ( 'NONE',  ( 115.2090389883689880, 0.3193521225029610777, -12.14321520033831625 ) ) ;
#8385 = CARTESIAN_POINT ( 'NONE',  ( 118.1852948109119836, -4.153390946401325223, -8.397313243818185668 ) ) ;
#8386 = CYLINDRICAL_SURFACE ( 'NONE', #15683, 3.000000000000001776 ) ;
#8387 = EDGE_CURVE ( 'NONE', #23245, #19524, #12264, .T. ) ;
#8388 = CARTESIAN_POINT ( 'NONE',  ( 123.8035975202278109, -2.239543233855044946, -18.13706010537467606 ) ) ;
#8389 = CARTESIAN_POINT ( 'NONE',  ( 123.5743281442453139, -2.084020599724406786, -8.691656652584148546 ) ) ;
#8390 = CARTESIAN_POINT ( 'NONE',  ( 121.4187148109119789, -6.344957434206645708, -7.627207830600334582 ) ) ;
#8391 = FACE_OUTER_BOUND ( 'NONE', #2111, .T. ) ;
#8392 = CIRCLE ( 'NONE', #33866, 1.999999999999998890 ) ;
#8393 = CARTESIAN_POINT ( 'NONE',  ( 89.78938736644981589, -25.99489077589524300, -13.39321520033831625 ) ) ;
#8394 = CARTESIAN_POINT ( 'NONE',  ( 117.8449348109119938, -1.833838273342659253, -17.42832698103878286 ) ) ;
#8395 = CARTESIAN_POINT ( 'NONE',  ( 123.0637881442452937, -8.899110576539710493, -16.42337572283490132 ) ) ;
#8396 = CARTESIAN_POINT ( 'NONE',  ( 113.4202548109119846, -10.30919188438810075, -12.61870101168855918 ) ) ;
#8397 = CARTESIAN_POINT ( 'NONE',  ( 121.2485348109119769, -0.4660016031367893996, -10.09054647747474043 ) ) ;
#8398 = CARTESIAN_POINT ( 'NONE',  ( 115.5191414775786569, -3.383040157471821630, -19.15922257007629170 ) ) ;
#8399 = DIRECTION ( 'NONE',  ( 0.000000000000000000, -1.000000000000000000, 0.000000000000000000 ) ) ;
#8400 = AXIS2_PLACEMENT_3D ( 'NONE', #31521, #28119, #42026 ) ;
#8401 = CARTESIAN_POINT ( 'NONE',  ( 125.3328548109119964, -0.8288870151387760510, -10.36305467784173118 ) ) ;
#8402 = ORIENTED_EDGE ( 'NONE', *, *, #11933, .F. ) ;
#8403 = CARTESIAN_POINT ( 'NONE',  ( 119.8303681442453126, -10.63000616557722466, -14.87417383870573495 ) ) ;
#8404 = CARTESIAN_POINT ( 'NONE',  ( 113.5385046295247804, -4.863998795839590272, -7.631215200338315796 ) ) ;
#8405 = CARTESIAN_POINT ( 'NONE',  ( 113.3995983795247895, -8.402594152722688392, -16.93181055722141792 ) ) ;
#8406 = DIRECTION ( 'NONE',  ( 0.000000000000000000, -0.3818493186865927203, 0.9242245927363029745 ) ) ;
#8407 = FACE_OUTER_BOUND ( 'NONE', #24964, .T. ) ;
#8408 = CARTESIAN_POINT ( 'NONE',  ( 84.39081516114413262, -30.32262605124143562, -12.39321520033834645 ) ) ;
#8409 = CARTESIAN_POINT ( 'NONE',  ( 126.1270281442452870, -10.30919188438810075, -12.61870101168855918 ) ) ;
#8410 = VERTEX_POINT ( 'NONE', #37388 ) ;
#8411 = CARTESIAN_POINT ( 'NONE',  ( 120.4543614775786295, -5.574606645277164318, -18.38911715685844683 ) ) ;
#8412 = CARTESIAN_POINT ( 'NONE',  ( 120.9241579359119925, -5.444069387712269226, -19.60292469916370450 ) ) ;
#8413 = CARTESIAN_POINT ( 'NONE',  ( 123.6328298109119714, -2.173413727453600508, -8.297982527556802879 ) ) ;
#8414 = CARTESIAN_POINT ( 'NONE',  ( 67.84197459855160162, -52.72621824513493038, -35.02248567325151640 ) ) ;
#8415 = CARTESIAN_POINT ( 'NONE',  ( 105.8292077545248446, -2.791137627527939813, -18.39754474579286025 ) ) ;
#8416 = ORIENTED_EDGE ( 'NONE', *, *, #40344, .F. ) ;
#8417 = CARTESIAN_POINT ( 'NONE',  ( 113.4769814775786330, -10.63000616557722466, -14.87417383870573495 ) ) ;
#8418 = CARTESIAN_POINT ( 'NONE',  ( 77.12856116249137983, -44.30583187727815186, -6.893215200338315363 ) ) ;
#8419 = CARTESIAN_POINT ( 'NONE',  ( 119.9438214775786378, -2.084020599724406786, -8.691656652584148546 ) ) ;
#8420 = CARTESIAN_POINT ( 'NONE',  ( 67.30914723170953096, -54.16566668288025710, -35.76359490593331003 ) ) ;
#8421 = CARTESIAN_POINT ( 'NONE',  ( 73.01241679510815175, -70.92052552613920113, -40.69577108532303811 ) ) ;
#8422 = CARTESIAN_POINT ( 'NONE',  ( 115.0286927483929134, -2.423081321603721694, -17.89265170041262465 ) ) ;
#8423 =( NAMED_UNIT ( * ) SI_UNIT ( $, .STERADIAN. ) SOLID_ANGLE_UNIT ( ) );
#8424 = ORIENTED_EDGE ( 'NONE', *, *, #34011, .F. ) ;
#8425 = EDGE_CURVE ( 'NONE', #31466, #28016, #26973, .T. ) ;
#8426 = AXIS2_PLACEMENT_3D ( 'NONE', #24813, #21391, #28693 ) ;
#8427 = CARTESIAN_POINT ( 'NONE',  ( 115.4831921295247952, -9.868328341294093420, -13.39321520033831447 ) ) ;
#8428 = CARTESIAN_POINT ( 'NONE',  ( 119.1496481442453046, -3.383040157471821630, -19.15922257007629170 ) ) ;
#8429 = CARTESIAN_POINT ( 'NONE',  ( 137.0105207745601774, -8.461374316958192310, -17.49868728018336483 ) ) ;
#8430 = ORIENTED_EDGE ( 'NONE', *, *, #2612, .F. ) ;
#8431 = CARTESIAN_POINT ( 'NONE',  ( 112.5693548109119888, -10.63000616557722466, -14.87417383870573495 ) ) ;
#8432 = CARTESIAN_POINT ( 'NONE',  ( 111.7751814775786556, -2.084020599724406786, -8.691656652584148546 ) ) ;
#8433 = AXIS2_PLACEMENT_3D ( 'NONE', #25208, #34980, #4665 ) ;
#8434 = CARTESIAN_POINT ( 'NONE',  ( 75.95778847736481509, -3.256761025687722189, -7.993215200338315007 ) ) ;
#8435 = CARTESIAN_POINT ( 'NONE',  ( 123.0637881442452937, -8.899110576539710493, -16.42337572283490132 ) ) ;
#8436 = ORIENTED_EDGE ( 'NONE', *, *, #21102, .F. ) ;
#8437 = CARTESIAN_POINT ( 'NONE',  ( 117.4478481442453131, 0.2603800115204892296, -16.42320221600525088 ) ) ;
#8438 = EDGE_CURVE ( 'NONE', #16407, #24250, #23730, .T. ) ;
#8439 = AXIS2_PLACEMENT_3D ( 'NONE', #21429, #18235, #31681 ) ;
#8440 = DIRECTION ( 'NONE',  ( 0.000000000000000000, 0.9284778069183720062, 0.3713878862591650232 ) ) ;
#8441 = CARTESIAN_POINT ( 'NONE',  ( 116.8439460817262585, -2.423081321603731020, -17.89265170041263175 ) ) ;
#8442 = FACE_OUTER_BOUND ( 'NONE', #42845, .T. ) ;
#8443 = CARTESIAN_POINT ( 'NONE',  ( 84.38170309240724976, -27.84333996136784961, -14.15691383771150136 ) ) ;
#8444 = CARTESIAN_POINT ( 'NONE',  ( 112.8529881442453160, -7.894159318335828068, -9.358103419637847864 ) ) ;
#8445 = CARTESIAN_POINT ( 'NONE',  ( 128.2184548109119930, 0.7167481258041193959, -11.18974888642105014 ) ) ;
#8446 = CARTESIAN_POINT ( 'NONE',  ( 3.060777270043529619, -5.064559853354640317, -7.393215200338315363 ) ) ;
#8447 = CONICAL_SURFACE ( 'NONE', #14271, 3077.683537175320453, 1.256637061435923686 ) ;
#8448 = CARTESIAN_POINT ( 'NONE',  ( 113.4202548109119846, 0.1319031606808879209, -14.10382304977623669 ) ) ;
#8449 = CARTESIAN_POINT ( 'NONE',  ( 112.5126281442453120, -10.30919188438810075, -12.61870101168855918 ) ) ;
#8450 = CARTESIAN_POINT ( 'NONE',  ( 120.9936110609119737, -6.340755971794695078, -8.611740276972781771 ) ) ;
#8451 = CARTESIAN_POINT ( 'NONE',  ( 124.7088614775786226, -9.565557343593413364, -10.61323700422348004 ) ) ;
#8452 = DIRECTION ( 'NONE',  ( -0.8636456077245089347, 0.5040994586965589219, 0.000000000000000000 ) ) ;
#8453 = CARTESIAN_POINT ( 'NONE',  ( 120.7947214775786193, -9.261995988541697145, -16.69588392320189030 ) ) ;
#8454 = EDGE_LOOP ( 'NONE', ( #23604, #18020, #38830, #17425 ) ) ;
#8455 = CARTESIAN_POINT ( 'NONE',  ( 127.4620922276976955, -8.463570135024619745, -17.71167606724072741 ) ) ;
#8456 = CARTESIAN_POINT ( 'NONE',  ( 67.84197459855160162, -56.44012947280842241, -36.50803721828817316 ) ) ;
#8457 = CARTESIAN_POINT ( 'NONE',  ( 108.5378796295247810, -4.863998795839590272, -8.388885654883775800 ) ) ;
#8458 = CARTESIAN_POINT ( 'NONE',  ( 110.2047546295247855, -4.863998795839590272, -18.39754474579285315 ) ) ;
#8459 = ADVANCED_FACE ( 'NONE', ( #34407 ), #40684, .T. ) ;
#8460 = CARTESIAN_POINT ( 'NONE',  ( 126.2471382750683659, -9.795756905406328485, -12.48647926791751139 ) ) ;
#8461 = CARTESIAN_POINT ( 'NONE',  ( 113.8740681442453138, 0.5811942927096154232, -14.16772938898807155 ) ) ;
#8462 = ORIENTED_EDGE ( 'NONE', *, *, #41925, .T. ) ;
#8463 = CARTESIAN_POINT ( 'NONE',  ( 106.8710046295248759, -4.863998795839590272, -7.631215200338315796 ) ) ;
#8464 = CARTESIAN_POINT ( 'NONE',  ( 70.19189222814998175, -55.40259354030312267, -35.36385344588251911 ) ) ;
#8465 = DIRECTION ( 'NONE',  ( 0.000000000000000000, -0.9242245927363028635, -0.3818493186865930533 ) ) ;
#8466 = CARTESIAN_POINT ( 'NONE',  ( 77.22947525540432423, -44.03086066871760096, -6.893215200338315363 ) ) ;
#8467 = CARTESIAN_POINT ( 'NONE',  ( 112.4559014775786494, -9.988377603198976828, -10.36322818467138340 ) ) ;
#8468 = CARTESIAN_POINT ( 'NONE',  ( 119.3198281442452924, 0.5811942927096110934, -14.16772938898807510 ) ) ;
#8469 = CARTESIAN_POINT ( 'NONE',  ( 109.0240515045248202, -2.477300249445798297, -7.631215200338321125 ) ) ;
#8470 = CARTESIAN_POINT ( 'NONE',  ( 110.5520202545248054, 0.1403307496149616695, -11.32035403202665336 ) ) ;
#8471 = ORIENTED_EDGE ( 'NONE', *, *, #35047, .T. ) ;
#8472 = DIRECTION ( 'NONE',  ( -0.4225728684367210941, 0.9063289528979869836, 0.000000000000000000 ) ) ;
#8473 = CARTESIAN_POINT ( 'NONE',  ( 117.9016614775786280, -0.1624402480850797581, -16.17319339645315424 ) ) ;
#8474 = CARTESIAN_POINT ( 'NONE',  ( 115.2355081442453155, -10.30919188438810075, -12.61870101168855918 ) ) ;
#8475 = CARTESIAN_POINT ( 'NONE',  ( 82.38065881859543538, -29.99489077589589314, -15.39321520033831447 ) ) ;
#8476 = CARTESIAN_POINT ( 'NONE',  ( 118.2420214775786462, -6.222761293078222344, -8.102969835052219238 ) ) ;
#8477 = CARTESIAN_POINT ( 'NONE',  ( 123.3474214775786209, -0.1624402480850797581, -16.17319339645315424 ) ) ;
#8478 = CARTESIAN_POINT ( 'NONE',  ( 115.5191414775786569, -6.222761293078241884, -8.102969835052219238 ) ) ;
#8479 = VERTEX_POINT ( 'NONE', #38721 ) ;
#8480 = CARTESIAN_POINT ( 'NONE',  ( 122.1743141859119817, -8.321307733199551748, -9.223433127585318303 ) ) ;
#8481 = CIRCLE ( 'NONE', #28856, 2.000000000000000444 ) ;
#8482 = DIRECTION ( 'NONE',  ( -0.000000000000000000, -0.9284778069183721172, -0.3713878862591650232 ) ) ;
#8483 = CARTESIAN_POINT ( 'NONE',  ( 116.9940348109119839, -0.1624402480850797581, -16.17319339645315424 ) ) ;
#8484 = ORIENTED_EDGE ( 'NONE', *, *, #34740, .F. ) ;
#8485 = CARTESIAN_POINT ( 'NONE',  ( 128.2184548109119930, -4.863998795839242995, -13.39321520033831447 ) ) ;
#8486 = CARTESIAN_POINT ( 'NONE',  ( 114.4413348109119823, -9.261995988541697145, -16.69588392320189030 ) ) ;
#8487 = CARTESIAN_POINT ( 'NONE',  ( 106.1764733795248219, -1.325403438956436419, -9.854619843455211026 ) ) ;
#8488 = CARTESIAN_POINT ( 'NONE',  ( 125.6732148109119862, -9.859900752359378018, -12.68260735090039759 ) ) ;
#8489 = AXIS2_PLACEMENT_3D ( 'NONE', #20289, #3402, #17320 ) ;
#8490 = VERTEX_POINT ( 'NONE', #35521 ) ;
#8491 = ORIENTED_EDGE ( 'NONE', *, *, #44553, .T. ) ;
#8492 = CARTESIAN_POINT ( 'NONE',  ( 120.7379948109119709, 0.4262465694468514643, -12.03445270309931736 ) ) ;
#8493 = EDGE_CURVE ( 'NONE', #18952, #20112, #18450, .T. ) ;
#8494 = CARTESIAN_POINT ( 'NONE',  ( 117.1642148109119859, -0.8288870151387760510, -10.36305467784173118 ) ) ;
#8495 = CARTESIAN_POINT ( 'NONE',  ( 77.77634386988368931, 3.254514819260763581, -4.893215200338314474 ) ) ;
#8496 = CIRCLE ( 'NONE', #28172, 2.000000000000000444 ) ;
#8497 = VERTEX_POINT ( 'NONE', #28486 ) ;
#8498 = CARTESIAN_POINT ( 'NONE',  ( 83.83554121260367253, -26.75858941326842810, -11.54476601486570964 ) ) ;
#8499 = CARTESIAN_POINT ( 'NONE',  ( 62.25607609626064942, -65.18564391136567338, -45.10442085122217293 ) ) ;
#8500 = CARTESIAN_POINT ( 'NONE',  ( 112.0105358795247810, -0.7896495226426338832, -17.46756447353520159 ) ) ;
#8501 = CARTESIAN_POINT ( 'NONE',  ( 115.3489614775786407, -9.261995988541697145, -16.69588392320189030 ) ) ;
#8503 = CARTESIAN_POINT ( 'NONE',  ( 114.3278814775786429, 0.1319031606808879209, -14.10382304977623669 ) ) ;
#8502 = CARTESIAN_POINT ( 'NONE',  ( 115.0086014775786509, -4.089484607189486809, -7.948022111789456723 ) ) ;
#8504 = CARTESIAN_POINT ( 'NONE',  ( 120.0572748109119772, -6.222761293078241884, -8.102969835052219238 ) ) ;
#8505 = CARTESIAN_POINT ( 'NONE',  ( 112.3808888976800233, -1.244021962887382315, -16.96476564598603787 ) ) ;
#8506 = ORIENTED_EDGE ( 'NONE', *, *, #7730, .F. ) ;
#8507 = CARTESIAN_POINT ( 'NONE',  ( 120.0005481442453146, -4.153390946401325223, -8.397313243818185668 ) ) ;
#8508 = CARTESIAN_POINT ( 'NONE',  ( 124.7655881442452852, -9.859900752359378018, -12.68260735090039759 ) ) ;
#8509 = CARTESIAN_POINT ( 'NONE',  ( 112.1494421295248003, 0.8980012041604618078, -13.39321520033831447 ) ) ;
#8510 = CARTESIAN_POINT ( 'NONE',  ( 114.0390358011494385, -1.149058757900090377, -17.09122335155388939 ) ) ;
#8511 = CARTESIAN_POINT ( 'NONE',  ( 111.1076452545248259, 0.8980012041604421569, -11.00651665394454071 ) ) ;
#8512 = CARTESIAN_POINT ( 'NONE',  ( 119.7736414775786358, -10.30919188438810075, -12.61870101168855918 ) ) ;
#8513 = B_SPLINE_CURVE_WITH_KNOTS ( 'NONE', 3,
 ( #24698, #38370, #530, #17862, #38586, #14217, #31535, #4394, #35393, #42489 ),
 .UNSPECIFIED., .F., .F.,
 ( 4, 3, 3, 4 ),
 ( 8.673617379884039324E-19, 0.0001671877548681294950, 0.0003343755096277725280, 0.0006463528481650619413 ),
 .UNSPECIFIED. ) ;
#8514 = ORIENTED_EDGE ( 'NONE', *, *, #8613, .T. ) ;
#8515 = CARTESIAN_POINT ( 'NONE',  ( 122.2128881442453263, -1.834011780172310813, -8.268836392978581529 ) ) ;
#8516 = DIRECTION ( 'NONE',  ( -0.000000000000000000, -0.9284778069183718952, -0.3713878862591649677 ) ) ;
#8517 = CARTESIAN_POINT ( 'NONE',  ( 108.9545983795247821, -0.7896495226426338832, -9.318865927141430916 ) ) ;
#8518 = CARTESIAN_POINT ( 'NONE',  ( 117.8449348109119938, -8.166667518702817929, -8.995218007635861213 ) ) ;
#8519 = B_SPLINE_CURVE_WITH_KNOTS ( 'NONE', 3,
 ( #28626, #38634, #17460, #7408, #10849, #28850, #31358, #42535, #3545, #11295, #3986, #131, #14487, #42761, #4216, #28398, #14043, #10628, #18362, #38419, #34976, #18132, #25205, #577, #24974, #42310, #11525, #25430, #3763, #14265, #41868, #31806, #11070, #35439, #39101, #28181, #24747, #7872, #21328, #24532, #35214, #21552, #7190, #21780, #17909, #4444 ),
 .UNSPECIFIED., .F., .F.,
 ( 4, 2, 2, 2, 2, 2, 2, 2, 2, 2, 2, 2, 2, 2, 2, 2, 2, 2, 2, 2, 2, 2, 4 ),
 ( 0.000000000000000000, 0.06249999999998950839, 0.09374999999999088229, 0.1093749999999976547, 0.1250000000000044409, 0.1875000000000314748, 0.2187500000000399958, 0.2500000000000485167, 0.3750000000000693889, 0.4375000000000795475, 0.5000000000000897060, 0.5625000000000998090, 0.5937500000001049161, 0.6093750000001075806, 0.6250000000001101341, 0.6875000000001189049, 0.7187500000001230127, 0.7343750000001187939, 0.7500000000001144640, 0.8125000000000971445, 0.8437500000000810463, 0.8750000000000649480, 1.000000000000000000 ),
 .UNSPECIFIED. ) ;
#8520 = CARTESIAN_POINT ( 'NONE',  ( 119.0929214775786278, -5.638512984488999180, -18.83840828888717311 ) ) ;
#8521 = CARTESIAN_POINT ( 'NONE',  ( 126.3975136127465362, -9.949554030138139993, -13.18299365370083898 ) ) ;
#8522 = CARTESIAN_POINT ( 'NONE',  ( 65.19189222814998175, -41.76310523276723785, -24.39321520033831447 ) ) ;
#8523 = CIRCLE ( 'NONE', #33239, 1.200000000000000178 ) ;
#8524 = ORIENTED_EDGE ( 'NONE', *, *, #42676, .T. ) ;
#8525 = DIRECTION ( 'NONE',  ( 1.000000000000000000, 0.000000000000000000, 0.000000000000000000 ) ) ;
#8526 = CARTESIAN_POINT ( 'NONE',  ( 109.2294415708224591, -10.34084703323438958, -14.19095601892115255 ) ) ;
#8527 = CARTESIAN_POINT ( 'NONE',  ( 119.6034614775786196, -3.505236298600246325, -18.68346056562440793 ) ) ;
#8528 = CARTESIAN_POINT ( 'NONE',  ( 112.9134265045247645, -2.791137627527939813, -8.388885654883777576 ) ) ;
#8529 = CARTESIAN_POINT ( 'NONE',  ( 106.5237390045248418, 0.8980012041604421569, -15.77991374673208469 ) ) ;
#8530 = CARTESIAN_POINT ( 'NONE',  ( 113.2500748109119968, -3.505236298600246325, -18.68346056562440793 ) ) ;
#8531 = PLANE ( 'NONE',  #24856 ) ;
#8532 = CARTESIAN_POINT ( 'NONE',  ( 68.92755183904094451, -25.82220866885473853, -5.893215200338315363 ) ) ;
#8533 = CARTESIAN_POINT ( 'NONE',  ( 111.8886348109120092, -6.222761293078241884, -8.102969835052219238 ) ) ;
#8534 = CARTESIAN_POINT ( 'NONE',  ( 119.0929214775786278, -5.638512984488999180, -18.83840828888717311 ) ) ;
#8535 = ORIENTED_EDGE ( 'NONE', *, *, #34388, .F. ) ;
#8536 = AXIS2_PLACEMENT_3D ( 'NONE', #4000, #591, #38882 ) ;
#8537 = CARTESIAN_POINT ( 'NONE',  ( 117.1074881442453233, 0.4262465694468514643, -12.03445270309931736 ) ) ;
#8538 = CARTESIAN_POINT ( 'NONE',  ( 113.4769814775786330, -10.63000616557722466, -14.87417383870573495 ) ) ;
#8539 = CARTESIAN_POINT ( 'NONE',  ( 120.8514481442452961, -7.893985811506177619, -18.51759400769804742 ) ) ;
#8540 = CARTESIAN_POINT ( 'NONE',  ( 118.9794681442453026, -0.8288870151387760510, -10.36305467784173118 ) ) ;
#8541 = VERTEX_POINT ( 'NONE', #34839 ) ;
#8542 = CARTESIAN_POINT ( 'NONE',  ( 123.7445081442452874, -7.894159318335828068, -9.358103419637847864 ) ) ;
#8543 = CARTESIAN_POINT ( 'NONE',  ( 119.6034614775786196, -6.344957434206665248, -7.627207830600338134 ) ) ;
#8544 = CARTESIAN_POINT ( 'NONE',  ( 125.1028739313154148, -6.088305799123888917, -6.024550168534809735 ) ) ;
#8545 = VECTOR ( 'NONE', #10028, 1000.000000000000000 ) ;
#8546 = CARTESIAN_POINT ( 'NONE',  ( 120.7947214775786193, -9.261995988541697145, -16.69588392320189030 ) ) ;
#8547 = DIRECTION ( 'NONE',  ( 0.9609149988134843001, -0.1028163501681632064, 0.2570431154366505933 ) ) ;
#8548 = CARTESIAN_POINT ( 'NONE',  ( 70.19189222814998175, -51.68868231262963775, -33.87830190084585524 ) ) ;
#8549 = CARTESIAN_POINT ( 'NONE',  ( 138.0385288853987049, -1.837662360184606714, -16.17424470069298081 ) ) ;
#8550 = CARTESIAN_POINT ( 'NONE',  ( 115.9693640045247776, 0.1403307496149616695, -15.46607636864997204 ) ) ;
#8551 = CARTESIAN_POINT ( 'NONE',  ( 123.2855641859119942, -8.321307733199551748, -9.223433127585318303 ) ) ;
#8552 = CYLINDRICAL_SURFACE ( 'NONE', #38978, 1.499999999999998002 ) ;
#8553 = CARTESIAN_POINT ( 'NONE',  ( 116.4267681442453153, -6.222761293078241884, -8.102969835052219238 ) ) ;
#8554 = CARTESIAN_POINT ( 'NONE',  ( 111.7751814775786556, -2.084020599724406786, -8.691656652584148546 ) ) ;
#8555 = CARTESIAN_POINT ( 'NONE',  ( 65.55689610126231059, -13.67296395165911704, -14.39321520033831625 ) ) ;
#8556 = ORIENTED_EDGE ( 'NONE', *, *, #11389, .T. ) ;
#8557 = CARTESIAN_POINT ( 'NONE',  ( 116.8028015045247940, -6.936859964151250502, -18.39754474579286025 ) ) ;
#8558 = CARTESIAN_POINT ( 'NONE',  ( 109.3018640045248304, 0.1403307496149616695, -15.46607636864997204 ) ) ;
#8559 = VECTOR ( 'NONE', #1263, 1000.000000000000000 ) ;
#8560 = CARTESIAN_POINT ( 'NONE',  ( 115.9729548109119861, -3.505236298600246325, -18.68346056562440793 ) ) ;
#8561 = FACE_OUTER_BOUND ( 'NONE', #44889, .T. ) ;
#8562 = EDGE_CURVE ( 'NONE', #18186, #10189, #15022, .T. ) ;
#8563 = CARTESIAN_POINT ( 'NONE',  ( 124.0229291344827516, -1.149058757900107697, -17.09122335155391781 ) ) ;
#8565 = CARTESIAN_POINT ( 'NONE',  ( 119.7169148109119874, -9.988377603198976828, -10.36322818467138340 ) ) ;
#8564 = CARTESIAN_POINT ( 'NONE',  ( 62.83933201006751545, -13.37155033267121951, -8.024690356892984155 ) ) ;
#8566 = CARTESIAN_POINT ( 'NONE',  ( 121.6456214775786293, 0.4262465694468514643, -12.03445270309931736 ) ) ;
#8567 = ORIENTED_EDGE ( 'NONE', *, *, #587, .T. ) ;
#8568 = CARTESIAN_POINT ( 'NONE',  ( 114.6936464071293784, 0.2518737723193609224, -14.64321520033831447 ) ) ;
#8569 = CARTESIAN_POINT ( 'NONE',  ( 126.0135748109119902, -8.166667518702819706, -8.995218007635861213 ) ) ;
#8570 = CARTESIAN_POINT ( 'NONE',  ( 108.0517077545248696, -2.791137627527939813, -18.39754474579286025 ) ) ;
#8571 = CARTESIAN_POINT ( 'NONE',  ( 123.9714148109119805, -8.899110576539710493, -16.42337572283490132 ) ) ;
#8572 = CARTESIAN_POINT ( 'NONE',  ( 122.4965214775786251, 0.1319031606808879209, -14.10382304977623669 ) ) ;
#8573 = CARTESIAN_POINT ( 'NONE',  ( 114.8384214775786489, -10.15424416112533912, -14.75197769757731336 ) ) ;
#8574 = CARTESIAN_POINT ( 'NONE',  ( 120.8842620163423192, -1.087735405160626723, -17.17288456429612964 ) ) ;
#8575 = CARTESIAN_POINT ( 'NONE',  ( 108.3989733795248753, -8.938348069036489818, -17.46756447353520159 ) ) ;
#8576 = CARTESIAN_POINT ( 'NONE',  ( 125.5597614775786326, -7.894159318335828068, -9.358103419637847864 ) ) ;
#8577 = CARTESIAN_POINT ( 'NONE',  ( 122.2128881442453263, -7.643976991954077427, -18.09477374809248928 ) ) ;
#8578 = CARTESIAN_POINT ( 'NONE',  ( 112.1722681442453222, -8.899110576539710493, -16.42337572283490132 ) ) ;
#8579 = DIRECTION ( 'NONE',  ( 1.000000000000000000, 0.000000000000000000, 0.000000000000000000 ) ) ;
#8580 = VECTOR ( 'NONE', #22463, 999.9999999999998863 ) ;
#8581 = CARTESIAN_POINT ( 'NONE',  ( 114.4413952545248350, 0.8980012041604421569, -11.00651665394454071 ) ) ;
#8582 = EDGE_CURVE ( 'NONE', #34725, #29032, #7171, .T. ) ;
#8583 = DIRECTION ( 'NONE',  ( 0.000000000000000000, 0.000000000000000000, 1.000000000000000000 ) ) ;
#8584 = CARTESIAN_POINT ( 'NONE',  ( 121.4754414775786131, -8.166667518702819706, -8.995218007635861213 ) ) ;
#8585 = CARTESIAN_POINT ( 'NONE',  ( 118.5256548109119876, -0.4660016031367893996, -10.09054647747474043 ) ) ;
#8586 = CARTESIAN_POINT ( 'NONE',  ( 107.7738952545248310, 0.8980012041604421569, -11.00651665394454071 ) ) ;
#8587 = CARTESIAN_POINT ( 'NONE',  ( 116.0296814775786345, -8.166667518702817929, -8.995218007635861213 ) ) ;
#8588 = EDGE_CURVE ( 'NONE', #34274, #33082, #4331, .T. ) ;
#8589 = ADVANCED_FACE ( 'NONE', ( #3844 ), #28933, .T. ) ;
#8590 = CARTESIAN_POINT ( 'NONE',  ( 87.44708369096657918, -21.99489077589588604, -6.893215200338315363 ) ) ;
#8591 = ORIENTED_EDGE ( 'NONE', *, *, #3448, .F. ) ;
#8592 = CARTESIAN_POINT ( 'NONE',  ( 116.5263184158184799, -9.825083310266851555, -11.28323190290009492 ) ) ;
#8593 = CARTESIAN_POINT ( 'NONE',  ( 119.0929214775786278, -5.638512984488999180, -18.83840828888717311 ) ) ;
#8594 = CARTESIAN_POINT ( 'NONE',  ( 123.9714148109119805, -8.899110576539710493, -16.42337572283490132 ) ) ;
#8595 = SHAPE_DEFINITION_REPRESENTATION ( #41973, #15458 ) ;
#8596 = CARTESIAN_POINT ( 'NONE',  ( 114.3846081442453197, 0.4262465694468514643, -12.03445270309931736 ) ) ;
#8597 = CARTESIAN_POINT ( 'NONE',  ( 111.8319081442453182, -4.153390946401321671, -8.397313243818183892 ) ) ;
#8598 = CARTESIAN_POINT ( 'NONE',  ( 108.8156921295247912, 0.8980012041604618078, -13.39321520033831447 ) ) ;
#8599 = CARTESIAN_POINT ( 'NONE',  ( 119.3765548109119834, -10.15424416112533912, -14.75197769757731336 ) ) ;
#8600 = CARTESIAN_POINT ( 'NONE',  ( 83.46705746533211823, -32.83968548964498524, -20.89321520033831092 ) ) ;
#8601 = CARTESIAN_POINT ( 'NONE',  ( 116.3860827545247787, -2.477300249445798297, -19.15521520033831138 ) ) ;
#8602 = ORIENTED_EDGE ( 'NONE', *, *, #33649, .T. ) ;
#8603 = CARTESIAN_POINT ( 'NONE',  ( 72.54180985774836188, -60.65691546915440568, -36.73639088572416966 ) ) ;
#8604 = CARTESIAN_POINT ( 'NONE',  ( 123.4041481442452834, -10.30919188438810075, -12.61870101168855918 ) ) ;
#8605 = ADVANCED_FACE ( 'NONE', ( #28710 ), #17988, .T. ) ;
#8606 = CARTESIAN_POINT ( 'NONE',  ( 125.6732148109119862, -9.859900752359378018, -12.68260735090039759 ) ) ;
#8607 = CARTESIAN_POINT ( 'NONE',  ( 91.11246428952674137, -25.99489077589524300, -13.39321520033831625 ) ) ;
#8608 = SURFACE_STYLE_USAGE ( .BOTH. , #39845 ) ;
#8609 = VECTOR ( 'NONE', #42176, 1000.000000000000000 ) ;
#8610 = CARTESIAN_POINT ( 'NONE',  ( 118.2987481442453088, -7.894159318335828068, -9.358103419637847864 ) ) ;
#8611 = DIRECTION ( 'NONE',  ( -0.2768435750659241079, -0.3568721902840695792, 0.8921882507333129819 ) ) ;
#8612 = CARTESIAN_POINT ( 'NONE',  ( 64.86955682001475054, -35.96757841592401661, -5.723731037142695044 ) ) ;
#8613 = EDGE_CURVE ( 'NONE', #5955, #24054, #2777, .T. ) ;
#8614 = CARTESIAN_POINT ( 'NONE',  ( 124.1983214775786166, -1.833838273342659697, -17.42832698103878286 ) ) ;
#8615 = CARTESIAN_POINT ( 'NONE',  ( 109.8405644685027767, 0.6938714319018670640, -14.64321520033831447 ) ) ;
#8616 = CARTESIAN_POINT ( 'NONE',  ( 124.3685014775786328, 0.4262465694468514643, -12.03445270309931736 ) ) ;
#8617 = ADVANCED_FACE ( 'NONE', ( #25288 ), #12363, .T. ) ;
#8618 = CARTESIAN_POINT ( 'NONE',  ( 125.2748812523276598, -11.53675367988898159, -16.14795873962287232 ) ) ;
#8619 = CARTESIAN_POINT ( 'NONE',  ( 122.6099748109119929, -9.261995988541697145, -16.69588392320189030 ) ) ;
#8620 = CARTESIAN_POINT ( 'NONE',  ( 116.9940348109119839, -0.1624402480850797581, -16.17319339645315424 ) ) ;
#8621 = CARTESIAN_POINT ( 'NONE',  ( 124.3117748109119844, 0.1319031606808879209, -14.10382304977623669 ) ) ;
#8622 = CARTESIAN_POINT ( 'NONE',  ( 120.1707281442453166, 0.2603800115204892296, -16.42320221600525088 ) ) ;
#8623 = CARTESIAN_POINT ( 'NONE',  ( 115.1220548109119761, -8.166667518702817929, -8.995218007635861213 ) ) ;
#8624 = CARTESIAN_POINT ( 'NONE',  ( 115.5526452545247622, -9.868328341294098749, -15.46607636864997204 ) ) ;
#8625 = CARTESIAN_POINT ( 'NONE',  ( 125.1059481442452750, -1.833838273342660141, -17.42832698103878286 ) ) ;
#8626 = ORIENTED_EDGE ( 'NONE', *, *, #35895, .F. ) ;
#8627 = CARTESIAN_POINT ( 'NONE',  ( 118.7525614775786380, -8.166667518702819706, -8.995218007635861213 ) ) ;
#8628 = CARTESIAN_POINT ( 'NONE',  ( 116.3860827545247787, -2.477300249445798297, -19.15521520033831138 ) ) ;
#8629 = CARTESIAN_POINT ( 'NONE',  ( 110.9687390045248350, -9.868328341294098749, -11.32035403202665869 ) ) ;
#8630 = DIRECTION ( 'NONE',  ( 0.000000000000000000, 0.9284778069183722282, 0.3713878862591645791 ) ) ;
#8631 = CARTESIAN_POINT ( 'NONE',  ( 112.3424481442453384, -3.505236298600246325, -18.68346056562440793 ) ) ;
#8632 = CARTESIAN_POINT ( 'NONE',  ( 59.75121349346655109, -13.58877957849837692, -7.404803486908546617 ) ) ;
#8633 = CARTESIAN_POINT ( 'NONE',  ( 116.5249890045247980, -9.868328341294098749, -11.32035403202665869 ) ) ;
#8634 = ORIENTED_EDGE ( 'NONE', *, *, #27571, .F. ) ;
#8635 = CARTESIAN_POINT ( 'NONE',  ( 123.9146881442452894, -10.15424416112533912, -14.75197769757731336 ) ) ;
#8636 = CARTESIAN_POINT ( 'NONE',  ( 122.2437673109119629, 0.2312338769422704887, -16.08380026872395874 ) ) ;
#8637 = FACE_OUTER_BOUND ( 'NONE', #32018, .T. ) ;
#8638 = EDGE_CURVE ( 'NONE', #529, #18915, #28179, .T. ) ;
#8639 = CARTESIAN_POINT ( 'NONE',  ( 111.9559014775786494, -9.522524984348095245, -10.63868154973201108 ) ) ;
#8640 = CARTESIAN_POINT ( 'NONE',  ( 109.6491296295247793, -4.863998795839590272, -8.388885654883775800 ) ) ;
#8641 = ORIENTED_EDGE ( 'NONE', *, *, #25857, .T. ) ;
#8642 = CARTESIAN_POINT ( 'NONE',  ( 114.5547881442453217, -5.638512984488999180, -18.83840828888717311 ) ) ;
#8643 = CARTESIAN_POINT ( 'NONE',  ( 88.58241854558018247, -11.31884705245859735, -13.99297490352741846 ) ) ;
#8644 = CARTESIAN_POINT ( 'NONE',  ( 123.9714148109119805, -8.899110576539710493, -16.42337572283490132 ) ) ;
#8645 = CARTESIAN_POINT ( 'NONE',  ( 113.9875214775786532, -8.899110576539710493, -16.42337572283490132 ) ) ;
#8646 = CYLINDRICAL_SURFACE ( 'NONE', #8929, 1.999999999999998668 ) ;
#8647 = CARTESIAN_POINT ( 'NONE',  ( 124.4819548109119722, -7.893985811506201600, -18.51759400769803676 ) ) ;
#8648 = CARTESIAN_POINT ( 'NONE',  ( 113.3635281442453504, -9.988377603198976828, -10.36322818467138340 ) ) ;
#8649 = CARTESIAN_POINT ( 'NONE',  ( 109.7185827545247889, -6.936859964151250502, -8.388885654883777576 ) ) ;
#8650 = CARTESIAN_POINT ( 'NONE',  ( 123.2906948109119867, -8.166667518702819706, -8.995218007635861213 ) ) ;
#8651 = CARTESIAN_POINT ( 'NONE',  ( 136.1332990479132263, -10.31707786543337058, -15.60180518456300547 ) ) ;
#8652 = EDGE_LOOP ( 'NONE', ( #17737, #4182, #20743, #6194, #39504 ) ) ;
#8653 = CARTESIAN_POINT ( 'NONE',  ( 114.4980614775786592, -7.893985811506177619, -18.51759400769804742 ) ) ;
#8654 = CARTESIAN_POINT ( 'NONE',  ( 125.9568481442452850, -6.344957434206665248, -7.627207830600338134 ) ) ;
#8655 = CARTESIAN_POINT ( 'NONE',  ( 105.6903015045248253, -2.477300249445798297, -7.631215200338321125 ) ) ;
#8656 = CARTESIAN_POINT ( 'NONE',  ( 112.3424481442453384, -6.344957434206662583, -7.627207830600332805 ) ) ;
#8657 = ORIENTED_EDGE ( 'NONE', *, *, #34603, .T. ) ;
#8658 = CARTESIAN_POINT ( 'NONE',  ( 119.6601881442453106, -8.166667518702819706, -8.995218007635861213 ) ) ;
#8659 = DIRECTION ( 'NONE',  ( 0.9609149988134837450, -0.1028163501681639419, 0.2570431154366518145 ) ) ;
#8660 = LINE ( 'NONE', #23248, #9499 ) ;
#8661 = CARTESIAN_POINT ( 'NONE',  ( 120.1332064091100733, -0.9924539043446216624, -17.29976612834909133 ) ) ;
#8662 = CARTESIAN_POINT ( 'NONE',  ( 136.9012041053388486, -2.916721388012065930, -8.216909731286408558 ) ) ;
#8663 = CARTESIAN_POINT ( 'NONE',  ( 114.1009748109119784, -5.574606645277164318, -18.38911715685844683 ) ) ;
#8664 = CARTESIAN_POINT ( 'NONE',  ( 70.19189222814998175, -59.83749578782295941, -37.13779888561150244 ) ) ;
#8665 = CIRCLE ( 'NONE', #29794, 2.445500000000005336 ) ;
#8666 = DIRECTION ( 'NONE',  ( -0.000000000000000000, -0.9284778069183720062, -0.3713878862591650232 ) ) ;
#8667 = CARTESIAN_POINT ( 'NONE',  ( 113.8740681442453138, -9.859900752359374465, -12.68260735090039404 ) ) ;
#8668 = CARTESIAN_POINT ( 'NONE',  ( 112.0588148109119828, 0.5811942927096154232, -14.16772938898807155 ) ) ;
#8669 = CARTESIAN_POINT ( 'NONE',  ( 116.6178968253198605, -9.773106258948061509, -14.47218176588315508 ) ) ;
#8670 = CARTESIAN_POINT ( 'NONE',  ( 122.6667014775786413, -2.084020599724406786, -8.691656652584148546 ) ) ;
#8671 = FACE_OUTER_BOUND ( 'NONE', #44083, .T. ) ;
#8672 = CARTESIAN_POINT ( 'NONE',  ( 123.9714148109119805, -0.4660016031367893996, -10.09054647747474043 ) ) ;
#8673 = EDGE_CURVE ( 'NONE', #3446, #22843, #29729, .T. ) ;
#8674 = CARTESIAN_POINT ( 'NONE',  ( 121.9292548109119849, -1.561330072975668948, -17.79121239304076951 ) ) ;
#8675 = ORIENTED_EDGE ( 'NONE', *, *, #24760, .T. ) ;
#8676 = CARTESIAN_POINT ( 'NONE',  ( 136.4689272580744444, 0.8652765085456386451, -12.77968882490968561 ) ) ;
#8677 = CARTESIAN_POINT ( 'NONE',  ( 110.3436608795247764, -8.938348069036489818, -9.318865927141430916 ) ) ;
#8678 = CARTESIAN_POINT ( 'NONE',  ( 109.9269421295247753, -9.868328341294093420, -13.39321520033831447 ) ) ;
#8679 = CARTESIAN_POINT ( 'NONE',  ( 107.7044421295247929, -9.868328341294093420, -13.39321520033831447 ) ) ;
#8680 = CARTESIAN_POINT ( 'NONE',  ( 127.7429221096635672, -10.18842876247218499, -11.18798664339182380 ) ) ;
#8681 = CARTESIAN_POINT ( 'NONE',  ( 116.6536748109119941, 0.9020085738987339008, -11.91225656197089222 ) ) ;
#8682 = ORIENTED_EDGE ( 'NONE', *, *, #7862, .T. ) ;
#8683 = CARTESIAN_POINT ( 'NONE',  ( 107.2877233795247776, -8.938348069036489818, -17.46756447353520159 ) ) ;
#8684 = CARTESIAN_POINT ( 'NONE',  ( 119.4332814775786318, -8.899110576539721151, -16.42337572283488711 ) ) ;
#8685 = CARTESIAN_POINT ( 'NONE',  ( 115.0086014775786509, -5.574606645277164318, -18.38911715685844683 ) ) ;
#8686 = CARTESIAN_POINT ( 'NONE',  ( 112.5126281442453120, -10.30919188438810075, -12.61870101168855918 ) ) ;
#8687 = CARTESIAN_POINT ( 'NONE',  ( 120.1140014775786398, -1.561330072975668504, -17.79121239304076951 ) ) ;
#8688 = CARTESIAN_POINT ( 'NONE',  ( 109.5102233795247884, -8.938348069036489818, -17.46756447353520159 ) ) ;
#8689 = CARTESIAN_POINT ( 'NONE',  ( 74.19189222814998175, -41.76310523276723785, -24.39321520033831447 ) ) ;
#8690 = ORIENTED_EDGE ( 'NONE', *, *, #20333, .F. ) ;
#8691 = CARTESIAN_POINT ( 'NONE',  ( 73.07463722459043254, -60.35343162539949446, -36.44966353086839206 ) ) ;
#8692 = CARTESIAN_POINT ( 'NONE',  ( 120.1707281442453166, -9.565557343593413364, -10.61323700422348004 ) ) ;
#8693 = CARTESIAN_POINT ( 'NONE',  ( 114.4413348109119823, -9.261995988541697145, -16.69588392320189030 ) ) ;
#8694 = CARTESIAN_POINT ( 'NONE',  ( 113.7038881442453402, -3.383040157471821630, -19.15922257007629170 ) ) ;
#8695 = LINE ( 'NONE', #22827, #15563 ) ;
#8696 = EDGE_CURVE ( 'NONE', #43595, #31077, #32110, .T. ) ;
#8697 = CARTESIAN_POINT ( 'NONE',  ( 122.0427081442452817, -9.859900752359378018, -12.68260735090039759 ) ) ;
#8698 = CARTESIAN_POINT ( 'NONE',  ( 117.7882081442453170, -3.505236298600246325, -18.68346056562440793 ) ) ;
#8699 = ORIENTED_EDGE ( 'NONE', *, *, #10836, .F. ) ;
#8700 = CARTESIAN_POINT ( 'NONE',  ( 122.5215798109119874, -7.200787124940443817, -17.81845355600750835 ) ) ;
#8701 = CIRCLE ( 'NONE', #10894, 2.999999999999999556 ) ;
#8702 = CARTESIAN_POINT ( 'NONE',  ( 114.1009748109119784, -4.089484607189486809, -7.948022111789456723 ) ) ;
#8703 = CARTESIAN_POINT ( 'NONE',  ( 118.4689281442453250, -10.15424416112533912, -14.75197769757731336 ) ) ;
#8704 = ORIENTED_EDGE ( 'NONE', *, *, #31525, .F. ) ;
#8705 = VECTOR ( 'NONE', #13012, 1000.000000000000000 ) ;
#8706 = CARTESIAN_POINT ( 'NONE',  ( 110.8116360982116788, 0.3867979994853637526, -12.14321520033833224 ) ) ;
#8707 = CARTESIAN_POINT ( 'NONE',  ( 113.3635281442453504, -9.988377603198976828, -10.36322818467138340 ) ) ;
#8708 = CARTESIAN_POINT ( 'NONE',  ( 115.9693640045247776, -10.62599879583958717, -11.00651665394454604 ) ) ;
#8709 = CARTESIAN_POINT ( 'NONE',  ( 113.7038881442453402, -6.222761293078241884, -8.102969835052219238 ) ) ;
#8710 = ORIENTED_EDGE ( 'NONE', *, *, #24838, .T. ) ;
#8711 = ORIENTED_EDGE ( 'NONE', *, *, #24211, .F. ) ;
#8712 = CARTESIAN_POINT ( 'NONE',  ( 123.2339681442453241, -3.505236298600246325, -18.68346056562440793 ) ) ;
#8713 = CARTESIAN_POINT ( 'NONE',  ( 122.8368814775786291, -7.894159318335828068, -9.358103419637847864 ) ) ;
#8714 =( BOUNDED_CURVE ( )  B_SPLINE_CURVE ( 3, ( #34923, #31084, #14208, #14653 ),
 .UNSPECIFIED., .F., .F. ) 
 B_SPLINE_CURVE_WITH_KNOTS ( ( 4, 4 ),
 ( 1.570796326794895004, 2.525095272406109981 ),
 .UNSPECIFIED. ) 
 CURVE ( )  GEOMETRIC_REPRESENTATION_ITEM ( )  RATIONAL_B_SPLINE_CURVE ( ( 1.000000000000000000, 0.9255384209705489473, 0.9255384209705489473, 1.000000000000000000 ) ) 
 REPRESENTATION_ITEM ( '' )  );
#8715 = FACE_BOUND ( 'NONE', #13443, .T. ) ;
#8716 = ORIENTED_EDGE ( 'NONE', *, *, #40630, .F. ) ;
#8717 = FACE_OUTER_BOUND ( 'NONE', #37955, .T. ) ;
#8718 = CARTESIAN_POINT ( 'NONE',  ( 61.85355368920866681, -65.73604765264855132, -43.91139043025361133 ) ) ;
#8719 = CARTESIAN_POINT ( 'NONE',  ( 105.4819421295248247, 0.8980012041604618078, -13.39321520033831447 ) ) ;
#8720 = CARTESIAN_POINT ( 'NONE',  ( 115.8595014775786609, -1.834011780172310813, -8.268836392978581529 ) ) ;
#8722 = CARTESIAN_POINT ( 'NONE',  ( 115.1787814775786387, -0.1624402480850797581, -16.17319339645315424 ) ) ;
#8721 = CARTESIAN_POINT ( 'NONE',  ( 114.1577014775786552, -6.344957434206662583, -7.627207830600332805 ) ) ;
#8723 = CARTESIAN_POINT ( 'NONE',  ( 120.6812681442452941, 0.1319031606808879209, -14.10382304977623669 ) ) ;
#8724 = DIRECTION ( 'NONE',  ( 0.000000000000000000, 0.000000000000000000, 1.000000000000000000 ) ) ;
#8725 = VERTEX_POINT ( 'NONE', #41944 ) ;
#8726 = CARTESIAN_POINT ( 'NONE',  ( 120.1707281442453166, -9.565557343593413364, -10.61323700422348004 ) ) ;
#8727 = CARTESIAN_POINT ( 'NONE',  ( 123.4608748109119745, 0.4262465694468514643, -12.03445270309931736 ) ) ;
#8728 = CARTESIAN_POINT ( 'NONE',  ( 113.4690515045247992, -2.477300249445798297, -7.631215200338321125 ) ) ;
#8729 = CARTESIAN_POINT ( 'NONE',  ( 70.19189222814998175, -59.83749578782295941, -37.13779888561150244 ) ) ;
#8730 = CARTESIAN_POINT ( 'NONE',  ( 112.2188952545247531, 0.8980012041604421569, -11.00651665394454071 ) ) ;
#8731 = AXIS2_PLACEMENT_3D ( 'NONE', #14846, #43333, #12102 ) ;
#8732 = CARTESIAN_POINT ( 'NONE',  ( 117.9583881442453048, -10.30919188438810075, -12.61870101168855918 ) ) ;
#8733 = ORIENTED_EDGE ( 'NONE', *, *, #9214, .T. ) ;
#8734 = CARTESIAN_POINT ( 'NONE',  ( 122.3830681442452857, -8.166667518702819706, -8.995218007635861213 ) ) ;
#8735 = CARTESIAN_POINT ( 'NONE',  ( 115.1010702440515558, -2.467220198592777525, -17.83387418641524391 ) ) ;
#8736 = CARTESIAN_POINT ( 'NONE',  ( 108.4684265045247997, -7.250697342233347165, -19.15521520033831138 ) ) ;
#8737 = CARTESIAN_POINT ( 'NONE',  ( 115.1220548109119761, -8.166667518702817929, -8.995218007635861213 ) ) ;
#8738 = CARTESIAN_POINT ( 'NONE',  ( 117.6180281442453150, -0.4660016031367893996, -10.09054647747474043 ) ) ;
#8739 = DIRECTION ( 'NONE',  ( 0.000000000000000000, 0.000000000000000000, 1.000000000000000000 ) ) ;
#8740 = CARTESIAN_POINT ( 'NONE',  ( 117.1427234793119396, -11.22998347280470455, -5.531657149556616915 ) ) ;
#8741 = ORIENTED_EDGE ( 'NONE', *, *, #18790, .F. ) ;
#8742 = CARTESIAN_POINT ( 'NONE',  ( -1.803662125172398545, -6.825544624776664904, -8.166198927921115569 ) ) ;
#8743 = CIRCLE ( 'NONE', #40052, 2.999999999999999556 ) ;
#8744 = CARTESIAN_POINT ( 'NONE',  ( 109.2294576096139878, -8.937404933060426160, -16.93127305845157338 ) ) ;
#8745 = CARTESIAN_POINT ( 'NONE',  ( 120.2841814775786276, -10.15424416112533912, -14.75197769757731336 ) ) ;
#8746 = ADVANCED_FACE ( 'NONE', ( #1105 ), #10708, .T. ) ;
#8747 = CARTESIAN_POINT ( 'NONE',  ( 109.9963952545248134, -9.868328341294098749, -15.46607636864997204 ) ) ;
#8748 = CARTESIAN_POINT ( 'NONE',  ( 114.7886608795247696, -1.325403438956436419, -16.93181055722141792 ) ) ;
#8749 = VECTOR ( 'NONE', #30706, 1000.000000000000000 ) ;
#8750 = CARTESIAN_POINT ( 'NONE',  ( 119.1496481442453046, -6.222761293078241884, -8.102969835052219238 ) ) ;
#8751 = DIRECTION ( 'NONE',  ( 0.000000000000000000, 0.6004852223388321697, -0.7996358532186279566 ) ) ;
#8752 = CARTESIAN_POINT ( 'NONE',  ( 70.07290130439605491, -26.13131486452389041, -5.723131632646605738 ) ) ;
#8753 = CARTESIAN_POINT ( 'NONE',  ( 111.8319081442453182, -4.153390946401321671, -8.397313243818183892 ) ) ;
#8754 = CARTESIAN_POINT ( 'NONE',  ( 118.2420214775786320, -3.383040157471821630, -19.15922257007629170 ) ) ;
#8755 = ORIENTED_EDGE ( 'NONE', *, *, #16476, .F. ) ;
#8756 = CARTESIAN_POINT ( 'NONE',  ( 118.6958348109119754, -3.505236298600246325, -18.68346056562440793 ) ) ;
#8757 = CARTESIAN_POINT ( 'NONE',  ( 115.1220548109119761, -8.166667518702817929, -8.995218007635861213 ) ) ;
#8758 = CARTESIAN_POINT ( 'NONE',  ( 121.2485348109119769, -0.4660016031367893996, -10.09054647747474043 ) ) ;
#8759 = CARTESIAN_POINT ( 'NONE',  ( 118.4122014775786340, -9.859900752359374465, -12.68260735090039404 ) ) ;
#8760 = VERTEX_POINT ( 'NONE', #9082 ) ;
#8761 = CARTESIAN_POINT ( 'NONE',  ( 124.9357681442453014, -7.643976991954077427, -18.09477374809248928 ) ) ;
#8762 = CARTESIAN_POINT ( 'NONE',  ( 120.5110881442453206, -6.344957434206665248, -7.627207830600338134 ) ) ;
#8763 = CONICAL_SURFACE ( 'NONE', #16061, 1.610000000000000986, 0.9599310885968765916 ) ;
#8764 = CARTESIAN_POINT ( 'NONE',  ( 125.2231329858104516, -7.806516698891761585, -6.696497996897097238 ) ) ;
#8765 = CARTESIAN_POINT ( 'NONE',  ( 120.9081748109119872, -5.638512984488999180, -18.83840828888717311 ) ) ;
#8766 = CARTESIAN_POINT ( 'NONE',  ( 108.1211608795247798, -8.938348069036489818, -9.318865927141430916 ) ) ;
#8767 = DIRECTION ( 'NONE',  ( 0.000000000000000000, 0.000000000000000000, -1.000000000000000000 ) ) ;
#8768 = CARTESIAN_POINT ( 'NONE',  ( 119.1871698793805194, -2.191907684172563986, -18.20049396185734025 ) ) ;
#8769 = CARTESIAN_POINT ( 'NONE',  ( 107.2877233795247776, -1.325403438956436419, -9.854619843455211026 ) ) ;
#8770 = AXIS2_PLACEMENT_3D ( 'NONE', #40267, #32948, #18837 ) ;
#8771 = CARTESIAN_POINT ( 'NONE',  ( 123.5633766859119760, -9.033780868592240054, -16.85052413769862056 ) ) ;
#8772 = CIRCLE ( 'NONE', #18967, 8.000000000000001776 ) ;
#8773 = CARTESIAN_POINT ( 'NONE',  ( 137.0596819398122932, -9.972289680933823064, -11.58104143152225163 ) ) ;
#8774 = CARTESIAN_POINT ( 'NONE',  ( 119.5467348109119712, -5.574606645277164318, -18.38911715685844683 ) ) ;
#8775 = CARTESIAN_POINT ( 'NONE',  ( 125.7299414775786346, 0.9020085738987339008, -11.91225656197089222 ) ) ;
#8776 = LINE ( 'NONE', #33149, #17752 ) ;
#8777 = ORIENTED_EDGE ( 'NONE', *, *, #42324, .F. ) ;
#8778 = CARTESIAN_POINT ( 'NONE',  ( 116.3198046295247963, -4.863998795839590272, -8.393215200338314474 ) ) ;
#8779 = CARTESIAN_POINT ( 'NONE',  ( 109.0240515045248202, -6.936859964151250502, -18.39754474579286025 ) ) ;
#8780 = CARTESIAN_POINT ( 'NONE',  ( 115.0653281442453277, -3.505236298600246325, -18.68346056562440793 ) ) ;
#8781 = CARTESIAN_POINT ( 'NONE',  ( 114.9073801386228979, -1.125321370491268125, -17.12283323191015327 ) ) ;
#8782 = CARTESIAN_POINT ( 'NONE',  ( 66.90558936096920206, -0.06963689119154935214, -10.39321520033831803 ) ) ;
#8783 = CARTESIAN_POINT ( 'NONE',  ( 86.09323753712084226, -25.99489077589524300, -13.39321520033831625 ) ) ;
#8785 = CARTESIAN_POINT ( 'NONE',  ( 124.5386814775786206, -5.638512984488999180, -18.83840828888717311 ) ) ;
#8784 = CARTESIAN_POINT ( 'NONE',  ( 86.51169734173754478, -25.99489077589583630, -7.893215200338315363 ) ) ;
#8786 = CARTESIAN_POINT ( 'NONE',  ( 122.8368814775786291, -7.894159318335828068, -9.358103419637847864 ) ) ;
#8787 = EDGE_LOOP ( 'NONE', ( #34111, #19882, #40972, #9487 ) ) ;
#8788 = CARTESIAN_POINT ( 'NONE',  ( 110.0654504682428865, 0.5115630086001619059, -14.64321520033831447 ) ) ;
#8789 = CARTESIAN_POINT ( 'NONE',  ( 125.8433948109119456, -1.834011780172310813, -8.268836392978581529 ) ) ;
#8790 = CARTESIAN_POINT ( 'NONE',  ( 110.6909265045248247, -2.791137627527939813, -8.388885654883777576 ) ) ;
#8791 = CARTESIAN_POINT ( 'NONE',  ( 120.5678148109119832, -1.833838273342659253, -17.42832698103878286 ) ) ;
#8792 = CARTESIAN_POINT ( 'NONE',  ( 119.6601881442453106, -1.833838273342659253, -17.42832698103878286 ) ) ;
#8793 = CARTESIAN_POINT ( 'NONE',  ( 120.5887993777725029, -1.267766418764730840, -16.93314635290706605 ) ) ;
#8794 = CARTESIAN_POINT ( 'NONE',  ( 106.2459265045248173, -7.250697342233347165, -19.15521520033831138 ) ) ;
#8795 = FACE_OUTER_BOUND ( 'NONE', #5674, .T. ) ;
#8796 = LINE ( 'NONE', #43007, #23813 ) ;
#8797 = AXIS2_PLACEMENT_3D ( 'NONE', #36651, #29375, #5424 ) ;
#8798 = CYLINDRICAL_SURFACE ( 'NONE', #12473, 4.999999999999998224 ) ;
#8799 = CARTESIAN_POINT ( 'NONE',  ( 110.6214733795247867, -8.938348069036489818, -17.46756447353520159 ) ) ;
#8800 =( BOUNDED_CURVE ( )  B_SPLINE_CURVE ( 2, ( #2164, #12454, #26356, #23389, #40263, #43913, #5815, #19734, #26580, #6042, #9255, #16555, #44598, #10607, #34955, #6958, #10385 ),
 .UNSPECIFIED., .F., .T. ) 
 B_SPLINE_CURVE_WITH_KNOTS ( ( 3, 2, 2, 2, 2, 2, 2, 2, 3 ),
 ( 0.3295046674808919662, 0.3359375000000000000, 0.3437500000000000000, 0.3515625000000000000, 0.3593750000000000000, 0.3671875000000000000, 0.3750000000000000000, 0.3828125000000000000, 0.3892453325190585178 ),
 .UNSPECIFIED. ) 
 CURVE ( )  GEOMETRIC_REPRESENTATION_ITEM ( )  RATIONAL_B_SPLINE_CURVE ( ( 0.9778625265006459788, 0.9373222120152210346, 1.000000000000000000, 0.9238795325112869605, 1.000000000000000000, 0.9238795325112869605, 1.000000000000000000, 0.9238795325112869605, 1.000000000000000000, 0.9238795325112869605, 1.000000000000000000, 0.9238795325112869605, 1.000000000000000000, 0.9238795325112869605, 1.000000000000000000, 0.9373222120157019832, 0.9778625265000240319 ) ) 
 REPRESENTATION_ITEM ( '' )  );
#8801 = CARTESIAN_POINT ( 'NONE',  ( -12.52947101616301673, -4.316762297166332196, -19.39321520033831803 ) ) ;
#8802 = DIRECTION ( 'NONE',  ( 0.000000000000000000, 0.000000000000000000, 1.000000000000000000 ) ) ;
#8803 = CARTESIAN_POINT ( 'NONE',  ( 122.9503348109119827, 0.5811942927096110934, -14.16772938898807510 ) ) ;
#8804 = CARTESIAN_POINT ( 'NONE',  ( 118.0718414775786300, -9.261995988541697145, -16.69588392320189030 ) ) ;
#8805 = CARTESIAN_POINT ( 'NONE',  ( 105.4819421295248247, 0.8980012041604618078, -13.39321520033831447 ) ) ;
#8806 = CARTESIAN_POINT ( 'NONE',  ( 115.2922348109119781, -10.63000616557722466, -14.87417383870573495 ) ) ;
#8807 = CARTESIAN_POINT ( 'NONE',  ( 71.02242295334774269, -99.02728775972636299, -55.91838671430374319 ) ) ;
#8808 = EDGE_LOOP ( 'NONE', ( #3050, #23553, #36226, #44641, #43126 ) ) ;
#8809 = CARTESIAN_POINT ( 'NONE',  ( 128.2184548109119930, -4.863998795839242995, -13.39321520033831447 ) ) ;
#8810 = B_SPLINE_CURVE_WITH_KNOTS ( 'NONE', 3,
 ( #30091, #39676, #22122, #2033, #23017, #19596, #36015, #43549 ),
 .UNSPECIFIED., .F., .F.,
 ( 4, 2, 2, 4 ),
 ( 0.000000000000000000, 0.2500000000000005551, 0.5000000000000011102, 1.000000000000000000 ),
 .UNSPECIFIED. ) ;
#8811 = CARTESIAN_POINT ( 'NONE',  ( 123.2339681442453241, -6.344957434206665248, -7.627207830600338134 ) ) ;
#8812 = AXIS2_PLACEMENT_3D ( 'NONE', #20983, #13919, #21202 ) ;
#8813 = CARTESIAN_POINT ( 'NONE',  ( 121.1918081442452859, 0.9020085738987339008, -11.91225656197089222 ) ) ;
#8814 = CARTESIAN_POINT ( 'NONE',  ( 126.2404814775786264, -0.8288870151387760510, -10.36305467784173118 ) ) ;
#8815 = VECTOR ( 'NONE', #8913, 1000.000000000000114 ) ;
#8816 = CARTESIAN_POINT ( 'NONE',  ( 114.3278814775786429, 0.1319031606808879209, -14.10382304977623669 ) ) ;
#8817 = CARTESIAN_POINT ( 'NONE',  ( 126.1270281442452870, -10.30919188438810075, -12.61870101168855918 ) ) ;
#8818 = CARTESIAN_POINT ( 'NONE',  ( 108.7462390045248242, 0.8980012041604421569, -15.77991374673208469 ) ) ;
#8819 = CARTESIAN_POINT ( 'NONE',  ( 118.5256548109119876, -8.899110576539710493, -16.42337572283490132 ) ) ;
#8820 = CARTESIAN_POINT ( 'NONE',  ( 116.7739797030027376, -3.961280311787784836, -18.49561454135252703 ) ) ;
#8821 = CARTESIAN_POINT ( 'NONE',  ( 115.9693640045247776, -10.62599879583958717, -11.00651665394454604 ) ) ;
#8822 = ORIENTED_EDGE ( 'NONE', *, *, #38675, .T. ) ;
#8823 = CARTESIAN_POINT ( 'NONE',  ( 121.4797829359119987, -5.367793381288652910, -18.78638297431638904 ) ) ;
#8824 = CARTESIAN_POINT ( 'NONE',  ( 124.0281414775786146, -1.834011780172310813, -8.268836392978581529 ) ) ;
#8825 = CARTESIAN_POINT ( 'NONE',  ( 122.1863582044368286, -6.247802574075781656, -18.73351920797576042 ) ) ;
#8826 = CARTESIAN_POINT ( 'NONE',  ( 125.0532895624266416, 2.567537813723679285, -12.20844840518084240 ) ) ;
#8827 = AXIS2_PLACEMENT_3D ( 'NONE', #6259, #20403, #41157 ) ;
#8828 = DIRECTION ( 'NONE',  ( 0.000000000000000000, 0.000000000000000000, 1.000000000000000000 ) ) ;
#8829 = CARTESIAN_POINT ( 'NONE',  ( 117.6180281442453150, -8.899110576539710493, -16.42337572283490132 ) ) ;
#8830 = CARTESIAN_POINT ( 'NONE',  ( 66.16515534780279495, -0.1171416179790299994, -16.39321520033831803 ) ) ;
#8831 = DIRECTION ( 'NONE',  ( 0.000000000000000000, 0.000000000000000000, -1.000000000000000000 ) ) ;
#8832 = CARTESIAN_POINT ( 'NONE',  ( 124.1415948109119540, -3.505236298600246325, -18.68346056562440793 ) ) ;
#8833 = ADVANCED_FACE ( 'NONE', ( #8407 ), #22984, .T. ) ;
#8834 = CARTESIAN_POINT ( 'NONE',  ( 123.7637130757767352, -0.9924539043446216624, -17.29976612834909133 ) ) ;
#8835 = DIRECTION ( 'NONE',  ( 0.000000000000000000, -0.9284778069183722282, -0.3713878862591645791 ) ) ;
#8836 = AXIS2_PLACEMENT_3D ( 'NONE', #8238, #39244, #26240 ) ;
#8837 = CARTESIAN_POINT ( 'NONE',  ( 124.5763124458833317, -11.88415338737963367, -16.94877137765329422 ) ) ;
#8838 = CARTESIAN_POINT ( 'NONE',  ( 123.4041481442452834, -10.30919188438810075, -12.61870101168855918 ) ) ;
#8839 = CARTESIAN_POINT ( 'NONE',  ( 117.6747548109119919, -7.643976991954077427, -18.09477374809248928 ) ) ;
#8840 = CARTESIAN_POINT ( 'NONE',  ( 121.3619881442452879, -5.574606645277164318, -18.38911715685844683 ) ) ;
#8841 = ORIENTED_EDGE ( 'NONE', *, *, #8880, .T. ) ;
#8842 = CARTESIAN_POINT ( 'NONE',  ( 124.5954081442453116, -3.383040157471821630, -19.15922257007629170 ) ) ;
#8843 = CARTESIAN_POINT ( 'NONE',  ( 114.1577014775786552, -6.344957434206662583, -7.627207830600332805 ) ) ;
#8844 = CARTESIAN_POINT ( 'NONE',  ( 115.3442858795247759, -8.402594152722688392, -9.854619843455216355 ) ) ;
#8845 = CARTESIAN_POINT ( 'NONE',  ( -7.923679509334008664, -5.078949698970065540, -8.893215200338314474 ) ) ;
#8846 = CARTESIAN_POINT ( 'NONE',  ( 123.6310548109119765, -4.153390946401325223, -8.397313243818185668 ) ) ;
#8847 = CARTESIAN_POINT ( 'NONE',  ( 122.5532481442453019, -10.63000616557722466, -14.87417383870573495 ) ) ;
#8848 = CARTESIAN_POINT ( 'NONE',  ( 113.1217858795247935, -0.7896495226426338832, -17.46756447353520159 ) ) ;
#8849 = CARTESIAN_POINT ( 'NONE',  ( 107.3571765045248299, -2.791137627527939813, -8.388885654883777576 ) ) ;
#8850 = DIRECTION ( 'NONE',  ( 1.000000000000000000, 0.000000000000000000, -0.000000000000000000 ) ) ;
#8851 = CARTESIAN_POINT ( 'NONE',  ( 86.34560043013698305, -9.320000780048239619, -18.64321520033831803 ) ) ;
#8852 = CARTESIAN_POINT ( 'NONE',  ( 122.4767535264548854, -8.247323210606174015, -17.08054893949881858 ) ) ;
#8853 = CARTESIAN_POINT ( 'NONE',  ( 113.1912390045248031, -9.868328341294098749, -11.32035403202665869 ) ) ;
#8854 = VERTEX_POINT ( 'NONE', #29149 ) ;
#8855 = CARTESIAN_POINT ( 'NONE',  ( 123.6310548109119765, -4.153390946401325223, -8.397313243818185668 ) ) ;
#8856 = CARTESIAN_POINT ( 'NONE',  ( 122.8688454359119646, -11.07370829466463569, -12.81314460846529002 ) ) ;
#8857 = CARTESIAN_POINT ( 'NONE',  ( 120.7157985609119635, -10.36940331770106916, -15.09355782777062061 ) ) ;
#8858 = DIRECTION ( 'NONE',  ( -0.2768435750659239414, -0.3568721902840664151, 0.8921882507333142032 ) ) ;
#8859 = CARTESIAN_POINT ( 'NONE',  ( 106.5931921295248372, -9.868328341294093420, -13.39321520033831447 ) ) ;
#8860 = EDGE_CURVE ( 'NONE', #35546, #5970, #28275, .T. ) ;
#8861 = ORIENTED_EDGE ( 'NONE', *, *, #23681, .F. ) ;
#8862 = CARTESIAN_POINT ( 'NONE',  ( 119.8303681442453126, -10.63000616557722466, -14.87417383870573495 ) ) ;
#8863 = CARTESIAN_POINT ( 'NONE',  ( 113.0231681442453322, 0.9020085738987376756, -11.91225656197089755 ) ) ;
#8864 = AXIS2_PLACEMENT_3D ( 'NONE', #44728, #10074, #10289 ) ;
#8865 = CARTESIAN_POINT ( 'NONE',  ( 123.0637881442452937, -8.899110576539710493, -16.42337572283490132 ) ) ;
#8866 = CARTESIAN_POINT ( 'NONE',  ( 115.7460481442453357, -10.15424416112533912, -14.75197769757731336 ) ) ;
#8867 =( LENGTH_UNIT ( ) NAMED_UNIT ( * ) SI_UNIT ( .MILLI., .METRE. ) );
#8868 = FACE_OUTER_BOUND ( 'NONE', #38724, .T. ) ;
#8869 = CARTESIAN_POINT ( 'NONE',  ( 88.22708560785949317, -3.622631779710408395, -18.64321520033831803 ) ) ;
#8870 = EDGE_CURVE ( 'NONE', #2680, #5955, #10796, .T. ) ;
#8871 = CARTESIAN_POINT ( 'NONE',  ( 113.5337081442453240, -9.261995988541697145, -16.69588392320189030 ) ) ;
#8872 = ADVANCED_FACE ( 'NONE', ( #11829 ), #17390, .T. ) ;
#8873 = CARTESIAN_POINT ( 'NONE',  ( 113.9552233795247815, -1.325403438956436419, -9.854619843455211026 ) ) ;
#8874 = CONICAL_SURFACE ( 'NONE', #28540, 2.000000000000000444, 0.9599310885968830309 ) ;
#8875 = CARTESIAN_POINT ( 'NONE',  ( 122.4965214775786251, -10.30919188438810075, -12.61870101168855918 ) ) ;
#8876 = DIRECTION ( 'NONE',  ( -0.000000000000000000, -0.9284778069183721172, -0.3713878862591650232 ) ) ;
#8877 = EDGE_LOOP ( 'NONE', ( #20314, #22437, #2024, #21245 ) ) ;
#8878 = CARTESIAN_POINT ( 'NONE',  ( 114.6115148109119986, -3.383040157471821630, -19.15922257007629170 ) ) ;
#8879 = CARTESIAN_POINT ( 'NONE',  ( 112.9097148109120070, -9.565557343593413364, -10.61323700422348004 ) ) ;
#8880 = EDGE_CURVE ( 'NONE', #32564, #29158, #23543, .T. ) ;
#8881 = DIRECTION ( 'NONE',  ( 0.000000000000000000, 0.000000000000000000, -1.000000000000000000 ) ) ;
#8882 = CARTESIAN_POINT ( 'NONE',  ( 126.4673881442452910, -7.894159318335828068, -9.358103419637847864 ) ) ;
#8883 = VERTEX_POINT ( 'NONE', #35530 ) ;
#8884 = CARTESIAN_POINT ( 'NONE',  ( 122.5532481442453019, -10.63000616557722466, -14.87417383870573495 ) ) ;
#8885 = FACE_OUTER_BOUND ( 'NONE', #13769, .T. ) ;
#8886 = DIRECTION ( 'NONE',  ( 0.9609149988134837450, -0.1028163501681639419, 0.2570431154366518145 ) ) ;
#8887 = ADVANCED_FACE ( 'NONE', ( #42849 ), #18224, .F. ) ;
#8888 = CARTESIAN_POINT ( 'NONE',  ( 115.1552801496069947, 0.3591747506842615789, -14.64321520033831447 ) ) ;
#8889 = EDGE_CURVE ( 'NONE', #2587, #22394, #10936, .T. ) ;
#8890 = EDGE_CURVE ( 'NONE', #6245, #35524, #35984, .T. ) ;
#8891 = CARTESIAN_POINT ( 'NONE',  ( 123.4944583641427727, -4.097270811097695642, -15.66323126201896798 ) ) ;
#8892 = CARTESIAN_POINT ( 'NONE',  ( 115.2355081442453155, 0.1319031606808879209, -14.10382304977623669 ) ) ;
#8893 = CARTESIAN_POINT ( 'NONE',  ( 86.84969988883354119, -8.456355172323730685, -8.143215200338314474 ) ) ;
#8894 = AXIS2_PLACEMENT_3D ( 'NONE', #13925, #24855, #20326 ) ;
#8895 = CARTESIAN_POINT ( 'NONE',  ( 125.1416936109526716, -1.781206261049963491, -20.14521123147079606 ) ) ;
#8896 = CARTESIAN_POINT ( 'NONE',  ( 112.2857214775786474, -5.574606645277164318, -18.38911715685844683 ) ) ;
#8897 = CARTESIAN_POINT ( 'NONE',  ( 125.3328548109119964, -0.8288870151387760510, -10.36305467784173118 ) ) ;
#8898 = CARTESIAN_POINT ( 'NONE',  ( 122.5910329359119970, -5.367793381288652910, -18.78638297431638904 ) ) ;
#8899 = CARTESIAN_POINT ( 'NONE',  ( 113.5337081442453240, -9.261995988541697145, -16.69588392320189030 ) ) ;
#8900 = CARTESIAN_POINT ( 'NONE',  ( 115.9162281442453235, -5.574606645277164318, -18.38911715685844683 ) ) ;
#8901 = CARTESIAN_POINT ( 'NONE',  ( 123.6310548109119765, -5.638512984488999180, -18.83840828888717311 ) ) ;
#8902 = CARTESIAN_POINT ( 'NONE',  ( 121.0783548109119749, 0.2603800115204892296, -16.42320221600525088 ) ) ;
#8903 = ORIENTED_EDGE ( 'NONE', *, *, #35051, .F. ) ;
#8904 = CARTESIAN_POINT ( 'NONE',  ( 126.6827570900509130, -8.513103522651428889, -17.14294544241743523 ) ) ;
#8905 = CARTESIAN_POINT ( 'NONE',  ( 110.4131140045248287, -10.62599879583958717, -11.00651665394454604 ) ) ;
#8906 = CARTESIAN_POINT ( 'NONE',  ( 109.3018640045248304, 0.1403307496149616695, -15.46607636864997204 ) ) ;
#8907 = VECTOR ( 'NONE', #35747, 1000.000000000000000 ) ;
#8908 = CARTESIAN_POINT ( 'NONE',  ( 108.9545983795247821, -8.402594152722688392, -16.93181055722141792 ) ) ;
#8909 = CARTESIAN_POINT ( 'NONE',  ( 126.2275303246277502, -9.801060169199397265, -12.57365908077032124 ) ) ;
#8910 = CARTESIAN_POINT ( 'NONE',  ( 116.3700414775786527, -5.638512984488999180, -18.83840828888717311 ) ) ;
#8911 = ORIENTED_EDGE ( 'NONE', *, *, #28125, .F. ) ;
#8912 = CARTESIAN_POINT ( 'NONE',  ( 125.4584548109119737, -8.963735245270648022, -18.43723750849711962 ) ) ;
#8913 = DIRECTION ( 'NONE',  ( -0.9609149988134834119, 0.1028163501681648995, -0.2570431154366529802 ) ) ;
#8914 = DIRECTION ( 'NONE',  ( 1.000000000000000000, 0.000000000000000000, 0.000000000000000000 ) ) ;
#8915 = CARTESIAN_POINT ( 'NONE',  ( 113.9875214775786532, -8.899110576539710493, -16.42337572283490132 ) ) ;
#8916 = CARTESIAN_POINT ( 'NONE',  ( 121.3052614775786111, -1.834011780172310813, -8.268836392978581529 ) ) ;
#8917 = CARTESIAN_POINT ( 'NONE',  ( 111.1770983795247787, -0.7896495226426338832, -9.318865927141430916 ) ) ;
#8918 = CARTESIAN_POINT ( 'NONE',  ( 94.20708369096698220, -27.10035099198479358, -13.29271931396930739 ) ) ;
#8919 = VERTEX_POINT ( 'NONE', #4533 ) ;
#8920 = DIRECTION ( 'NONE',  ( 0.000000000000000000, 0.000000000000000000, 1.000000000000000000 ) ) ;
#8921 = CARTESIAN_POINT ( 'NONE',  ( 118.8660148109119774, 0.1319031606808879209, -14.10382304977623669 ) ) ;
#8922 = CARTESIAN_POINT ( 'NONE',  ( 119.2631014775786298, 0.2603800115204892296, -16.42320221600525088 ) ) ;
#8923 = CARTESIAN_POINT ( 'NONE',  ( 112.3424481442453384, -3.505236298600246325, -18.68346056562440793 ) ) ;
#8924 = CARTESIAN_POINT ( 'NONE',  ( 114.6682414775786469, -1.561330072975668060, -17.79121239304076596 ) ) ;
#8925 = DIRECTION ( 'NONE',  ( 1.000000000000000000, 0.000000000000000000, -0.000000000000000000 ) ) ;
#8926 = CARTESIAN_POINT ( 'NONE',  ( 124.0848681442452772, -5.574606645277164318, -18.38911715685844683 ) ) ;
#8927 = CARTESIAN_POINT ( 'NONE',  ( 121.0216281442452981, -7.894159318335828068, -9.358103419637847864 ) ) ;
#8928 = ORIENTED_EDGE ( 'NONE', *, *, #41494, .F. ) ;
#8929 = AXIS2_PLACEMENT_3D ( 'NONE', #19131, #18901, #5438 ) ;
#8930 = CARTESIAN_POINT ( 'NONE',  ( 123.1466579359119891, -5.444069387712269226, -19.60292469916370450 ) ) ;
#8931 = AXIS2_PLACEMENT_3D ( 'NONE', #42108, #27979, #10869 ) ;
#8932 = CARTESIAN_POINT ( 'NONE',  ( 113.9307948109119906, 0.9020085738987339008, -11.91225656197089222 ) ) ;
#8933 = CARTESIAN_POINT ( 'NONE',  ( 120.1707281442453166, -9.565557343593413364, -10.61323700422348004 ) ) ;
#8934 = ORIENTED_EDGE ( 'NONE', *, *, #6666, .F. ) ;
#8935 = CARTESIAN_POINT ( 'NONE',  ( 124.2579079359120016, -4.360204210389833968, -8.000047426360245240 ) ) ;
#8936 = CARTESIAN_POINT ( 'NONE',  ( 119.1496481442453046, -3.383040157471821630, -19.15922257007629170 ) ) ;
#8937 = PRESENTATION_LAYER_ASSIGNMENT (  '', '', ( #19877 ) ) ;
#8938 = CARTESIAN_POINT ( 'NONE',  ( 113.5385046295247804, -4.863998795839590272, -7.631215200338315796 ) ) ;
#8939 = CARTESIAN_POINT ( 'NONE',  ( 116.9940348109119839, -0.1624402480850797581, -16.17319339645315424 ) ) ;
#8940 = ADVANCED_FACE ( 'NONE', ( #32346 ), #11609, .T. ) ;
#8941 = EDGE_LOOP ( 'NONE', ( #5331, #1108, #28713, #36956 ) ) ;
#8942 = VECTOR ( 'NONE', #36676, 1000.000000000000000 ) ;
#8943 = VERTEX_POINT ( 'NONE', #39423 ) ;
#8944 = CARTESIAN_POINT ( 'NONE',  ( 123.8012348109119642, -9.565557343593413364, -10.61323700422348004 ) ) ;
#8945 = CARTESIAN_POINT ( 'NONE',  ( 120.1707281442453166, -9.565557343593413364, -10.61323700422348004 ) ) ;
#8946 = CARTESIAN_POINT ( 'NONE',  ( 83.83554121260367253, -27.84333996136784961, -14.15691383771150136 ) ) ;
#8947 = EDGE_CURVE ( 'NONE', #33232, #13961, #7501, .T. ) ;
#8948 = CARTESIAN_POINT ( 'NONE',  ( 62.22678445075433018, -36.72958069525633817, -5.531797115907686191 ) ) ;
#8949 = CARTESIAN_POINT ( 'NONE',  ( 61.79762598887304392, -65.86410496095400902, -43.61203885794885338 ) ) ;
#8950 = CARTESIAN_POINT ( 'NONE',  ( 117.7882081442453170, -6.344957434206665248, -7.627207830600338134 ) ) ;
#8951 = CYLINDRICAL_SURFACE ( 'NONE', #28449, 3.000000000000001776 ) ;
#8952 = EDGE_CURVE ( 'NONE', #40373, #29623, #14128, .T. ) ;
#8953 = CARTESIAN_POINT ( 'NONE',  ( 117.4478481442453131, 0.2603800115204892296, -16.42320221600525088 ) ) ;
#8955 = CARTESIAN_POINT ( 'NONE',  ( 114.8384214775786489, -10.15424416112533912, -14.75197769757731336 ) ) ;
#8954 = CARTESIAN_POINT ( 'NONE',  ( 114.2144281442453178, -8.166667518702817929, -8.995218007635859436 ) ) ;
#8956 = EDGE_CURVE ( 'NONE', #38354, #25316, #6596, .T. ) ;
#8957 = CARTESIAN_POINT ( 'NONE',  ( 121.8725281442453223, -6.222761293078241884, -8.102969835052219238 ) ) ;
#8958 = EDGE_LOOP ( 'NONE', ( #31828, #3939, #14652, #11833 ) ) ;
#8959 = CARTESIAN_POINT ( 'NONE',  ( 120.4543614775786295, -5.574606645277164318, -18.38911715685844683 ) ) ;
#8960 = CIRCLE ( 'NONE', #31534, 2.999999999999999556 ) ;
#8961 = DIRECTION ( 'NONE',  ( -0.000000000000000000, -0.9284778069183718952, -0.3713878862591649677 ) ) ;
#8962 = CARTESIAN_POINT ( 'NONE',  ( 114.5803015045248117, -2.477300249445798297, -7.631215200338321125 ) ) ;
#8963 = CARTESIAN_POINT ( 'NONE',  ( 70.86891319097370001, -49.31949126737637812, -35.46156944284200563 ) ) ;
#8964 = CARTESIAN_POINT ( 'NONE',  ( 112.7745202545247878, -10.62599879583958717, -15.77991374673208469 ) ) ;
#8965 = CARTESIAN_POINT ( 'NONE',  ( 119.1496481442453046, -3.383040157471821630, -19.15922257007629170 ) ) ;
#8966 = ORIENTED_EDGE ( 'NONE', *, *, #31267, .T. ) ;
#8967 = CARTESIAN_POINT ( 'NONE',  ( 120.3409081442453044, -0.4660016031367893996, -10.09054647747474043 ) ) ;
#8968 = CARTESIAN_POINT ( 'NONE',  ( 63.34631942287607842, -37.83243761108621328, -4.915970705112973960 ) ) ;
#8969 = CARTESIAN_POINT ( 'NONE',  ( 107.2182702545248105, -10.62599879583958717, -15.77991374673208469 ) ) ;
#8970 = CARTESIAN_POINT ( 'NONE',  ( 118.7525614775786380, -8.166667518702819706, -8.995218007635861213 ) ) ;
#8971 = CARTESIAN_POINT ( 'NONE',  ( 118.0718414775786300, -9.261995988541697145, -16.69588392320189030 ) ) ;
#8972 = CARTESIAN_POINT ( 'NONE',  ( 73.07463722459043254, -59.21746703140907897, -35.99528165304237604 ) ) ;
#8973 = DIRECTION ( 'NONE',  ( 0.000000000000000000, 0.000000000000000000, 1.000000000000000000 ) ) ;
#8974 = ORIENTED_EDGE ( 'NONE', *, *, #25111, .T. ) ;
#8975 = CONICAL_SURFACE ( 'NONE', #34406, 1.610000000000000986, 0.9599310885968765916 ) ;
#8976 = CARTESIAN_POINT ( 'NONE',  ( 115.5950730757767531, -0.9924539043446216624, -17.29976612834909133 ) ) ;
#8977 = CARTESIAN_POINT ( 'NONE',  ( 109.2295516025745030, -10.43151013607753974, -13.43516445080127752 ) ) ;
#8978 = CARTESIAN_POINT ( 'NONE',  ( 120.1707281442453166, -9.565557343593413364, -10.61323700422348004 ) ) ;
#8979 = CARTESIAN_POINT ( 'NONE',  ( 110.8298327545248299, -6.936859964151250502, -8.388885654883777576 ) ) ;
#8980 = CARTESIAN_POINT ( 'NONE',  ( 110.8992858795247827, -8.402594152722688392, -9.854619843455216355 ) ) ;
#8981 = CARTESIAN_POINT ( 'NONE',  ( 119.4900081442453086, -7.643976991954077427, -18.09477374809248928 ) ) ;
#8982 = DIRECTION ( 'NONE',  ( -0.1352586133457981954, -0.9908103287288499983, 0.000000000000000000 ) ) ;
#8983 = CARTESIAN_POINT ( 'NONE',  ( 70.83207129814674374, -26.36080320520898823, -5.469311635450105236 ) ) ;
#8984 = CARTESIAN_POINT ( 'NONE',  ( 113.9875214775786532, -8.899110576539710493, -16.42337572283490132 ) ) ;
#8985 = CARTESIAN_POINT ( 'NONE',  ( 122.4965214775786251, -10.30919188438810075, -12.61870101168855918 ) ) ;
#8986 = EDGE_LOOP ( 'NONE', ( #32423, #41248, #12929, #34150, #42729 ) ) ;
#8987 = CARTESIAN_POINT ( 'NONE',  ( 121.5888948109119809, 0.1319031606808879209, -14.10382304977623669 ) ) ;
#8988 = CARTESIAN_POINT ( 'NONE',  ( 115.6893214775786447, 0.5811942927096154232, -14.16772938898807155 ) ) ;
#8989 = CARTESIAN_POINT ( 'NONE',  ( 121.9859814775786333, 0.2603800115204892296, -16.42320221600525088 ) ) ;
#8990 = CARTESIAN_POINT ( 'NONE',  ( 123.1205148109119563, -7.643976991954077427, -18.09477374809248928 ) ) ;
#8991 = ORIENTED_EDGE ( 'NONE', *, *, #33478, .F. ) ;
#8992 = CARTESIAN_POINT ( 'NONE',  ( 123.8579614775786126, -9.859900752359378018, -12.68260735090039759 ) ) ;
#8993 =( BOUNDED_SURFACE ( )  B_SPLINE_SURFACE ( 1, 2, ( 
 ( #19658, #33545, #9400, #43610, #13057, #26956, #2550, #40878, #40421, #16708, #40645, #16479, #6445, #20127, #34014, #30602, #9868, #5516, #20353, #2095, #44302, #2783, #16021, #44519, #23777, #15796, #27190, #29698, #12385, #37669, #26283, #40191, #12610, #22857, #19436, #29929, #9180, #43843, #26513, #36968, #2324, #16252, #30155, #26737, #23311, #14167, #28085, #41774, #10976, #10758, #13952, #13733, #38541, #17595, #7102, #27643, #21236, #39, #24655, #17377, #41993, #17815, #3895, #34674, #6884, #10098, #6665, #3460, #31709, #31489, #20575, #24002, #10534, #27864, #24434, #35114, #41557, #37889, #7316, #31046, #3011, #21012, #41339, #38325, #34886, #258, #479, #42216, #14392, #34452, #31265, #3674, #3233, #27419, #24218, #38109, #28304, #24880, #17159, #38772, #7542, #34237, #16933, #44752, #30829, #13511, #44976, #10316, #20794, #7776, #4794, #4570, #22133, #35798, #39911, #29195, #5017, #21459, #18935, #18264, #35342, #1375, #42887, #12103, #14617, #26007, #4114, #28534, #18036, #18494, #32822, #8227, #11648, #11877, #36250, #32384, #43107, #21904, #1592, #39231, #25338, #32160, #39688, #39463, #18715, #29420, #36026, #25557, #31932, #15288, #22356, #28757, #697, #11433, #15513, #42440, #11205, #15068, #928, #25781, #8453, #43334, #1151, #25109, #32606, #39006, #21683, #7996, #35571, #4344, #14847, #28981, #42662, #16426, #37382, #23030, #30101, #27133, #19160, #23261, #43559, #29645, #26227, #40136, #36693, #26460, #2497, #23496, #6152, #22575, #44017, #20072, #22799, #33958, #36917, #43788, #2725, #5688, #12328, #12779, #37144, #36477, #30322, #2269, #26681, #16197, #30546, #13232, #5463, #15970, #8901, #40592, #44248, #19383, #13006, #16651, #8672, #26905, #5244, #33041, #44467, #1816, #19840, #33271, #15743, #2046, #9351, #29873, #12553, #40362, #9126, #19607, #33491, #5918, #33727, #40825, #9580, #21572, #4006, #18385, #18152, #20740, #20520, #815, #24993, #14507, #34400, #28646, #6835, #32047, #24165, #4234, #25224, #11314, #41502, #13679, #16882 ),
 ( #14734, #42552, #44922, #39122, #7889, #13459, #30996, #27588, #21795, #35689, #10258, #17928, #14957, #6387, #11092, #30773, #44699, #27362, #41282, #23949, #38057, #35459, #4464, #32273, #9814, #31827, #1041, #10042, #41057, #34620, #597, #23723, #28420, #37830, #42331, #38888, #37613, #20295, #7657, #34180, #2955, #6607, #3181, #17105, #25450, #42782, #8120, #22021, #35915, #18602, #1268, #4681, #11543, #32493, #28869, #39352, #19828, #16642, #30535, #23713, #37604, #16413, #44688, #27354, #41273, #23939, #37132, #13449, #20513, #16873, #37820, #2944, #12997, #10033, #40582, #6597, #9341, #9569, #10250, #41492, #30311, #6376, #31206, #17317, #9804, #2716, #34392, #38049, #26893, #20286, #40813, #6827, #3174, #24158, #34612, #33716, #44237, #34170, #2487, #23484, #20732, #37371, #6142, #30763, #17096, #20063, #30989, #44914, #13671, #27579, #3399, #33946, #45128, #26669, #23250, #5908, #13223, #44457, #27122, #41047, #18197, #25271, #31645, #414, #21392, #10474, #25041, #38935, #4049, #7704, #7254, #28695, #7473, #28470, #18433, #32092, #21618, #42599, #21842, #3609, #32324, #14106, #31873, #35507, #189, #4279, #7932, #13886, #863, #41709, #27796, #11362, #24375, #14780, #24596, #20954, #38261, #638, #21169, #7042, #28022, #35737, #35045, #34826, #17525, #31423, #38706, #39168, #4510, #35274, #41929, #10693, #17972, #38480, #3826, #42376, #14551, #17749, #14331, #24814, #28245, #42154, #10914, #11138, #15910, #1532, #18868, #22071, #18651, #15454, #29808, #43500, #32543, #35963, #22512, #39849, #36406, #1983, #25719, #4733, #22733, #43044, #36633, #1313, #40067, #40299, #5624, #5407, #28916, #1089, #43723, #19546, #12268, #11812, #8165, #15003, #19094, #8389, #11587, #15225, #9063, #39626, #42826, #25496, #29132, #25942, #26164, #8832, #8614, #22964, #19323, #5176, #22294, #33208, #29583, #32979, #36188, #12491, #12039, #26389, #29359, #36855, #39400, #4954, #43273, #32759, #1755, #15679, #22727, #25713, #4272, #1307, #18191, #8381, #8606, #39843, #8159 ) ),
 .UNSPECIFIED., .F., .F., .T. ) 
 B_SPLINE_SURFACE_WITH_KNOTS ( ( 2, 2 ),
 ( 3, 2, 2, 2, 2, 2, 2, 2, 2, 2, 2, 2, 2, 2, 2, 2, 2, 2, 2, 2, 2, 2, 2, 2, 2, 2, 2, 2, 2, 2, 2, 2, 2, 2, 2, 2, 2, 2, 2, 2, 2, 2, 2, 2, 2, 2, 2, 2, 2, 2, 2, 2, 2, 2, 2, 2, 2, 2, 2, 2, 2, 2, 2, 2, 2, 2, 2, 2, 2, 2, 2, 2, 2, 2, 2, 2, 2, 2, 2, 2, 2, 2, 2, 2, 2, 2, 2, 2, 2, 2, 2, 2, 2, 2, 2, 2, 2, 2, 2, 2, 2, 2, 2, 2, 2, 2, 2, 2, 2, 2, 2, 2, 2, 2, 2, 2, 2, 2, 2, 2, 2, 2, 2, 2, 2, 2, 2, 2, 3 ),
 ( 0.000000000000000000, 1.000000000000000000 ),
 ( 0.000000000000000000, 0.007812500000000000000, 0.01562500000000000000, 0.02343750000000000000, 0.03125000000000000000, 0.03906250000000000000, 0.04687500000000000000, 0.05468750000000000000, 0.06250000000000000000, 0.07031250000000000000, 0.07812500000000000000, 0.08593750000000000000, 0.09375000000000000000, 0.1015625000000000000, 0.1093750000000000000, 0.1171875000000000000, 0.1250000000000000000, 0.1328125000000000000, 0.1406250000000000000, 0.1484375000000000000, 0.1562500000000000000, 0.1640625000000000000, 0.1718750000000000000, 0.1796875000000000000, 0.1875000000000000000, 0.1953125000000000000, 0.2031250000000000000, 0.2109375000000000000, 0.2187500000000000000, 0.2265625000000000000, 0.2343750000000000000, 0.2421875000000000000, 0.2500000000000000000, 0.2578125000000000000, 0.2656250000000000000, 0.2734375000000000000, 0.2812500000000000000, 0.2890625000000000000, 0.2968750000000000000, 0.3046875000000000000, 0.3125000000000000000, 0.3203125000000000000, 0.3281250000000000000, 0.3359375000000000000, 0.3437500000000000000, 0.3515625000000000000, 0.3593750000000000000, 0.3671875000000000000, 0.3750000000000000000, 0.3828125000000000000, 0.3906250000000000000, 0.3984375000000000000, 0.4062500000000000000, 0.4140625000000000000, 0.4218750000000000000, 0.4296875000000000000, 0.4375000000000000000, 0.4453125000000000000, 0.4531250000000000000, 0.4609375000000000000, 0.4687500000000000000, 0.4765625000000000000, 0.4843750000000000000, 0.4921875000000000000, 0.5000000000000000000, 0.5078125000000000000, 0.5156250000000000000, 0.5234375000000000000, 0.5312500000000000000, 0.5390625000000000000, 0.5468750000000000000, 0.5546875000000000000, 0.5625000000000000000, 0.5703125000000000000, 0.5781250000000000000, 0.5859375000000000000, 0.5937500000000000000, 0.6015625000000000000, 0.6093750000000000000, 0.6171875000000000000, 0.6250000000000000000, 0.6328125000000000000, 0.6406250000000000000, 0.6484375000000000000, 0.6562500000000000000, 0.6640625000000000000, 0.6718750000000000000, 0.6796875000000000000, 0.6875000000000000000, 0.6953125000000000000, 0.7031250000000000000, 0.7109375000000000000, 0.7187500000000000000, 0.7265625000000000000, 0.7343750000000000000, 0.7421875000000000000, 0.7500000000000000000, 0.7578125000000000000, 0.7656250000000000000, 0.7734375000000000000, 0.7812500000000000000, 0.7890625000000000000, 0.7968750000000000000, 0.8046875000000000000, 0.8125000000000000000, 0.8203125000000000000, 0.8281250000000000000, 0.8359375000000000000, 0.8437500000000000000, 0.8515625000000000000, 0.8593750000000000000, 0.8671875000000000000, 0.8750000000000000000, 0.8828125000000000000, 0.8906250000000000000, 0.8984375000000000000, 0.9062500000000000000, 0.9140625000000000000, 0.9218750000000000000, 0.9296875000000000000, 0.9375000000000000000, 0.9453125000000000000, 0.9531250000000000000, 0.9609375000000000000, 0.9687500000000000000, 0.9765625000000000000, 0.9843750000000000000, 0.9921875000000000000, 1.000000000000000000 ),
 .UNSPECIFIED. ) 
 GEOMETRIC_REPRESENTATION_ITEM ( )  RATIONAL_B_SPLINE_SURFACE ( (
 ( 1.000000000000000000, 0.9238795325112869605, 1.000000000000000000, 0.9238795325112869605, 1.000000000000000000, 0.9238795325112869605, 1.000000000000000000, 0.9238795325112869605, 1.000000000000000000, 0.9238795325112869605, 1.000000000000000000, 0.9238795325112869605, 1.000000000000000000, 0.9238795325112869605, 1.000000000000000000, 0.9238795325112869605, 1.000000000000000000, 0.9238795325112869605, 1.000000000000000000, 0.9238795325112869605, 1.000000000000000000, 0.9238795325112869605, 1.000000000000000000, 0.9238795325112869605, 1.000000000000000000, 0.9238795325112869605, 1.000000000000000000, 0.9238795325112869605, 1.000000000000000000, 0.9238795325112869605, 1.000000000000000000, 0.9238795325112869605, 1.000000000000000000, 0.9238795325112869605, 1.000000000000000000, 0.9238795325112869605, 1.000000000000000000, 0.9238795325112869605, 1.000000000000000000, 0.9238795325112869605, 1.000000000000000000, 0.9238795325112869605, 1.000000000000000000, 0.9238795325112869605, 1.000000000000000000, 0.9238795325112869605, 1.000000000000000000, 0.9238795325112869605, 1.000000000000000000, 0.9238795325112869605, 1.000000000000000000, 0.9238795325112869605, 1.000000000000000000, 0.9238795325112869605, 1.000000000000000000, 0.9238795325112869605, 1.000000000000000000, 0.9238795325112869605, 1.000000000000000000, 0.9238795325112869605, 1.000000000000000000, 0.9238795325112869605, 1.000000000000000000, 0.9238795325112869605, 1.000000000000000000, 0.9238795325112869605, 1.000000000000000000, 0.9238795325112869605, 1.000000000000000000, 0.9238795325112869605, 1.000000000000000000, 0.9238795325112869605, 1.000000000000000000, 0.9238795325112869605, 1.000000000000000000, 0.9238795325112869605, 1.000000000000000000, 0.9238795325112869605, 1.000000000000000000, 0.9238795325112869605, 1.000000000000000000, 0.9238795325112869605, 1.000000000000000000, 0.9238795325112869605, 1.000000000000000000, 0.9238795325112869605, 1.000000000000000000, 0.9238795325112869605, 1.000000000000000000, 0.9238795325112869605, 1.000000000000000000, 0.9238795325112869605, 1.000000000000000000, 0.9238795325112869605, 1.000000000000000000, 0.9238795325112869605, 1.000000000000000000, 0.9238795325112869605, 1.000000000000000000, 0.9238795325112869605, 1.000000000000000000, 0.9238795325112869605, 1.000000000000000000, 0.9238795325112869605, 1.000000000000000000, 0.9238795325112869605, 1.000000000000000000, 0.9238795325112869605, 1.000000000000000000, 0.9238795325112869605, 1.000000000000000000, 0.9238795325112869605, 1.000000000000000000, 0.9238795325112869605, 1.000000000000000000, 0.9238795325112869605, 1.000000000000000000, 0.9238795325112869605, 1.000000000000000000, 0.9238795325112869605, 1.000000000000000000, 0.9238795325112869605, 1.000000000000000000, 0.9238795325112869605, 1.000000000000000000, 0.9238795325112869605, 1.000000000000000000, 0.9238795325112869605, 1.000000000000000000, 0.9238795325112869605, 1.000000000000000000, 0.9238795325112869605, 1.000000000000000000, 0.9238795325112869605, 1.000000000000000000, 0.9238795325112869605, 1.000000000000000000, 0.9238795325112869605, 1.000000000000000000, 0.9238795325112869605, 1.000000000000000000, 0.9238795325112869605, 1.000000000000000000, 0.9238795325112869605, 1.000000000000000000, 0.9238795325112869605, 1.000000000000000000, 0.9238795325112869605, 1.000000000000000000, 0.9238795325112869605, 1.000000000000000000, 0.9238795325112869605, 1.000000000000000000, 0.9238795325112869605, 1.000000000000000000, 0.9238795325112869605, 1.000000000000000000, 0.9238795325112869605, 1.000000000000000000, 0.9238795325112869605, 1.000000000000000000, 0.9238795325112869605, 1.000000000000000000, 0.9238795325112869605, 1.000000000000000000, 0.9238795325112869605, 1.000000000000000000, 0.9238795325112869605, 1.000000000000000000, 0.9238795325112869605, 1.000000000000000000, 0.9238795325112869605, 1.000000000000000000, 0.9238795325112869605, 1.000000000000000000, 0.9238795325112869605, 1.000000000000000000, 0.9238795325112869605, 1.000000000000000000, 0.9238795325112869605, 1.000000000000000000, 0.9238795325112869605, 1.000000000000000000, 0.9238795325112869605, 1.000000000000000000, 0.9238795325112869605, 1.000000000000000000, 0.9238795325112869605, 1.000000000000000000, 0.9238795325112869605, 1.000000000000000000, 0.9238795325112869605, 1.000000000000000000, 0.9238795325112869605, 1.000000000000000000, 0.9238795325112869605, 1.000000000000000000, 0.9238795325112869605, 1.000000000000000000, 0.9238795325112869605, 1.000000000000000000, 0.9238795325112869605, 1.000000000000000000, 0.9238795325112869605, 1.000000000000000000, 0.9238795325112869605, 1.000000000000000000, 0.9238795325112869605, 1.000000000000000000, 0.9238795325112869605, 1.000000000000000000, 0.9238795325112869605, 1.000000000000000000, 0.9238795325112869605, 1.000000000000000000, 0.9238795325112869605, 1.000000000000000000, 0.9238795325112869605, 1.000000000000000000, 0.9238795325112869605, 1.000000000000000000, 0.9238795325112869605, 1.000000000000000000, 0.9238795325112869605, 1.000000000000000000, 0.9238795325112869605, 1.000000000000000000, 0.9238795325112869605, 1.000000000000000000, 0.9238795325112869605, 1.000000000000000000, 0.9238795325112869605, 1.000000000000000000, 0.9238795325112869605, 1.000000000000000000, 0.9238795325112869605, 1.000000000000000000, 0.9238795325112869605, 1.000000000000000000, 0.9238795325112869605, 1.000000000000000000, 0.9238795325112869605, 1.000000000000000000, 0.9238795325112869605, 1.000000000000000000, 0.9238795325112869605, 1.000000000000000000, 0.9238795325112869605, 1.000000000000000000, 0.9238795325112869605, 1.000000000000000000, 0.9238795325112869605, 1.000000000000000000, 0.9238795325112869605, 1.000000000000000000, 0.9238795325112869605, 1.000000000000000000),
 ( 1.000000000000000000, 0.9238795325112869605, 1.000000000000000000, 0.9238795325112869605, 1.000000000000000000, 0.9238795325112869605, 1.000000000000000000, 0.9238795325112869605, 1.000000000000000000, 0.9238795325112869605, 1.000000000000000000, 0.9238795325112869605, 1.000000000000000000, 0.9238795325112869605, 1.000000000000000000, 0.9238795325112869605, 1.000000000000000000, 0.9238795325112869605, 1.000000000000000000, 0.9238795325112869605, 1.000000000000000000, 0.9238795325112869605, 1.000000000000000000, 0.9238795325112869605, 1.000000000000000000, 0.9238795325112869605, 1.000000000000000000, 0.9238795325112869605, 1.000000000000000000, 0.9238795325112869605, 1.000000000000000000, 0.9238795325112869605, 1.000000000000000000, 0.9238795325112869605, 1.000000000000000000, 0.9238795325112869605, 1.000000000000000000, 0.9238795325112869605, 1.000000000000000000, 0.9238795325112869605, 1.000000000000000000, 0.9238795325112869605, 1.000000000000000000, 0.9238795325112869605, 1.000000000000000000, 0.9238795325112869605, 1.000000000000000000, 0.9238795325112869605, 1.000000000000000000, 0.9238795325112869605, 1.000000000000000000, 0.9238795325112869605, 1.000000000000000000, 0.9238795325112869605, 1.000000000000000000, 0.9238795325112869605, 1.000000000000000000, 0.9238795325112869605, 1.000000000000000000, 0.9238795325112869605, 1.000000000000000000, 0.9238795325112869605, 1.000000000000000000, 0.9238795325112869605, 1.000000000000000000, 0.9238795325112869605, 1.000000000000000000, 0.9238795325112869605, 1.000000000000000000, 0.9238795325112869605, 1.000000000000000000, 0.9238795325112869605, 1.000000000000000000, 0.9238795325112869605, 1.000000000000000000, 0.9238795325112869605, 1.000000000000000000, 0.9238795325112869605, 1.000000000000000000, 0.9238795325112869605, 1.000000000000000000, 0.9238795325112869605, 1.000000000000000000, 0.9238795325112869605, 1.000000000000000000, 0.9238795325112869605, 1.000000000000000000, 0.9238795325112869605, 1.000000000000000000, 0.9238795325112869605, 1.000000000000000000, 0.9238795325112869605, 1.000000000000000000, 0.9238795325112869605, 1.000000000000000000, 0.9238795325112869605, 1.000000000000000000, 0.9238795325112869605, 1.000000000000000000, 0.9238795325112869605, 1.000000000000000000, 0.9238795325112869605, 1.000000000000000000, 0.9238795325112869605, 1.000000000000000000, 0.9238795325112869605, 1.000000000000000000, 0.9238795325112869605, 1.000000000000000000, 0.9238795325112869605, 1.000000000000000000, 0.9238795325112869605, 1.000000000000000000, 0.9238795325112869605, 1.000000000000000000, 0.9238795325112869605, 1.000000000000000000, 0.9238795325112869605, 1.000000000000000000, 0.9238795325112869605, 1.000000000000000000, 0.9238795325112869605, 1.000000000000000000, 0.9238795325112869605, 1.000000000000000000, 0.9238795325112869605, 1.000000000000000000, 0.9238795325112869605, 1.000000000000000000, 0.9238795325112869605, 1.000000000000000000, 0.9238795325112869605, 1.000000000000000000, 0.9238795325112869605, 1.000000000000000000, 0.9238795325112869605, 1.000000000000000000, 0.9238795325112869605, 1.000000000000000000, 0.9238795325112869605, 1.000000000000000000, 0.9238795325112869605, 1.000000000000000000, 0.9238795325112869605, 1.000000000000000000, 0.9238795325112869605, 1.000000000000000000, 0.9238795325112869605, 1.000000000000000000, 0.9238795325112869605, 1.000000000000000000, 0.9238795325112869605, 1.000000000000000000, 0.9238795325112869605, 1.000000000000000000, 0.9238795325112869605, 1.000000000000000000, 0.9238795325112869605, 1.000000000000000000, 0.9238795325112869605, 1.000000000000000000, 0.9238795325112869605, 1.000000000000000000, 0.9238795325112869605, 1.000000000000000000, 0.9238795325112869605, 1.000000000000000000, 0.9238795325112869605, 1.000000000000000000, 0.9238795325112869605, 1.000000000000000000, 0.9238795325112869605, 1.000000000000000000, 0.9238795325112869605, 1.000000000000000000, 0.9238795325112869605, 1.000000000000000000, 0.9238795325112869605, 1.000000000000000000, 0.9238795325112869605, 1.000000000000000000, 0.9238795325112869605, 1.000000000000000000, 0.9238795325112869605, 1.000000000000000000, 0.9238795325112869605, 1.000000000000000000, 0.9238795325112869605, 1.000000000000000000, 0.9238795325112869605, 1.000000000000000000, 0.9238795325112869605, 1.000000000000000000, 0.9238795325112869605, 1.000000000000000000, 0.9238795325112869605, 1.000000000000000000, 0.9238795325112869605, 1.000000000000000000, 0.9238795325112869605, 1.000000000000000000, 0.9238795325112869605, 1.000000000000000000, 0.9238795325112869605, 1.000000000000000000, 0.9238795325112869605, 1.000000000000000000, 0.9238795325112869605, 1.000000000000000000, 0.9238795325112869605, 1.000000000000000000, 0.9238795325112869605, 1.000000000000000000, 0.9238795325112869605, 1.000000000000000000, 0.9238795325112869605, 1.000000000000000000, 0.9238795325112869605, 1.000000000000000000, 0.9238795325112869605, 1.000000000000000000, 0.9238795325112869605, 1.000000000000000000, 0.9238795325112869605, 1.000000000000000000, 0.9238795325112869605, 1.000000000000000000, 0.9238795325112869605, 1.000000000000000000, 0.9238795325112869605, 1.000000000000000000, 0.9238795325112869605, 1.000000000000000000, 0.9238795325112869605, 1.000000000000000000, 0.9238795325112869605, 1.000000000000000000, 0.9238795325112869605, 1.000000000000000000, 0.9238795325112869605, 1.000000000000000000, 0.9238795325112869605, 1.000000000000000000, 0.9238795325112869605, 1.000000000000000000, 0.9238795325112869605, 1.000000000000000000, 0.9238795325112869605, 1.000000000000000000, 0.9238795325112869605, 1.000000000000000000, 0.9238795325112869605, 1.000000000000000000, 0.9238795325112869605, 1.000000000000000000, 0.9238795325112869605, 1.000000000000000000) ) ) 
 REPRESENTATION_ITEM ( '' )  SURFACE ( )  );
#8994 = EDGE_CURVE ( 'NONE', #22341, #18093, #18842, .T. ) ;
#8995 = TOROIDAL_SURFACE ( 'NONE', #41777, 4.700000000000000178, 0.2999999999999999889 ) ;
#8996 = AXIS2_PLACEMENT_3D ( 'NONE', #34206, #40851, #30800 ) ;
#8997 = CARTESIAN_POINT ( 'NONE',  ( 124.0848681442452772, -4.089484607189486809, -7.948022111789456723 ) ) ;
#8998 = CARTESIAN_POINT ( 'NONE',  ( 125.3563494635840954, -7.185071377748551313, -6.737895779717858247 ) ) ;
#8999 = CARTESIAN_POINT ( 'NONE',  ( 125.9568481442452850, -6.344957434206665248, -7.627207830600338134 ) ) ;
#9000 = CARTESIAN_POINT ( 'NONE',  ( 107.4960827545248350, -2.477300249445798297, -19.15521520033831138 ) ) ;
#9001 = DIRECTION ( 'NONE',  ( 0.000000000000000000, 0.6004852223388322807, -0.7996358532186280677 ) ) ;
#9002 = CARTESIAN_POINT ( 'NONE',  ( 135.3184548109119874, -0.6896191363000483410, -17.70303589939592825 ) ) ;
#9003 = CARTESIAN_POINT ( 'NONE',  ( 108.8156921295247912, -9.868328341294093420, -13.39321520033831447 ) ) ;
#9004 = AXIS2_PLACEMENT_3D ( 'NONE', #4038, #39613, #22283 ) ;
#9005 = EDGE_CURVE ( 'NONE', #6107, #2531, #26192, .T. ) ;
#9006 = CARTESIAN_POINT ( 'NONE',  ( 123.2161110609119703, -6.340755971794695078, -8.611740276972781771 ) ) ;
#9007 = DIRECTION ( 'NONE',  ( -0.7871354856660202071, 0.6167752151498580027, 0.002461946824133919541 ) ) ;
#9008 = CARTESIAN_POINT ( 'NONE',  ( 118.9794681442453026, -0.8288870151387760510, -10.36305467784173118 ) ) ;
#9009 = CARTESIAN_POINT ( 'NONE',  ( 125.2761281442453054, -10.63000616557722466, -14.87417383870573495 ) ) ;
#9010 = CARTESIAN_POINT ( 'NONE',  ( 126.2252495083089343, -5.683655150050220151, -18.32939578658380952 ) ) ;
#9011 = ORIENTED_EDGE ( 'NONE', *, *, #43495, .F. ) ;
#9012 = CARTESIAN_POINT ( 'NONE',  ( 67.08264006073221708, -20.21382323020432992, -10.89321520033831447 ) ) ;
#9013 = CARTESIAN_POINT ( 'NONE',  ( 108.0517077545248696, -2.791137627527939813, -18.39754474579286025 ) ) ;
#9014 = CARTESIAN_POINT ( 'NONE',  ( 117.9016614775786280, -0.1624402480850797581, -16.17319339645315424 ) ) ;
#9015 = LINE ( 'NONE', #22913, #38390 ) ;
#9016 = CARTESIAN_POINT ( 'NONE',  ( 64.17717360238856372, -59.27884951796255564, -42.87418841894955790 ) ) ;
#9017 = DIRECTION ( 'NONE',  ( 0.9609149988134837450, -0.1028163501681639419, 0.2570431154366518145 ) ) ;
#9019 = CARTESIAN_POINT ( 'NONE',  ( 121.0783548109119749, 0.2603800115204892296, -16.42320221600525088 ) ) ;
#9018 = CARTESIAN_POINT ( 'NONE',  ( 69.35389446611465303, -26.13003040042851666, -5.855554755288591373 ) ) ;
#9020 = CARTESIAN_POINT ( 'NONE',  ( 121.8725281442453223, -6.222761293078241884, -8.102969835052219238 ) ) ;
#9021 = VERTEX_POINT ( 'NONE', #2232 ) ;
#9022 = DIRECTION ( 'NONE',  ( 0.000000000000000000, 0.9242245927363040847, 0.3818493186865896671 ) ) ;
#9023 = CARTESIAN_POINT ( 'NONE',  ( 126.2872529661361654, 0.06646519102223864828, -14.41099760634975269 ) ) ;
#9024 = CARTESIAN_POINT ( 'NONE',  ( 108.5378796295247810, -4.863998795839590272, -8.388885654883775800 ) ) ;
#9025 = CARTESIAN_POINT ( 'NONE',  ( 121.9292548109119849, -7.894159318335828068, -9.358103419637847864 ) ) ;
#9026 = CARTESIAN_POINT ( 'NONE',  ( 120.0572748109119772, -6.222761293078241884, -8.102969835052219238 ) ) ;
#9027 = CARTESIAN_POINT ( 'NONE',  ( 125.3303382280814589, 1.196307385452442196, -17.12740918756453112 ) ) ;
#9028 = CARTESIAN_POINT ( 'NONE',  ( 115.2053796295247849, -4.863998795839590272, -8.388885654883775800 ) ) ;
#9029 = CARTESIAN_POINT ( 'NONE',  ( 68.56885555382550024, -20.41671115022304406, -12.39321520033831447 ) ) ;
#9030 = CARTESIAN_POINT ( 'NONE',  ( 126.2184548109119788, -4.863998795839242995, -13.39321520033831447 ) ) ;
#9031 = CARTESIAN_POINT ( 'NONE',  ( -13.38014282662990162, -5.026713647828855436, -8.593215200338319093 ) ) ;
#9032 = EDGE_CURVE ( 'NONE', #9608, #38611, #4981, .T. ) ;
#9033 = CARTESIAN_POINT ( 'NONE',  ( 109.5796765045248122, -7.250697342233347165, -19.15521520033831138 ) ) ;
#9034 = CARTESIAN_POINT ( 'NONE',  ( 151.2860562277021472, -4.863998795839242995, -13.39321520033831447 ) ) ;
#9035 = CARTESIAN_POINT ( 'NONE',  ( 114.0246765045248196, -7.250697342233347165, -19.15521520033831138 ) ) ;
#9036 = CARTESIAN_POINT ( 'NONE',  ( 119.8870948109119752, -9.261995988541697145, -16.69588392320189030 ) ) ;
#9037 = CARTESIAN_POINT ( 'NONE',  ( 120.6245414775786458, -9.988377603198976828, -10.36322818467138340 ) ) ;
#9038 = CARTESIAN_POINT ( 'NONE',  ( 107.4266296295248821, -4.863998795839590272, -19.15521520033831493 ) ) ;
#9039 = CARTESIAN_POINT ( 'NONE',  ( 115.3489614775786407, -9.261995988541697145, -16.69588392320189030 ) ) ;
#9040 = DIRECTION ( 'NONE',  ( 0.7962509850245457210, 0.6049664196031383501, 0.000000000000000000 ) ) ;
#9041 = EDGE_LOOP ( 'NONE', ( #32417, #3373, #20530, #37592 ) ) ;
#9042 = LINE ( 'NONE', #32956, #7233 ) ;
#9043 = CARTESIAN_POINT ( 'NONE',  ( 122.2128881442453263, -1.834011780172310813, -8.268836392978581529 ) ) ;
#9044 = CARTESIAN_POINT ( 'NONE',  ( 121.6456214775786293, -10.63000616557722466, -14.87417383870573495 ) ) ;
#9045 = CARTESIAN_POINT ( 'NONE',  ( 126.4106614775786284, -6.222761293078241884, -8.102969835052219238 ) ) ;
#9046 = CARTESIAN_POINT ( 'NONE',  ( 111.8886348109120092, -6.222761293078241884, -8.102969835052219238 ) ) ;
#9047 = CARTESIAN_POINT ( 'NONE',  ( 114.9518748109119883, -7.643976991954077427, -18.09477374809248928 ) ) ;
#9048 = CARTESIAN_POINT ( 'NONE',  ( 124.0281414775786146, -1.834011780172310813, -8.268836392978581529 ) ) ;
#9049 = CARTESIAN_POINT ( 'NONE',  ( 110.0658483795247804, -0.7896495226426338832, -9.318865927141430916 ) ) ;
#9050 = CARTESIAN_POINT ( 'NONE',  ( 120.9081748109119872, -4.153390946401325223, -8.397313243818185668 ) ) ;
#9051 = CARTESIAN_POINT ( 'NONE',  ( 69.69189222814998175, -41.76310523276723785, -24.39321520033831447 ) ) ;
#9052 = DIRECTION ( 'NONE',  ( 0.000000000000000000, -0.3818493186865936084, 0.9242245927363024194 ) ) ;
#9053 = ORIENTED_EDGE ( 'NONE', *, *, #6698, .T. ) ;
#9054 = APPLICATION_CONTEXT ( 'automotive_design' ) ;
#9055 = CIRCLE ( 'NONE', #3224, 2.000000000000000444 ) ;
#9056 = CARTESIAN_POINT ( 'NONE',  ( 69.36136150295220659, -52.75929888348183994, -31.20173714864591830 ) ) ;
#9057 = CARTESIAN_POINT ( 'NONE',  ( 124.1983214775786166, -8.166667518702819706, -8.995218007635861213 ) ) ;
#9058 = CARTESIAN_POINT ( 'NONE',  ( 113.0523327545247838, -6.936859964151250502, -8.388885654883788234 ) ) ;
#9059 = CARTESIAN_POINT ( 'NONE',  ( 124.7442371152539096, 2.096536125358192226, -9.913456651695405242 ) ) ;
#9060 = ADVANCED_FACE ( 'NONE', ( #15479 ), #43296, .T. ) ;
#9061 = CARTESIAN_POINT ( 'NONE',  ( 67.26988314049960138, -0.1294138187462419431, -16.39321520033831447 ) ) ;
#9062 = DIRECTION ( 'NONE',  ( 0.000000000000000000, -1.000000000000000000, 0.000000000000000000 ) ) ;
#9063 = CARTESIAN_POINT ( 'NONE',  ( 123.7445081442452874, -7.894159318335828068, -9.358103419637847864 ) ) ;
#9064 = CARTESIAN_POINT ( 'NONE',  ( 123.4564593026122878, -1.179503403430468333, -17.05068175419387089 ) ) ;
#9065 = CARTESIAN_POINT ( 'NONE',  ( 125.3328548109119964, -0.8288870151387760510, -10.36305467784173118 ) ) ;
#9066 = CARTESIAN_POINT ( 'NONE',  ( 125.1679698639839273, -11.59951594357973725, -16.43112627289485062 ) ) ;
#9067 = CARTESIAN_POINT ( 'NONE',  ( 125.1626748109119802, -9.988377603198980381, -10.36322818467138518 ) ) ;
#9068 =( BOUNDED_CURVE ( )  B_SPLINE_CURVE ( 2, ( #4476, #39133, #31614, #31839, #14295, #28213, #21358, #608, #28431, #18163, #1053, #827, #7900, #14969, #28881, #11554, #15872 ),
 .UNSPECIFIED., .F., .T. ) 
 B_SPLINE_CURVE_WITH_KNOTS ( ( 3, 2, 2, 2, 2, 2, 2, 2, 3 ),
 ( 0.2046282416568590001, 0.2109375000000000000, 0.2187500000000000000, 0.2265625000000000000, 0.2343750000000000000, 0.2421875000000000000, 0.2500000000000000000, 0.2578125000000000000, 0.2641217583431409999 ),
 .UNSPECIFIED. ) 
 CURVE ( )  GEOMETRIC_REPRESENTATION_ITEM ( )  RATIONAL_B_SPLINE_CURVE ( ( 0.9763430640195970289, 0.9385262470928680267, 1.000000000000000000, 0.9238795325112869605, 1.000000000000000000, 0.9238795325112869605, 1.000000000000000000, 0.9238795325112869605, 1.000000000000000000, 0.9238795325112869605, 1.000000000000000000, 0.9238795325112869605, 1.000000000000000000, 0.9238795325112869605, 1.000000000000000000, 0.9385262470928680267, 0.9763430640195970289 ) ) 
 REPRESENTATION_ITEM ( '' )  );
#9069 = CARTESIAN_POINT ( 'NONE',  ( 119.4332814775786318, -8.899110576539710493, -16.42337572283490132 ) ) ;
#9070 = CARTESIAN_POINT ( 'NONE',  ( 124.9924948109119924, -5.574606645277164318, -18.38911715685844683 ) ) ;
#9071 = VERTEX_POINT ( 'NONE', #12519 ) ;
#9072 = CARTESIAN_POINT ( 'NONE',  ( 123.9714148109119805, -0.4660016031367893996, -10.09054647747474043 ) ) ;
#9073 = CARTESIAN_POINT ( 'NONE',  ( 116.7671281442453335, -1.834011780172310813, -8.268836392978581529 ) ) ;
#9074 = CARTESIAN_POINT ( 'NONE',  ( 115.6220983795247861, -8.402594152722688392, -16.93181055722141792 ) ) ;
#9075 = CARTESIAN_POINT ( 'NONE',  ( 113.0798948109119948, -8.899110576539710493, -16.42337572283490132 ) ) ;
#9076 = CARTESIAN_POINT ( 'NONE',  ( 125.7866681442452688, -8.899110576539710493, -16.42337572283490132 ) ) ;
#9077 = CARTESIAN_POINT ( 'NONE',  ( 124.8790414775786246, -0.4660016031367893996, -10.09054647747474043 ) ) ;
#9078 = CARTESIAN_POINT ( 'NONE',  ( 115.8999108795247821, -8.938348069036489818, -9.318865927141430916 ) ) ;
#9079 = CARTESIAN_POINT ( 'NONE',  ( 110.4825671295247815, 0.1403307496149613920, -13.39321520033831447 ) ) ;
#9080 = DIRECTION ( 'NONE',  ( 0.000000000000000000, 0.000000000000000000, 1.000000000000000000 ) ) ;
#9081 = VECTOR ( 'NONE', #24110, 1000.000000000000114 ) ;
#9082 = CARTESIAN_POINT ( 'NONE',  ( 69.36136150295220659, -58.12267893792004259, -33.34707047463405871 ) ) ;
#9083 = CARTESIAN_POINT ( 'NONE',  ( 117.4478481442453131, -9.565557343593413364, -10.61323700422348004 ) ) ;
#9084 = CARTESIAN_POINT ( 'NONE',  ( 72.30589087944665039, -67.07702721507251908, -42.22679270393576445 ) ) ;
#9085 = CARTESIAN_POINT ( 'NONE',  ( 115.7610046295247912, -4.863998795839590272, -18.39754474579285315 ) ) ;
#9086 = ORIENTED_EDGE ( 'NONE', *, *, #44338, .F. ) ;
#9087 = CARTESIAN_POINT ( 'NONE',  ( 123.5743281442453139, -2.084020599724406786, -8.691656652584148546 ) ) ;
#9088 = CARTESIAN_POINT ( 'NONE',  ( 120.2990798109119766, -7.200787124940443817, -17.81845355600750835 ) ) ;
#9089 = CARTESIAN_POINT ( 'NONE',  ( 122.1743141859119817, -0.8832429491016019485, -18.19431474523657855 ) ) ;
#9090 = ORIENTED_EDGE ( 'NONE', *, *, #9573, .T. ) ;
#9091 = CARTESIAN_POINT ( 'NONE',  ( 123.7325746589382192, -8.341213398351550623, -17.25835129106723542 ) ) ;
#9092 = AXIS2_PLACEMENT_3D ( 'NONE', #12040, #37078, #5852 ) ;
#9093 = CARTESIAN_POINT ( 'NONE',  ( 116.6762522984324733, -11.82972831326674168, -21.28207584875485026 ) ) ;
#9094 = ORIENTED_EDGE ( 'NONE', *, *, #44807, .F. ) ;
#9095 = CARTESIAN_POINT ( 'NONE',  ( 118.5256548109119876, -0.4660016031367893996, -10.09054647747474043 ) ) ;
#9096 = CARTESIAN_POINT ( 'NONE',  ( 124.9924948109119924, -5.574606645277164318, -18.38911715685844683 ) ) ;
#9097 = CARTESIAN_POINT ( 'NONE',  ( 113.7038881442453402, -6.222761293078241884, -8.102969835052219238 ) ) ;
#9098 = LINE ( 'NONE', #33698, #35131 ) ;
#9099 = CARTESIAN_POINT ( 'NONE',  ( 114.9562903192117034, -2.378957183258582742, -17.95140958770220152 ) ) ;
#9100 = CARTESIAN_POINT ( 'NONE',  ( 114.1577014775786552, -6.344957434206662583, -7.627207830600332805 ) ) ;
#9101 = CARTESIAN_POINT ( 'NONE',  ( 113.1217858795247935, -8.402594152722688392, -9.854619843455216355 ) ) ;
#9102 = CARTESIAN_POINT ( 'NONE',  ( 123.8579614775786126, 0.5811942927096110934, -14.16772938898807510 ) ) ;
#9103 = DIRECTION ( 'NONE',  ( -0.9609149988134837450, 0.1028163501681639419, -0.2570431154366518145 ) ) ;
#9104 = ORIENTED_EDGE ( 'NONE', *, *, #13069, .T. ) ;
#9105 = CARTESIAN_POINT ( 'NONE',  ( 113.7606148109119886, -1.561330072975668060, -17.79121239304076596 ) ) ;
#9106 = CARTESIAN_POINT ( 'NONE',  ( 115.1787814775786387, -0.1624402480850797581, -16.17319339645315424 ) ) ;
#9107 = DIRECTION ( 'NONE',  ( 0.000000000000000000, 0.000000000000000000, -1.000000000000000000 ) ) ;
#9108 = CARTESIAN_POINT ( 'NONE',  ( 112.5126281442453120, -10.30919188438810075, -12.61870101168855918 ) ) ;
#9109 =( GEOMETRIC_REPRESENTATION_CONTEXT ( 3 ) GLOBAL_UNCERTAINTY_ASSIGNED_CONTEXT ( ( #35143 ) ) GLOBAL_UNIT_ASSIGNED_CONTEXT ( ( #10523, #20784, #27408 ) ) REPRESENTATION_CONTEXT ( 'NONE', 'WORKASPACE' ) );
#9110 = ORIENTED_EDGE ( 'NONE', *, *, #2742, .F. ) ;
#9111 = CARTESIAN_POINT ( 'NONE',  ( 121.1918081442452859, 0.9020085738987339008, -11.91225656197089222 ) ) ;
#9112 = CARTESIAN_POINT ( 'NONE',  ( 72.75524511225664526, -21.99489077589588604, -18.39321520033831803 ) ) ;
#9113 = CARTESIAN_POINT ( 'NONE',  ( 109.6491296295247793, -4.863998795839638234, -8.388885654883775800 ) ) ;
#9114 = DIRECTION ( 'NONE',  ( 0.000000000000000000, 0.9284778069183720062, 0.3713878862591650232 ) ) ;
#9115 = CARTESIAN_POINT ( 'NONE',  ( 123.7184548109119788, -4.683672500039349984, -14.88233656108870662 ) ) ;
#9116 = VECTOR ( 'NONE', #6475, 1000.000000000000000 ) ;
#9117 = CARTESIAN_POINT ( 'NONE',  ( 115.9729548109119861, -3.505236298600246325, -18.68346056562440793 ) ) ;
#9118 = EDGE_CURVE ( 'NONE', #2964, #44682, #14436, .T. ) ;
#9119 = LINE ( 'NONE', #8893, #43025 ) ;
#9120 = CARTESIAN_POINT ( 'NONE',  ( 125.3567159805640756, -2.805979814341523326, -20.12909359689052380 ) ) ;
#9121 = CARTESIAN_POINT ( 'NONE',  ( 113.4769814775786330, 0.4262465694468514643, -12.03445270309931736 ) ) ;
#9122 = CARTESIAN_POINT ( 'NONE',  ( 126.1837548109119496, 0.4262465694468514643, -12.03445270309931736 ) ) ;
#9123 = CARTESIAN_POINT ( 'NONE',  ( 123.9106423109119675, -0.4387604401700512802, -15.73000352943951619 ) ) ;
#9124 = CARTESIAN_POINT ( 'NONE',  ( 112.8529881442453302, -1.561330072975668060, -17.79121239304076596 ) ) ;
#9125 = CARTESIAN_POINT ( 'NONE',  ( 116.0296814775786345, -1.833838273342658809, -17.42832698103878286 ) ) ;
#9126 = CARTESIAN_POINT ( 'NONE',  ( 124.7655881442452852, 0.5811942927096110934, -14.16772938898807510 ) ) ;
#9127 = CARTESIAN_POINT ( 'NONE',  ( 122.2696148109119889, -4.089484607189486809, -7.948022111789456723 ) ) ;
#9128 = EDGE_LOOP ( 'NONE', ( #23639, #15600, #33915, #40784, #27439, #30548 ) ) ;
#9129 = CARTESIAN_POINT ( 'NONE',  ( 113.9307948109119906, 0.9020085738987339008, -11.91225656197089222 ) ) ;
#9130 = ADVANCED_FACE ( 'NONE', ( #18893 ), #15249, .F. ) ;
#9131 = CARTESIAN_POINT ( 'NONE',  ( 112.3578015045248861, -2.477300249445798297, -7.631215200338321125 ) ) ;
#9132 = CARTESIAN_POINT ( 'NONE',  ( 110.1353015045248469, -6.936859964151250502, -18.39754474579286025 ) ) ;
#9133 = CARTESIAN_POINT ( 'NONE',  ( 110.2742077545248094, -2.791137627527939813, -18.39754474579286025 ) ) ;
#9134 = CARTESIAN_POINT ( 'NONE',  ( 128.1691939224698729, -3.811125363834908963, -16.04426352910759235 ) ) ;
#9135 = CARTESIAN_POINT ( 'NONE',  ( 117.9016614775786280, -9.988377603198976828, -10.36322818467138340 ) ) ;
#9136 = EDGE_LOOP ( 'NONE', ( #5669, #30467, #21637, #23005, #41024 ) ) ;
#9137 = CARTESIAN_POINT ( 'NONE',  ( 61.76986277844709861, -39.32091226840162079, -4.893215200338314474 ) ) ;
#9138 = DIRECTION ( 'NONE',  ( 0.7400066460894876297, -0.6725995567522979890, -0.000000000000000000 ) ) ;
#9139 = FACE_OUTER_BOUND ( 'NONE', #40245, .T. ) ;
#9140 = CARTESIAN_POINT ( 'NONE',  ( 115.5191414775786569, -6.222761293078241884, -8.102969835052219238 ) ) ;
#9141 = CARTESIAN_POINT ( 'NONE',  ( 107.7044421295247929, -9.868328341294093420, -13.39321520033831447 ) ) ;
#9142 = CARTESIAN_POINT ( 'NONE',  ( 120.3409081442453044, -0.4660016031367893996, -10.09054647747474043 ) ) ;
#9143 = CARTESIAN_POINT ( 'NONE',  ( 110.6909265045248247, -7.250697342233347165, -19.15521520033831138 ) ) ;
#9144 = DIRECTION ( 'NONE',  ( 0.000000000000000000, 0.9284778069183720062, 0.3713878862591650232 ) ) ;
#9145 = ORIENTED_EDGE ( 'NONE', *, *, #27260, .T. ) ;
#9146 = CARTESIAN_POINT ( 'NONE',  ( 120.8514481442453103, -2.084020599724394796, -8.691656652584146769 ) ) ;
#9147 = CARTESIAN_POINT ( 'NONE',  ( 122.6099748109119929, -0.8288870151387760510, -10.36305467784173118 ) ) ;
#9148 = CARTESIAN_POINT ( 'NONE',  ( 120.8514481442452961, -7.893985811506177619, -18.51759400769804742 ) ) ;
#9149 = CARTESIAN_POINT ( 'NONE',  ( 113.9875214775786532, -8.899110576539710493, -16.42337572283490132 ) ) ;
#9150 = CARTESIAN_POINT ( 'NONE',  ( 115.2355081442453155, -10.30919188438810075, -12.61870101168855918 ) ) ;
#9151 = ADVANCED_FACE ( 'NONE', ( #29156 ), #4232, .T. ) ;
#9152 = LINE ( 'NONE', #40618, #9650 ) ;
#9153 = CARTESIAN_POINT ( 'NONE',  ( 124.8223148109119762, -10.15424416112533912, -14.75197769757731336 ) ) ;
#9154 = CARTESIAN_POINT ( 'NONE',  ( 118.2987481442453088, -7.894159318335828068, -9.358103419637847864 ) ) ;
#9155 = VERTEX_POINT ( 'NONE', #36659 ) ;
#9156 = EDGE_CURVE ( 'NONE', #13839, #43475, #7769, .T. ) ;
#9157 = ADVANCED_FACE ( 'NONE', ( #5432 ), #23927, .F. ) ;
#9158 = VECTOR ( 'NONE', #13335, 1000.000000000000114 ) ;
#9159 = CARTESIAN_POINT ( 'NONE',  ( 124.1190016859119680, -9.665098340737509730, -17.37397104707595474 ) ) ;
#9160 = CARTESIAN_POINT ( 'NONE',  ( 113.5904348109119866, -7.893985811506177619, -18.51759400769804742 ) ) ;
#9161 = CARTESIAN_POINT ( 'NONE',  ( 122.1561614775786353, -8.899110576539710493, -16.42337572283490132 ) ) ;
#9162 = ORIENTED_EDGE ( 'NONE', *, *, #27531, .T. ) ;
#9163 = CARTESIAN_POINT ( 'NONE',  ( 122.2437673109119629, -9.289237151508434209, -11.05642687123711276 ) ) ;
#9164 = CARTESIAN_POINT ( 'NONE',  ( 117.8449348109119938, -8.166667518702817929, -8.995218007635861213 ) ) ;
#9165 = CARTESIAN_POINT ( 'NONE',  ( 111.3854577545248645, -7.250697342233347165, -7.631215200338321125 ) ) ;
#9166 = CARTESIAN_POINT ( 'NONE',  ( 115.1220548109119761, -1.833838273342658809, -17.42832698103878286 ) ) ;
#9167 = ORIENTED_EDGE ( 'NONE', *, *, #7185, .F. ) ;
#9168 = VERTEX_POINT ( 'NONE', #15936 ) ;
#9169 = CARTESIAN_POINT ( 'NONE',  ( 124.4252281442452812, -0.8288870151387760510, -10.36305467784173118 ) ) ;
#9170 = AXIS2_PLACEMENT_3D ( 'NONE', #37507, #2395, #16324 ) ;
#9171 = CARTESIAN_POINT ( 'NONE',  ( 120.6245414775786458, -0.1624402480850797581, -16.17319339645315424 ) ) ;
#9172 = LINE ( 'NONE', #12829, #22849 ) ;
#9173 = CARTESIAN_POINT ( 'NONE',  ( 117.4478481442453131, 0.2603800115204892296, -16.42320221600525088 ) ) ;
#9174 = AXIS2_PLACEMENT_3D ( 'NONE', #28750, #35564, #18709 ) ;
#9175 = DIRECTION ( 'NONE',  ( -0.4461977533474357771, 0.3417300876246960328, -0.8271203734159368048 ) ) ;
#9176 = CARTESIAN_POINT ( 'NONE',  ( 115.0653281442453277, -6.344957434206662583, -7.627207830600332805 ) ) ;
#9178 = CARTESIAN_POINT ( 'NONE',  ( 116.2565881442453133, -0.8288870151387760510, -10.36305467784173118 ) ) ;
#9177 = CARTESIAN_POINT ( 'NONE',  ( 114.1009748109119784, -4.089484607189486809, -7.948022111789456723 ) ) ;
#9179 = CARTESIAN_POINT ( 'NONE',  ( 124.4252281442452812, -0.8288870151387760510, -10.36305467784173118 ) ) ;
#9180 = CARTESIAN_POINT ( 'NONE',  ( 113.7606148109119886, -1.561330072975668060, -17.79121239304076596 ) ) ;
#9181 = ORIENTED_EDGE ( 'NONE', *, *, #10964, .F. ) ;
#9182 = VECTOR ( 'NONE', #42713, 1000.000000000000000 ) ;
#9183 = CARTESIAN_POINT ( 'NONE',  ( 124.0281414775786146, -7.643976991954077427, -18.09477374809248928 ) ) ;
#9184 = CARTESIAN_POINT ( 'NONE',  ( 122.9503348109119827, 0.5811942927096136469, -14.16772938898805378 ) ) ;
#9185 = ADVANCED_FACE ( 'NONE', ( #29835 ), #19573, .T. ) ;
#9186 = CARTESIAN_POINT ( 'NONE',  ( 90.04708369096697140, -25.99489077589524300, -13.39321520033831447 ) ) ;
#9187 = CARTESIAN_POINT ( 'NONE',  ( 114.3719421295247827, 0.8980012041604618078, -13.39321520033831447 ) ) ;
#9188 = CARTESIAN_POINT ( 'NONE',  ( 114.7886608795247696, -1.325403438956436419, -16.93181055722141792 ) ) ;
#9189 = CARTESIAN_POINT ( 'NONE',  ( 112.5661608795247872, -8.938348069036489818, -9.318865927141430916 ) ) ;
#9190 = AXIS2_PLACEMENT_3D ( 'NONE', #26427, #11848, #1565 ) ;
#9191 = CARTESIAN_POINT ( 'NONE',  ( 123.0637881442452937, -0.4660016031367893996, -10.09054647747474043 ) ) ;
#9192 = VERTEX_POINT ( 'NONE', #36436 ) ;
#9193 = CARTESIAN_POINT ( 'NONE',  ( 121.2485348109119769, -0.4660016031367893996, -10.09054647747474043 ) ) ;
#9194 = DIRECTION ( 'NONE',  ( 0.000000000000000000, 0.000000000000000000, -1.000000000000000000 ) ) ;
#9195 = CARTESIAN_POINT ( 'NONE',  ( 106.8015515045248378, -2.477300249445798297, -7.631215200338321125 ) ) ;
#9196 = CARTESIAN_POINT ( 'NONE',  ( 121.0216281442452981, -1.561330072975668948, -17.79121239304076951 ) ) ;
#9197 = CARTESIAN_POINT ( 'NONE',  ( 120.0572748109119772, -3.383040157471821630, -19.15922257007629170 ) ) ;
#9198 = CARTESIAN_POINT ( 'NONE',  ( 63.69189222814998175, -82.08636712479707853, -32.64558696907351987 ) ) ;
#9199 = CARTESIAN_POINT ( 'NONE',  ( 120.3439060953690642, -6.001247023715329476, -18.26661038929047720 ) ) ;
#9200 = CARTESIAN_POINT ( 'NONE',  ( 119.2572829359120021, -5.367793381288652910, -18.78638297431638904 ) ) ;
#9201 = ORIENTED_EDGE ( 'NONE', *, *, #31738, .F. ) ;
#9202 = CARTESIAN_POINT ( 'NONE',  ( -2.533732661084656002, -7.044826992859106518, -7.503826880137411059 ) ) ;
#9203 = DIRECTION ( 'NONE',  ( 1.000000000000000000, 0.000000000000000000, 0.000000000000000000 ) ) ;
#9204 = CARTESIAN_POINT ( 'NONE',  ( 123.1205148109119563, -7.643976991954077427, -18.09477374809248928 ) ) ;
#9205 = AXIS2_PLACEMENT_3D ( 'NONE', #13580, #109, #27490 ) ;
#9206 = CARTESIAN_POINT ( 'NONE',  ( 116.3860827545247787, -2.477300249445798297, -19.15521520033831138 ) ) ;
#9207 = CARTESIAN_POINT ( 'NONE',  ( 111.2465515045248168, -6.936859964151250502, -18.39754474579286025 ) ) ;
#9208 = CARTESIAN_POINT ( 'NONE',  ( 116.9940348109119839, -0.1624402480850797581, -16.17319339645315424 ) ) ;
#9209 = LINE ( 'NONE', #27829, #11029 ) ;
#9210 = CARTESIAN_POINT ( 'NONE',  ( 69.24446145078422887, -25.84570955357843758, -5.871778085103664502 ) ) ;
#9211 = CARTESIAN_POINT ( 'NONE',  ( 112.4559014775786778, -0.1624402480850797581, -16.17319339645315424 ) ) ;
#9212 = CARTESIAN_POINT ( 'NONE',  ( 125.2194014775786286, -10.30919188438810075, -12.61870101168855918 ) ) ;
#9213 = VERTEX_POINT ( 'NONE', #8414 ) ;
#9214 = EDGE_CURVE ( 'NONE', #30187, #24697, #5654, .T. ) ;
#9215 = CARTESIAN_POINT ( 'NONE',  ( 123.2339681442453241, -3.505236298600246325, -18.68346056562440793 ) ) ;
#9216 = CARTESIAN_POINT ( 'NONE',  ( 116.7671281442453335, -1.834011780172310813, -8.268836392978581529 ) ) ;
#9217 = CARTESIAN_POINT ( 'NONE',  ( 121.3619881442452879, -4.089484607189486809, -7.948022111789456723 ) ) ;
#9218 = CARTESIAN_POINT ( 'NONE',  ( 122.6667014775786413, -2.084020599724406786, -8.691656652584148546 ) ) ;
#9219 = ORIENTED_EDGE ( 'NONE', *, *, #13074, .T. ) ;
#9220 = EDGE_CURVE ( 'NONE', #34283, #42441, #45046, .T. ) ;
#9221 = FACE_OUTER_BOUND ( 'NONE', #3208, .T. ) ;
#9222 = AXIS2_PLACEMENT_3D ( 'NONE', #38744, #4083, #7741 ) ;
#9223 = CARTESIAN_POINT ( 'NONE',  ( 124.7655881442452852, 0.5811942927096110934, -14.16772938898807510 ) ) ;
#9224 = CARTESIAN_POINT ( 'NONE',  ( 113.8740681442453138, -9.859900752359374465, -12.68260735090039404 ) ) ;
#9225 = CARTESIAN_POINT ( 'NONE',  ( 125.3328548109119964, -9.261995988541697145, -16.69588392320189030 ) ) ;
#9226 = CARTESIAN_POINT ( 'NONE',  ( 108.6767858795247861, -0.7896495226426338832, -17.46756447353520159 ) ) ;
#9227 = FACE_OUTER_BOUND ( 'NONE', #38110, .T. ) ;
#9228 = ORIENTED_EDGE ( 'NONE', *, *, #21674, .F. ) ;
#9229 = CARTESIAN_POINT ( 'NONE',  ( 119.0405381477680038, -2.280480477428463715, -18.08254604495226658 ) ) ;
#9230 = CARTESIAN_POINT ( 'NONE',  ( 108.1211608795247798, -1.325403438956436419, -16.93181055722141792 ) ) ;
#9231 = CIRCLE ( 'NONE', #15057, 1.610000000000000986 ) ;
#9232 = PLANE ( 'NONE',  #24143 ) ;
#9233 = CARTESIAN_POINT ( 'NONE',  ( 118.5256548109119876, -8.899110576539710493, -16.42337572283490132 ) ) ;
#9234 = CARTESIAN_POINT ( 'NONE',  ( 115.0653281442453277, -3.505236298600246325, -18.68346056562440793 ) ) ;
#9235 = CARTESIAN_POINT ( 'NONE',  ( 125.7299414775786204, -10.15424416112551143, -14.75197769757842181 ) ) ;
#9236 = EDGE_LOOP ( 'NONE', ( #16536, #8514, #19385, #43081, #20711, #39419 ) ) ;
#9237 = CARTESIAN_POINT ( 'NONE',  ( 115.6740958961590593, -2.263366209404225504, -18.10533625161308180 ) ) ;
#9238 = CARTESIAN_POINT ( 'NONE',  ( 116.6536748109119941, -10.15424416112533912, -14.75197769757731336 ) ) ;
#9239 = CARTESIAN_POINT ( 'NONE',  ( 113.6471614775786492, -4.153390946401321671, -8.397313243818183892 ) ) ;
#9240 = CARTESIAN_POINT ( 'NONE',  ( 65.10287265247758626, -0.4742552606671335269, -10.39321520033831625 ) ) ;
#9241 = LINE ( 'NONE', #24059, #42796 ) ;
#9243 = CARTESIAN_POINT ( 'NONE',  ( 122.2696148109119889, -4.089484607189486809, -7.948022111789456723 ) ) ;
#9242 = DIRECTION ( 'NONE',  ( 0.3445294493088631449, 0.9387755102040804545, 0.000000000000000000 ) ) ;
#9244 = CARTESIAN_POINT ( 'NONE',  ( 124.4819548109119722, -2.084020599724406786, -8.691656652584148546 ) ) ;
#9245 = VERTEX_POINT ( 'NONE', #37107 ) ;
#9246 = DIRECTION ( 'NONE',  ( 1.000000000000000000, 0.000000000000000000, 0.000000000000000000 ) ) ;
#9247 = CARTESIAN_POINT ( 'NONE',  ( 125.9001214775786224, -4.089484607189486809, -7.948022111789456723 ) ) ;
#9248 = CARTESIAN_POINT ( 'NONE',  ( 110.2047546295247855, -4.863998795839590272, -18.39754474579285315 ) ) ;
#9249 = EDGE_CURVE ( 'NONE', #42907, #37027, #33354, .T. ) ;
#9250 = CARTESIAN_POINT ( 'NONE',  ( 125.1059481442452750, -1.833838273342660141, -17.42832698103878286 ) ) ;
#9251 = VECTOR ( 'NONE', #3394, 1000.000000000000227 ) ;
#9252 = CARTESIAN_POINT ( 'NONE',  ( 120.3409081442453044, -8.899110576539710493, -16.42337572283490132 ) ) ;
#9253 = CARTESIAN_POINT ( 'NONE',  ( 125.1375072647520312, 1.201293586859333296, -17.68058412753241626 ) ) ;
#9254 = CARTESIAN_POINT ( 'NONE',  ( 112.8439733795247832, -1.325403438956436419, -9.854619843455211026 ) ) ;
#9255 = CARTESIAN_POINT ( 'NONE',  ( 117.0507614775786465, -10.30919188438810252, -12.61870101168856628 ) ) ;
#9256 = DIRECTION ( 'NONE',  ( -0.9908103287288505534, 0.1352586133457950313, 0.000000000000000000 ) ) ;
#9257 = CARTESIAN_POINT ( 'NONE',  ( 114.0442481442453300, -7.643976991954077427, -18.09477374809248928 ) ) ;
#9258 = CARTESIAN_POINT ( 'NONE',  ( 110.4825671295247815, -10.62599879583958540, -13.39321520033831447 ) ) ;
#9259 = CARTESIAN_POINT ( 'NONE',  ( -13.49558570875300134, -4.874768836305437780, -18.10912819220449421 ) ) ;
#9260 = CARTESIAN_POINT ( 'NONE',  ( 114.7192077545248594, -7.250697342233347165, -7.631215200338321125 ) ) ;
#9261 = CARTESIAN_POINT ( 'NONE',  ( 121.1350814775786233, 0.5811942927096110934, -14.16772938898807510 ) ) ;
#9262 = CARTESIAN_POINT ( 'NONE',  ( 120.7379948109119709, -10.63000616557722466, -14.87417383870573495 ) ) ;
#9263 =( BOUNDED_CURVE ( )  B_SPLINE_CURVE ( 3, ( #37855, #19687, #38294, #41740 ),
 .UNSPECIFIED., .F., .T. ) 
 B_SPLINE_CURVE_WITH_KNOTS ( ( 4, 4 ),
 ( 3.141592653589795336, 6.283185307179590673 ),
 .UNSPECIFIED. ) 
 CURVE ( )  GEOMETRIC_REPRESENTATION_ITEM ( )  RATIONAL_B_SPLINE_CURVE ( ( 1.000000000000000000, 0.3333333333333335369, 0.3333333333333335369, 1.000000000000000000 ) ) 
 REPRESENTATION_ITEM ( '' )  );
#9264 = CARTESIAN_POINT ( 'NONE',  ( 117.8449348109119938, -8.166667518702817929, -8.995218007635861213 ) ) ;
#9265 = CARTESIAN_POINT ( 'NONE',  ( 113.1933481442453058, -4.089484607189486809, -7.948022111789456723 ) ) ;
#9266 = ORIENTED_EDGE ( 'NONE', *, *, #41493, .T. ) ;
#9267 = CARTESIAN_POINT ( 'NONE',  ( 113.6471614775786492, -4.153390946401321671, -8.397313243818183892 ) ) ;
#9268 = CARTESIAN_POINT ( 'NONE',  ( 112.6260814775786514, -0.8288870151387760510, -10.36305467784173118 ) ) ;
#9269 = CARTESIAN_POINT ( 'NONE',  ( 120.4543614775786295, -4.089484607189486809, -7.948022111789456723 ) ) ;
#9270 = EDGE_CURVE ( 'NONE', #9298, #38344, #25380, .T. ) ;
#9271 = CARTESIAN_POINT ( 'NONE',  ( 124.6521348109119884, -7.894159318335828068, -9.358103419637847864 ) ) ;
#9272 = CIRCLE ( 'NONE', #28922, 2.999999999999999556 ) ;
#9273 = EDGE_CURVE ( 'NONE', #11473, #6307, #41687, .T. ) ;
#9274 = CARTESIAN_POINT ( 'NONE',  ( 112.5126281442453120, 0.1319031606808879209, -14.10382304977623669 ) ) ;
#9275 = ORIENTED_EDGE ( 'NONE', *, *, #17740, .T. ) ;
#9276 = CARTESIAN_POINT ( 'NONE',  ( 118.6391081442452986, -5.574606645277164318, -18.38911715685844683 ) ) ;
#9277 = CARTESIAN_POINT ( 'NONE',  ( 111.3780948109119890, -5.574606645277164318, -18.38911715685844683 ) ) ;
#9278 = CARTESIAN_POINT ( 'NONE',  ( 107.8433483795247838, -0.7896495226426338832, -9.318865927141430916 ) ) ;
#9279 = CARTESIAN_POINT ( 'NONE',  ( 121.0783548109119749, -9.565557343593413364, -10.61323700422348004 ) ) ;
#9280 = CARTESIAN_POINT ( 'NONE',  ( 116.8179980013510857, -1.923079332374536099, -17.71147565550795022 ) ) ;
#9281 = CARTESIAN_POINT ( 'NONE',  ( 67.69189222814998175, -62.82237896425675672, -47.71602681600972318 ) ) ;
#9282 = EDGE_LOOP ( 'NONE', ( #39307, #16680, #11885, #11488, #22212 ) ) ;
#9283 = AXIS2_PLACEMENT_3D ( 'NONE', #30485, #44636, #9292 ) ;
#9284 = CARTESIAN_POINT ( 'NONE',  ( 121.5492360609119800, -3.387241619883791355, -18.17469012370385073 ) ) ;
#9285 = CARTESIAN_POINT ( 'NONE',  ( 124.5954081442453116, -3.383040157471821630, -19.15922257007629170 ) ) ;
#9286 = DIRECTION ( 'NONE',  ( -1.000000000000000000, 0.000000000000000000, 0.000000000000000000 ) ) ;
#9287 = CARTESIAN_POINT ( 'NONE',  ( 111.8886348109120092, -3.383040157471821630, -19.15922257007629170 ) ) ;
#9288 = CARTESIAN_POINT ( 'NONE',  ( 122.0563581739442895, -4.756192495830085853, -19.39047411591440095 ) ) ;
#9289 = LINE ( 'NONE', #13166, #36909 ) ;
#9290 = CARTESIAN_POINT ( 'NONE',  ( 109.3018640045248304, 0.1403307496149616695, -15.46607636864997204 ) ) ;
#9291 = CARTESIAN_POINT ( 'NONE',  ( 79.05243529145373316, 4.793396140045460108, -21.04957699274893557 ) ) ;
#9292 = DIRECTION ( 'NONE',  ( 0.000000000000000000, -0.3818493186865927203, 0.9242245927363029745 ) ) ;
#9293 = CARTESIAN_POINT ( 'NONE',  ( 124.7127519260344997, -11.83533031758874898, -16.88573608159204653 ) ) ;
#9295 = CARTESIAN_POINT ( 'NONE',  ( 126.1837548109119211, -10.63000616557722466, -14.87417383870573495 ) ) ;
#9294 = VECTOR ( 'NONE', #22862, 1000.000000000000000 ) ;
#9296 = CARTESIAN_POINT ( 'NONE',  ( 116.8805814775786445, -3.505236298600246325, -18.68346056562440793 ) ) ;
#9297 = CARTESIAN_POINT ( 'NONE',  ( 119.7434548109119845, 0.09318999503389145678, -15.44192152833163334 ) ) ;
#9298 = VERTEX_POINT ( 'NONE', #44432 ) ;
#9299 = CARTESIAN_POINT ( 'NONE',  ( 123.9146881442452894, 0.9020085738987339008, -11.91225656197089222 ) ) ;
#9300 = CARTESIAN_POINT ( 'NONE',  ( 113.9875214775786532, -0.4660016031367893996, -10.09054647747474043 ) ) ;
#9301 = CARTESIAN_POINT ( 'NONE',  ( 117.1500671295247713, 0.1403307496149613920, -13.39321520033831447 ) ) ;
#9302 = DIRECTION ( 'NONE',  ( -0.9908103287288504424, 0.1352586133457950590, 0.000000000000000000 ) ) ;
#9303 = CARTESIAN_POINT ( 'NONE',  ( 124.7088614775786226, -9.565557343593413364, -10.61323700422348004 ) ) ;
#9304 = CARTESIAN_POINT ( 'NONE',  ( 125.4463081442452932, -5.638512984488999180, -18.83840828888717311 ) ) ;
#9305 = CARTESIAN_POINT ( 'NONE',  ( 106.5931921295248372, -9.868328341294093420, -13.39321520033831447 ) ) ;
#9306 = CARTESIAN_POINT ( 'NONE',  ( 109.5796765045248122, -2.791137627527939813, -8.388885654883777576 ) ) ;
#9307 = CARTESIAN_POINT ( 'NONE',  ( 83.49267580666517574, -32.76310523276723785, -23.89321520033831803 ) ) ;
#9308 = CARTESIAN_POINT ( 'NONE',  ( 116.3133148109120043, -2.084020599724406786, -8.691656652584148546 ) ) ;
#9309 = CARTESIAN_POINT ( 'NONE',  ( 117.5045748109119756, -9.859900752359374465, -12.68260735090039404 ) ) ;
#9310 = DIRECTION ( 'NONE',  ( -0.9063289528979890930, -0.4225728684367167087, 0.000000000000000000 ) ) ;
#9311 = CARTESIAN_POINT ( 'NONE',  ( 112.4967077545247633, -2.791137627527939813, -18.39754474579286025 ) ) ;
#9312 = ORIENTED_EDGE ( 'NONE', *, *, #24773, .F. ) ;
#9313 = CYLINDRICAL_SURFACE ( 'NONE', #26981, 1.999999999999998890 ) ;
#9314 = CARTESIAN_POINT ( 'NONE',  ( 126.4106614775786284, -6.222761293078241884, -8.102969835052219238 ) ) ;
#9315 = CARTESIAN_POINT ( 'NONE',  ( 123.2161110609119561, -3.163656168406935087, -18.89861972220014508 ) ) ;
#9316 = CARTESIAN_POINT ( 'NONE',  ( 122.3826735609119680, -9.645473719204776586, -14.86997237629376656 ) ) ;
#9317 = ORIENTED_EDGE ( 'NONE', *, *, #32665, .F. ) ;
#9318 = DIRECTION ( 'NONE',  ( 0.9609149988134843001, -0.1028163501681632064, 0.2570431154366505933 ) ) ;
#9319 = CARTESIAN_POINT ( 'NONE',  ( 117.0649885480837042, -11.39702756529595540, -21.68909395195552392 ) ) ;
#9320 = EDGE_LOOP ( 'NONE', ( #24900, #23436, #34370, #9353, #45004, #33871 ) ) ;
#9321 = CARTESIAN_POINT ( 'NONE',  ( 117.7314814775786260, -4.089484607189486809, -7.948022111789456723 ) ) ;
#9322 = CARTESIAN_POINT ( 'NONE',  ( 125.8433948109119456, -7.643976991954077427, -18.09477374809248928 ) ) ;
#9323 = EDGE_CURVE ( 'NONE', #22022, #13784, #44888, .T. ) ;
#9324 = CARTESIAN_POINT ( 'NONE',  ( 115.6325948109119821, -9.565557343593413364, -10.61323700422348004 ) ) ;
#9325 = CARTESIAN_POINT ( 'NONE',  ( 116.2050738206745137, -2.348512537728063787, -17.99195118506216318 ) ) ;
#9326 = CARTESIAN_POINT ( 'NONE',  ( 124.1983214775786166, -8.166667518702828588, -8.995218007635868318 ) ) ;
#9327 = CARTESIAN_POINT ( 'NONE',  ( 114.1009748109119784, -4.089484607189486809, -7.948022111789456723 ) ) ;
#9328 = CARTESIAN_POINT ( 'NONE',  ( 110.2742077545248094, -2.791137627527939813, -18.39754474579286025 ) ) ;
#9329 = CARTESIAN_POINT ( 'NONE',  ( 123.2339681442453241, -6.344957434206665248, -7.627207830600338134 ) ) ;
#9330 = DIRECTION ( 'NONE',  ( 0.000000000000000000, -0.3818493186865936084, 0.9242245927363024194 ) ) ;
#9331 = EDGE_LOOP ( 'NONE', ( #22443, #42916, #24039, #4522, #19586, #21662, #25451, #16566, #28743 ) ) ;
#9332 = CARTESIAN_POINT ( 'NONE',  ( 114.5547881442453217, -5.638512984488999180, -18.83840828888717311 ) ) ;
#9333 = CARTESIAN_POINT ( 'NONE',  ( 115.6893214775786447, -9.859900752359374465, -12.68260735090039404 ) ) ;
#9334 = DIRECTION ( 'NONE',  ( -0.9908103287288504424, 0.1352586133457951423, 0.000000000000000000 ) ) ;
#9335 = CARTESIAN_POINT ( 'NONE',  ( 113.3068014775786594, -8.166667518702817929, -8.995218007635859436 ) ) ;
#9336 = ORIENTED_EDGE ( 'NONE', *, *, #1314, .F. ) ;
#9337 = CARTESIAN_POINT ( 'NONE',  ( 123.3474214775786209, -9.988377603198976828, -10.36322818467138340 ) ) ;
#9338 = FACE_OUTER_BOUND ( 'NONE', #4869, .T. ) ;
#9339 = FACE_OUTER_BOUND ( 'NONE', #35606, .T. ) ;
#9340 = CARTESIAN_POINT ( 'NONE',  ( 67.30914723170953096, -62.31448015807357166, -39.02309189069894302 ) ) ;
#9341 = CARTESIAN_POINT ( 'NONE',  ( 115.5758681442453053, -7.894159318335828068, -9.358103419637847864 ) ) ;
#9342 = CARTESIAN_POINT ( 'NONE',  ( 123.6270561621488184, -4.437987522111543015, -15.20954377567900373 ) ) ;
#9343 = CARTESIAN_POINT ( 'NONE',  ( 114.6115148109119986, -6.222761293078241884, -8.102969835052219238 ) ) ;
#9344 = CARTESIAN_POINT ( 'NONE',  ( 117.2294421295247844, 0.6306099254434621715, -12.14321520033831625 ) ) ;
#9345 = CARTESIAN_POINT ( 'NONE',  ( 125.3503171566262324, -2.572797884969513671, -20.07118512341956063 ) ) ;
#9346 = CARTESIAN_POINT ( 'NONE',  ( 115.8027748109119841, -8.899110576539710493, -16.42337572283490132 ) ) ;
#9347 = CARTESIAN_POINT ( 'NONE',  ( 114.4980614775786592, -7.893985811506177619, -18.51759400769804742 ) ) ;
#9348 = CARTESIAN_POINT ( 'NONE',  ( 122.1048610609119720, -6.340755971794695078, -8.611740276972781771 ) ) ;
#9349 = CARTESIAN_POINT ( 'NONE',  ( 126.6942948109119840, -8.899110576539710493, -16.42337572283490132 ) ) ;
#9350 = CARTESIAN_POINT ( 'NONE',  ( 114.7249681442453237, -9.565557343593413364, -10.61323700422348004 ) ) ;
#9351 = CARTESIAN_POINT ( 'NONE',  ( 124.5386814775786206, -5.638512984488999180, -18.83840828888717311 ) ) ;
#9352 = CARTESIAN_POINT ( 'NONE',  ( 122.2128881442453263, -1.834011780172310813, -8.268836392978581529 ) ) ;
#9353 = ORIENTED_EDGE ( 'NONE', *, *, #12252, .T. ) ;
#9354 = CARTESIAN_POINT ( 'NONE',  ( 112.9664414775786412, 0.5811942927096154232, -14.16772938898807155 ) ) ;
#9355 = CARTESIAN_POINT ( 'NONE',  ( 112.9828796295247884, -4.863998795839590272, -19.15521520033831493 ) ) ;
#9356 = CARTESIAN_POINT ( 'NONE',  ( 107.2182702545248105, 0.1403307496149616695, -11.32035403202665336 ) ) ;
#9357 = CARTESIAN_POINT ( 'NONE',  ( 110.6909265045248247, -2.791137627527939813, -8.388885654883777576 ) ) ;
#9358 = AXIS2_PLACEMENT_3D ( 'NONE', #8851, #8179, #43741 ) ;
#9359 = PRODUCT_DEFINITION ( 'UNKNOWN', '', #28600, #4596 ) ;
#9360 = CARTESIAN_POINT ( 'NONE',  ( -7.917624645353499524, -12.21642755857638818, -18.19321520033831519 ) ) ;
#9361 = CARTESIAN_POINT ( 'NONE',  ( 118.2987481442453088, -1.561330072975668504, -17.79121239304076951 ) ) ;
#9362 = EDGE_LOOP ( 'NONE', ( #1393, #19446, #15235, #2423, #21861, #29572 ) ) ;
#9363 = LINE ( 'NONE', #37153, #16540 ) ;
#9364 = CARTESIAN_POINT ( 'NONE',  ( 114.3278814775786429, 0.1319031606808879209, -14.10382304977623669 ) ) ;
#9365 = CARTESIAN_POINT ( 'NONE',  ( 106.5237390045248418, -9.868328341294098749, -11.32035403202665869 ) ) ;
#9366 = CARTESIAN_POINT ( 'NONE',  ( 118.2987481442453088, -1.561330072975668504, -17.79121239304076951 ) ) ;
#9367 = CARTESIAN_POINT ( 'NONE',  ( 107.6349890045248401, 0.8980012041604421569, -15.77991374673208469 ) ) ;
#9368 = DIRECTION ( 'NONE',  ( 1.000000000000000000, 0.000000000000000000, 0.000000000000000000 ) ) ;
#9369 = ORIENTED_EDGE ( 'NONE', *, *, #22760, .T. ) ;
#9370 = CARTESIAN_POINT ( 'NONE',  ( 110.6196051332721879, 0.2334052082820642360, -14.64321520033831447 ) ) ;
#9371 = CARTESIAN_POINT ( 'NONE',  ( 121.8725281442453223, -6.222761293078241884, -8.102969835052219238 ) ) ;
#9372 = CARTESIAN_POINT ( 'NONE',  ( 121.4754414775786131, -8.166667518702819706, -8.995218007635861213 ) ) ;
#9373 = CARTESIAN_POINT ( 'NONE',  ( 113.3068014775786594, -1.833838273342658809, -17.42832698103878286 ) ) ;
#9374 = CARTESIAN_POINT ( 'NONE',  ( 114.1577014775786552, -6.344957434206662583, -7.627207830600332805 ) ) ;
#9375 = CARTESIAN_POINT ( 'NONE',  ( 118.2005203923315548, -1.063912429576147511, -17.20460841810472985 ) ) ;
#9376 = CARTESIAN_POINT ( 'NONE',  ( 125.7866681442452688, -8.899110576539710493, -16.42337572283490132 ) ) ;
#9377 = CARTESIAN_POINT ( 'NONE',  ( 119.4900081442453086, -7.643976991954077427, -18.09477374809248928 ) ) ;
#9378 = ORIENTED_EDGE ( 'NONE', *, *, #19023, .T. ) ;
#9379 = CARTESIAN_POINT ( 'NONE',  ( 119.5467348109119712, -4.089484607189483256, -7.948022111789462052 ) ) ;
#9380 = CARTESIAN_POINT ( 'NONE',  ( 113.2500748109119968, -6.344957434206662583, -7.627207830600332805 ) ) ;
#9381 = CARTESIAN_POINT ( 'NONE',  ( 122.2696148109119889, -5.574606645277164318, -18.38911715685844683 ) ) ;
#9382 = VERTEX_POINT ( 'NONE', #13647 ) ;
#9383 = CARTESIAN_POINT ( 'NONE',  ( 123.4244704359119709, -10.25716656981731489, -12.88942061488890545 ) ) ;
#9384 = CARTESIAN_POINT ( 'NONE',  ( 117.2776681442452968, -5.638512984488999180, -18.83840828888717311 ) ) ;
#9385 = CARTESIAN_POINT ( 'NONE',  ( 114.3719421295247827, 0.8980012041604618078, -13.39321520033831447 ) ) ;
#9386 = CARTESIAN_POINT ( 'NONE',  ( 117.1074881442453233, 0.4262465694468514643, -12.03445270309931736 ) ) ;
#9387 = ORIENTED_EDGE ( 'NONE', *, *, #4676, .T. ) ;
#9388 = ORIENTED_EDGE ( 'NONE', *, *, #33755, .T. ) ;
#9389 = CARTESIAN_POINT ( 'NONE',  ( 111.8319081442453182, -5.638512984488999180, -18.83840828888717311 ) ) ;
#9390 = B_SPLINE_CURVE_WITH_KNOTS ( 'NONE', 3,
 ( #20034, #6117, #33916, #27554, #3151, #37343, #24133, #41466, #13859, #6572, #20710, #30964, #12974, #2687, #6348, #23458, #33690, #41249, #10448, #19802, #41022, #38025, #6801, #20262 ),
 .UNSPECIFIED., .F., .F.,
 ( 4, 2, 2, 1, 1, 1, 2, 2, 2, 1, 1, 1, 2, 2, 4 ),
 ( 0.000000000000000000, 0.2499999999999916178, 0.3749999999999865663, 0.4374999999999830136, 0.4687499999999789058, 0.4843749999999755196, 0.4921874999999747979, 0.4999999999999740208, 0.6249999999999837907, 0.6874999999999900080, 0.7187499999999965583, 0.7343749999999972244, 0.7421874999999965583, 0.7499999999999957812, 1.000000000000000000 ),
 .UNSPECIFIED. ) ;
#9391 = CARTESIAN_POINT ( 'NONE',  ( 122.0994348109119443, -10.15424416112533912, -14.75197769757731336 ) ) ;
#9392 = DIRECTION ( 'NONE',  ( 1.000000000000000000, 1.131967377815149893E-16, 4.676795828538290169E-17 ) ) ;
#9393 = ORIENTED_EDGE ( 'NONE', *, *, #21448, .F. ) ;
#9394 = CARTESIAN_POINT ( 'NONE',  ( 118.4122014775786340, 0.5811942927096110934, -14.16772938898807510 ) ) ;
#9395 = CARTESIAN_POINT ( 'NONE',  ( 106.5237390045248418, 0.8980012041604421569, -15.77991374673208469 ) ) ;
#9396 = CARTESIAN_POINT ( 'NONE',  ( 120.3976348109119812, -1.834011780172310813, -8.268836392978581529 ) ) ;
#9398 = CARTESIAN_POINT ( 'NONE',  ( 120.6245414775786458, -0.1624402480850797581, -16.17319339645315424 ) ) ;
#9397 = CARTESIAN_POINT ( 'NONE',  ( 113.4769814775786330, -10.63000616557722466, -14.87417383870573495 ) ) ;
#9399 = FACE_OUTER_BOUND ( 'NONE', #21695, .T. ) ;
#9400 = CARTESIAN_POINT ( 'NONE',  ( 111.8319081442453182, -5.638512984488999180, -18.83840828888717311 ) ) ;
#9401 = EDGE_CURVE ( 'NONE', #21122, #28482, #9390, .T. ) ;
#9402 = ORIENTED_EDGE ( 'NONE', *, *, #38682, .T. ) ;
#9403 = CARTESIAN_POINT ( 'NONE',  ( 124.4252281442452812, -0.8288870151387760510, -10.36305467784173118 ) ) ;
#9404 = CARTESIAN_POINT ( 'NONE',  ( 123.5743281442453139, -7.893985811506158079, -18.51759400769805453 ) ) ;
#9405 = LINE ( 'NONE', #16025, #32919 ) ;
#9406 = CARTESIAN_POINT ( 'NONE',  ( 112.8439733795247832, -8.938348069036489818, -17.46756447353520159 ) ) ;
#9407 = CARTESIAN_POINT ( 'NONE',  ( 113.7468640045248236, 0.1403307496149616695, -15.46607636864997204 ) ) ;
#9408 = CARTESIAN_POINT ( 'NONE',  ( 111.5243640045248412, -10.62599879583958717, -11.00651665394454604 ) ) ;
#9409 = CARTESIAN_POINT ( 'NONE',  ( 122.6667014775786413, -7.893985811506177619, -18.51759400769804742 ) ) ;
#9410 = CARTESIAN_POINT ( 'NONE',  ( 121.9292548109119849, -7.894159318335828068, -9.358103419637847864 ) ) ;
#9411 = ORIENTED_EDGE ( 'NONE', *, *, #2440, .F. ) ;
#9412 = CARTESIAN_POINT ( 'NONE',  ( 119.8870948109119752, -9.261995988541697145, -16.69588392320189030 ) ) ;
#9413 = CARTESIAN_POINT ( 'NONE',  ( 112.9664414775786412, -9.859900752359374465, -12.68260735090039404 ) ) ;
#9414 = CARTESIAN_POINT ( 'NONE',  ( 119.7736414775786358, -10.30919188438810075, -12.61870101168855918 ) ) ;
#9415 = CARTESIAN_POINT ( 'NONE',  ( 120.1707281442453166, 0.2603800115204892296, -16.42320221600525088 ) ) ;
#9416 = CARTESIAN_POINT ( 'NONE',  ( 63.37404594698951854, -3.173945195454633605, -19.03816892419136764 ) ) ;
#9417 = CARTESIAN_POINT ( 'NONE',  ( 125.7299414775786346, -10.15424416112533912, -14.75197769757731336 ) ) ;
#9418 = DIRECTION ( 'NONE',  ( 1.000000000000000000, 0.000000000000000000, -0.000000000000000000 ) ) ;
#9419 = CARTESIAN_POINT ( 'NONE',  ( 123.1466579359119891, -4.360204210389833968, -8.000047426360245240 ) ) ;
#9420 = ORIENTED_EDGE ( 'NONE', *, *, #40344, .T. ) ;
#9421 = CARTESIAN_POINT ( 'NONE',  ( 121.9470836909669913, -24.14644159042263993, -12.62951656296512937 ) ) ;
#9422 = DIRECTION ( 'NONE',  ( 0.5040994586965589219, 0.8636456077245088236, 0.000000000000000000 ) ) ;
#9423 = CARTESIAN_POINT ( 'NONE',  ( 124.8223148109119762, -10.15424416112533912, -14.75197769757731336 ) ) ;
#9424 = CARTESIAN_POINT ( 'NONE',  ( 107.2877233795247776, -1.325403438956436419, -9.854619843455211026 ) ) ;
#9425 = CARTESIAN_POINT ( 'NONE',  ( 111.3160046295247838, -4.863998795839590272, -18.39754474579285315 ) ) ;
#9427 = VECTOR ( 'NONE', #39972, 1000.000000000000114 ) ;
#9426 = CARTESIAN_POINT ( 'NONE',  ( 117.7314814775786260, -5.574606645277164318, -18.38911715685844683 ) ) ;
#9428 = CARTESIAN_POINT ( 'NONE',  ( 70.04692138463070705, -26.21798220612133434, -5.722398249991135444 ) ) ;
#9429 = CARTESIAN_POINT ( 'NONE',  ( 117.1642148109119859, -0.8288870151387760510, -10.36305467784173118 ) ) ;
#9430 = CARTESIAN_POINT ( 'NONE',  ( 123.5743281442453139, -7.893985811506177619, -18.51759400769804742 ) ) ;
#9431 = VERTEX_POINT ( 'NONE', #16384 ) ;
#9432 = EDGE_CURVE ( 'NONE', #18453, #20584, #11573, .T. ) ;
#9433 = CARTESIAN_POINT ( 'NONE',  ( 121.9292548109119849, -7.894159318335828068, -9.358103419637847864 ) ) ;
#9434 = CARTESIAN_POINT ( 'NONE',  ( 117.8449348109119938, -8.166667518702817929, -8.995218007635861213 ) ) ;
#9435 = CARTESIAN_POINT ( 'NONE',  ( 124.6521348109119884, -1.561330072975668948, -17.79121239304076951 ) ) ;
#9436 = CARTESIAN_POINT ( 'NONE',  ( 122.1561614775786353, -8.899110576539710493, -16.42337572283490132 ) ) ;
#9437 = ORIENTED_EDGE ( 'NONE', *, *, #38993, .T. ) ;
#9438 = FACE_OUTER_BOUND ( 'NONE', #32639, .T. ) ;
#9439 = EDGE_CURVE ( 'NONE', #873, #23361, #44212, .T. ) ;
#9440 = EDGE_CURVE ( 'NONE', #25300, #12207, #21778, .T. ) ;
#9441 = CARTESIAN_POINT ( 'NONE',  ( 124.5386814775786206, -5.638512984488999180, -18.83840828888717311 ) ) ;
#9442 = CARTESIAN_POINT ( 'NONE',  ( 115.6325948109119821, -9.565557343593413364, -10.61323700422348004 ) ) ;
#9443 = CARTESIAN_POINT ( 'NONE',  ( 125.1626748109119802, -9.988377603198980381, -10.36322818467138518 ) ) ;
#9444 = CARTESIAN_POINT ( 'NONE',  ( 107.7738952545248310, 0.8980012041604421569, -11.00651665394454071 ) ) ;
#9445 = DIRECTION ( 'NONE',  ( 0.9908103287288495542, -0.1352586133458027196, 0.000000000000000000 ) ) ;
#9446 = ORIENTED_EDGE ( 'NONE', *, *, #34328, .F. ) ;
#9447 = ADVANCED_FACE ( 'NONE', ( #45102 ), #3553, .T. ) ;
#9448 = CARTESIAN_POINT ( 'NONE',  ( 59.62174278132245320, -14.86814543204979344, -7.393215200338313586 ) ) ;
#9449 = CARTESIAN_POINT ( 'NONE',  ( 108.4684265045247997, -2.791137627527939813, -8.388885654883777576 ) ) ;
#9450 = AXIS2_PLACEMENT_3D ( 'NONE', #6883, #42215, #38324 ) ;
#9451 = DIRECTION ( 'NONE',  ( 1.000000000000000000, 0.000000000000000000, 0.000000000000000000 ) ) ;
#9452 = EDGE_CURVE ( 'NONE', #26347, #32179, #14447, .T. ) ;
#9453 = CARTESIAN_POINT ( 'NONE',  ( 121.0783548109119749, -9.565557343593413364, -10.61323700422348004 ) ) ;
#9454 = CARTESIAN_POINT ( 'NONE',  ( 115.6893214775786447, -9.859900752359374465, -12.68260735090039404 ) ) ;
#9455 = CARTESIAN_POINT ( 'NONE',  ( 125.6732148109119862, -9.859900752359370912, -12.68260735090036562 ) ) ;
#9456 = EDGE_CURVE ( 'NONE', #23894, #3386, #7680, .T. ) ;
#9457 = ADVANCED_FACE ( 'NONE', ( #31849 ), #31254, .F. ) ;
#9458 = ORIENTED_EDGE ( 'NONE', *, *, #7188, .T. ) ;
#9459 = DIRECTION ( 'NONE',  ( 0.9609149988134837450, -0.1028163501681639419, 0.2570431154366518145 ) ) ;
#9460 = CARTESIAN_POINT ( 'NONE',  ( 120.7947214775786193, -0.8288870151387760510, -10.36305467784173118 ) ) ;
#9461 = CARTESIAN_POINT ( 'NONE',  ( 112.6260814775786514, -0.8288870151387760510, -10.36305467784173118 ) ) ;
#9462 = CIRCLE ( 'NONE', #21215, 2.000000000000000444 ) ;
#9463 = CARTESIAN_POINT ( 'NONE',  ( 67.69189222814998175, -59.27884951796255564, -42.87418841894956500 ) ) ;
#9464 = CARTESIAN_POINT ( 'NONE',  ( 111.2184548109119788, -8.862178061932382889, -16.39564131203247399 ) ) ;
#9466 = CARTESIAN_POINT ( 'NONE',  ( 122.2128881442453263, -1.834011780172310813, -8.268836392978581529 ) ) ;
#9465 = DIRECTION ( 'NONE',  ( 1.000000000000000000, 0.000000000000000000, 0.000000000000000000 ) ) ;
#9467 = CARTESIAN_POINT ( 'NONE',  ( 112.9664414775786412, 0.5811942927096154232, -14.16772938898807155 ) ) ;
#9468 = ORIENTED_EDGE ( 'NONE', *, *, #8072, .F. ) ;
#9469 = CONICAL_SURFACE ( 'NONE', #731, 2.445500000000004448, 0.9599310885968757034 ) ;
#9470 = PLANE ( 'NONE',  #42821 ) ;
#9471 = CARTESIAN_POINT ( 'NONE',  ( 113.4725659692789748, -1.179503403430478770, -17.05068175419387799 ) ) ;
#9472 = CARTESIAN_POINT ( 'NONE',  ( 106.9404577545248145, -2.791137627527939813, -18.39754474579286025 ) ) ;
#9473 = CARTESIAN_POINT ( 'NONE',  ( 124.1415948109119540, -3.505236298600246325, -18.68346056562440793 ) ) ;
#9474 = CARTESIAN_POINT ( 'NONE',  ( 118.7525614775786380, -1.833838273342659253, -17.42832698103878286 ) ) ;
#9475 = FACE_OUTER_BOUND ( 'NONE', #24147, .T. ) ;
#9476 = CARTESIAN_POINT ( 'NONE',  ( 112.3578015045248861, -6.936859964151250502, -18.39754474579286025 ) ) ;
#9477 = CARTESIAN_POINT ( 'NONE',  ( 89.67401078471493747, -25.23119213852205789, -15.24166438581092109 ) ) ;
#9478 = CARTESIAN_POINT ( 'NONE',  ( 59.69399050597296252, -13.58096788970641811, -8.603412892520118760 ) ) ;
#9479 = CARTESIAN_POINT ( 'NONE',  ( 113.5904348109119866, -2.084020599724406786, -8.691656652584148546 ) ) ;
#9480 = CARTESIAN_POINT ( 'NONE',  ( 111.5243640045248412, -10.62599879583958717, -11.00651665394454604 ) ) ;
#9481 = CARTESIAN_POINT ( 'NONE',  ( 111.9410827545248708, -2.477300249445798297, -19.15521520033831138 ) ) ;
#9482 = CARTESIAN_POINT ( 'NONE',  ( 123.2906948109119867, -8.166667518702819706, -8.995218007635861213 ) ) ;
#9483 = CARTESIAN_POINT ( 'NONE',  ( 122.3830681442452857, -8.166667518702819706, -8.995218007635861213 ) ) ;
#9484 = DIRECTION ( 'NONE',  ( 0.9609149988134837450, -0.1028163501681639419, 0.2570431154366518145 ) ) ;
#9485 = CARTESIAN_POINT ( 'NONE',  ( 118.4122014775786340, 0.5811942927096110934, -14.16772938898807510 ) ) ;
#9486 = CARTESIAN_POINT ( 'NONE',  ( 113.2500748109119968, -6.344957434206662583, -7.627207830600332805 ) ) ;
#9487 = ORIENTED_EDGE ( 'NONE', *, *, #12819, .T. ) ;
#9488 = CARTESIAN_POINT ( 'NONE',  ( 113.8173414775786512, -9.565557343593413364, -10.61323700422348004 ) ) ;
#9489 = CARTESIAN_POINT ( 'NONE',  ( 125.7866681442452688, -0.4660016031367893996, -10.09054647747474043 ) ) ;
#9490 = CARTESIAN_POINT ( 'NONE',  ( 121.3619881442452879, -4.089484607189486809, -7.948022111789456723 ) ) ;
#9491 = CIRCLE ( 'NONE', #16029, 1.009117809157100254 ) ;
#9492 = CARTESIAN_POINT ( 'NONE',  ( 114.8384214775786489, 0.9020085738987339008, -11.91225656197089222 ) ) ;
#9493 = ITEM_DEFINED_TRANSFORMATION ( 'NONE', 'NONE', #24253,  #12375 ) ;
#9494 = CARTESIAN_POINT ( 'NONE',  ( 113.6471614775786492, -4.153390946401321671, -8.397313243818183892 ) ) ;
#9495 = ORIENTED_EDGE ( 'NONE', *, *, #14542, .T. ) ;
#9496 = CARTESIAN_POINT ( 'NONE',  ( 116.0864081442453113, -0.1624402480850797581, -16.17319339645315424 ) ) ;
#9497 = CARTESIAN_POINT ( 'NONE',  ( 113.6471614775786492, -4.153390946401321671, -8.397313243818183892 ) ) ;
#9498 = CARTESIAN_POINT ( 'NONE',  ( 108.3295202545248657, -10.62599879583958717, -15.77991374673208469 ) ) ;
#9499 = VECTOR ( 'NONE', #39899, 1000.000000000000000 ) ;
#9500 = CARTESIAN_POINT ( 'NONE',  ( 109.7880358795247986, -8.402594152722688392, -9.854619843455216355 ) ) ;
#9501 = CARTESIAN_POINT ( 'NONE',  ( 124.0848681442452772, -5.574606645277164318, -18.38911715685844683 ) ) ;
#9502 = CARTESIAN_POINT ( 'NONE',  ( 116.8928740015602870, 0.2848729546123598966, -14.64321520033831447 ) ) ;
#9503 = CARTESIAN_POINT ( 'NONE',  ( 75.95778847736481509, -3.256761025687722189, -18.79321520033831661 ) ) ;
#9504 = ORIENTED_EDGE ( 'NONE', *, *, #37847, .F. ) ;
#9505 = CARTESIAN_POINT ( 'NONE',  ( 123.4939235609119663, -9.645473719204776586, -14.86997237629376656 ) ) ;
#9506 = CARTESIAN_POINT ( 'NONE',  ( 124.7655881442452852, 0.5811942927096110934, -14.16772938898807510 ) ) ;
#9507 = CARTESIAN_POINT ( 'NONE',  ( 113.4690515045247992, -6.936859964151197211, -18.39754474579287447 ) ) ;
#9508 = CARTESIAN_POINT ( 'NONE',  ( 111.7184548109119788, -9.261995988541697145, -16.69588392320189030 ) ) ;
#9509 = CARTESIAN_POINT ( 'NONE',  ( 116.6786527946934768, 2.098153082867008745, -6.056648293417564055 ) ) ;
#9510 = DIRECTION ( 'NONE',  ( 1.000000000000000000, 0.000000000000000000, -0.000000000000000000 ) ) ;
#9511 = CARTESIAN_POINT ( 'NONE',  ( 107.4960827545248350, -6.936859964151250502, -8.388885654883777576 ) ) ;
#9512 = CARTESIAN_POINT ( 'NONE',  ( 123.6071420163423085, -1.087735405160626723, -17.17288456429612964 ) ) ;
#9513 = CARTESIAN_POINT ( 'NONE',  ( 137.1322768238038350, -4.609925023091584251, -18.75211014789456598 ) ) ;
#9514 = DIRECTION ( 'NONE',  ( 0.000000000000000000, -0.9242245927363029745, -0.3818493186865927203 ) ) ;
#9515 = CARTESIAN_POINT ( 'NONE',  ( 124.4252281442452812, -9.261995988541697145, -16.69588392320189030 ) ) ;
#9516 = CARTESIAN_POINT ( 'NONE',  ( 120.4543614775786295, -5.574606645277164318, -18.38911715685844683 ) ) ;
#9517 = CARTESIAN_POINT ( 'NONE',  ( 119.7434548109119703, -0.2404488592019161652, -16.18068212994647226 ) ) ;
#9518 = ORIENTED_EDGE ( 'NONE', *, *, #6378, .T. ) ;
#9519 = CARTESIAN_POINT ( 'NONE',  ( 122.3263414775786373, -6.344957434206665248, -7.627207830600338134 ) ) ;
#9520 = EDGE_CURVE ( 'NONE', #22284, #43627, #18853, .T. ) ;
#9521 = CARTESIAN_POINT ( 'NONE',  ( 120.4543614775786295, -4.089484607189486809, -7.948022111789456723 ) ) ;
#9522 = CARTESIAN_POINT ( 'NONE',  ( 117.0806140045248185, 0.1403307496149616695, -15.46607636864997204 ) ) ;
#9523 = CARTESIAN_POINT ( 'NONE',  ( 113.5337081442453240, -0.8288870151387760510, -10.36305467784173118 ) ) ;
#9524 =( BOUNDED_CURVE ( )  B_SPLINE_CURVE ( 2, ( #31328, #14682, #547, #7608, #18329, #995, #6951, #24286, #31553, #35180, #42731, #28596, #35639, #102, #24943, #7159, #42507 ),
 .UNSPECIFIED., .F., .F. ) 
 B_SPLINE_CURVE_WITH_KNOTS ( ( 3, 2, 2, 2, 2, 2, 2, 2, 3 ),
 ( 0.1420046674808919940, 0.1484375000000000000, 0.1562500000000000000, 0.1640625000000000000, 0.1718750000000000000, 0.1796875000000000000, 0.1875000000000000000, 0.1953125000000000000, 0.2017453325190585178 ),
 .UNSPECIFIED. ) 
 CURVE ( )  GEOMETRIC_REPRESENTATION_ITEM ( )  RATIONAL_B_SPLINE_CURVE ( ( 0.9778625265006459788, 0.9373222120152210346, 1.000000000000000000, 0.9238795325112869605, 1.000000000000000000, 0.9238795325112869605, 1.000000000000000000, 0.9238795325112869605, 1.000000000000000000, 0.9238795325112869605, 1.000000000000000000, 0.9238795325112869605, 1.000000000000000000, 0.9238795325112869605, 1.000000000000000000, 0.9373222120157019832, 0.9778625265000240319 ) ) 
 REPRESENTATION_ITEM ( '' )  );
#9525 = CARTESIAN_POINT ( 'NONE',  ( 112.0020881442453344, 0.2603800115204892296, -16.42320221600525088 ) ) ;
#9526 = CARTESIAN_POINT ( 'NONE',  ( 123.6310548109119765, -5.638512984488999180, -18.83840828888717311 ) ) ;
#9527 = CARTESIAN_POINT ( 'NONE',  ( 111.6632702545248605, -10.62599879583958717, -15.77991374673208469 ) ) ;
#9528 = CARTESIAN_POINT ( 'NONE',  ( 107.4960827545248350, -6.936859964151250502, -8.388885654883777576 ) ) ;
#9529 = CARTESIAN_POINT ( 'NONE',  ( 83.49687201881269516, -32.20436853251904807, -23.72624644355049028 ) ) ;
#9530 = CARTESIAN_POINT ( 'NONE',  ( 116.4834948109119779, -7.894159318335828068, -9.358103419637847864 ) ) ;
#9531 = CIRCLE ( 'NONE', #17529, 2.000000000000000444 ) ;
#9532 = CARTESIAN_POINT ( 'NONE',  ( 118.0151148109119816, 0.4262465694468514643, -12.03445270309931736 ) ) ;
#9533 = CARTESIAN_POINT ( 'NONE',  ( 76.69189222814998175, -40.21211973637274184, -4.893215200338314474 ) ) ;
#9534 = CARTESIAN_POINT ( 'NONE',  ( 111.5938171295247940, 0.1403307496149613920, -13.39321520033831447 ) ) ;
#9535 = ORIENTED_EDGE ( 'NONE', *, *, #32802, .T. ) ;
#9536 = AXIS2_PLACEMENT_3D ( 'NONE', #30681, #6282, #20651 ) ;
#9537 = DIRECTION ( 'NONE',  ( 0.2768435750659235528, 0.3568721902840663041, -0.8921882507333145362 ) ) ;
#9538 = CARTESIAN_POINT ( 'NONE',  ( 112.0020881442453344, 0.2603800115204892296, -16.42320221600525088 ) ) ;
#9539 = CARTESIAN_POINT ( 'NONE',  ( 79.79010115959992788, 5.106172230548759572, -6.893215200338315363 ) ) ;
#9540 = CARTESIAN_POINT ( 'NONE',  ( 123.3550173109119612, 0.2312338769422704887, -16.08380026872395874 ) ) ;
#9541 = CARTESIAN_POINT ( 'NONE',  ( 121.8270485609119760, -0.08252387247370887580, -11.91645802438286417 ) ) ;
#9542 = ORIENTED_EDGE ( 'NONE', *, *, #42709, .T. ) ;
#9543 = CARTESIAN_POINT ( 'NONE',  ( 114.1635827545248247, -2.477300249445798297, -19.15521520033830427 ) ) ;
#9544 = CARTESIAN_POINT ( 'NONE',  ( 111.5045738707033536, -1.272620149025138092, -16.92668288537504750 ) ) ;
#9545 = ORIENTED_EDGE ( 'NONE', *, *, #25043, .F. ) ;
#9546 = CARTESIAN_POINT ( 'NONE',  ( 118.9794681442453026, -9.261995988541697145, -16.69588392320189030 ) ) ;
#9547 = CARTESIAN_POINT ( 'NONE',  ( 125.9568481442452850, -3.505236298600246325, -18.68346056562440793 ) ) ;
#9548 = CARTESIAN_POINT ( 'NONE',  ( 118.0718414775786442, -0.8288870151387760510, -10.36305467784173118 ) ) ;
#9549 = FACE_OUTER_BOUND ( 'NONE', #30433, .T. ) ;
#9550 = CARTESIAN_POINT ( 'NONE',  ( 122.0994348109119443, 0.9020085738987339008, -11.91225656197089222 ) ) ;
#9551 = CARTESIAN_POINT ( 'NONE',  ( 113.7038881442453402, -3.383040157471821630, -19.15922257007629170 ) ) ;
#9552 = CARTESIAN_POINT ( 'NONE',  ( 111.1076452545248259, -9.868328341294098749, -15.46607636864997204 ) ) ;
#9553 = AXIS2_PLACEMENT_3D ( 'NONE', #29824, #36872, #26406 ) ;
#9554 = CARTESIAN_POINT ( 'NONE',  ( 125.1059481442452750, -8.166667518702819706, -8.995218007635861213 ) ) ;
#9555 = B_SPLINE_CURVE_WITH_KNOTS ( 'NONE', 3,
 ( #22462, #36494, #37159, #30343, #5480, #15987, #19858, #43576, #39929, #40610 ),
 .UNSPECIFIED., .F., .F.,
 ( 4, 3, 3, 4 ),
 ( 0.000000000000000000, 0.0001671877560958114864, 0.0003343755126086594954, 0.0006438490228507209303 ),
 .UNSPECIFIED. ) ;
#9556 = CARTESIAN_POINT ( 'NONE',  ( 112.6609831777918913, -0.01829820670813664396, -14.64321520033831447 ) ) ;
#9557 = ORIENTED_EDGE ( 'NONE', *, *, #11734, .F. ) ;
#9558 = CARTESIAN_POINT ( 'NONE',  ( 119.7169148109119874, -9.988377603198976828, -10.36322818467138340 ) ) ;
#9559 = CARTESIAN_POINT ( 'NONE',  ( 115.8027748109119841, -8.899110576539710493, -16.42337572283490132 ) ) ;
#9560 = CARTESIAN_POINT ( 'NONE',  ( 126.9115046738230319, -4.631886270669566485, -18.73501732256985619 ) ) ;
#9561 = CARTESIAN_POINT ( 'NONE',  ( 112.3991748109119868, -8.166667518702817929, -8.995218007635859436 ) ) ;
#9562 = ORIENTED_EDGE ( 'NONE', *, *, #23937, .F. ) ;
#9563 = AXIS2_PLACEMENT_3D ( 'NONE', #17482, #44869, #14065 ) ;
#9564 = CARTESIAN_POINT ( 'NONE',  ( 120.7379948109119709, -10.63000616557722466, -14.87417383870573495 ) ) ;
#9565 = CARTESIAN_POINT ( 'NONE',  ( 76.69189222814998175, -46.76310523276723785, -4.893215200338314474 ) ) ;
#9566 = CARTESIAN_POINT ( 'NONE',  ( 109.9963952545248134, -9.868328341294102302, -15.46607636865003244 ) ) ;
#9567 = CARTESIAN_POINT ( 'NONE',  ( 71.02242295334774269, -99.02728775972636299, -55.91838671430374319 ) ) ;
#9568 = PLANE ( 'NONE',  #33211 ) ;
#9569 = CARTESIAN_POINT ( 'NONE',  ( 115.6325948109119821, -9.565557343593413364, -10.61323700422348004 ) ) ;
#9570 = CARTESIAN_POINT ( 'NONE',  ( 112.4174607241439361, -2.443475742715324639, -17.86549347949428679 ) ) ;
#9571 = CARTESIAN_POINT ( 'NONE',  ( 116.3700414775786527, -4.153390946401321671, -8.397313243818183892 ) ) ;
#9572 = CARTESIAN_POINT ( 'NONE',  ( 113.1912390045248031, -9.868328341294098749, -11.32035403202665869 ) ) ;
#9573 = EDGE_CURVE ( 'NONE', #14657, #35146, #13085, .T. ) ;
#9574 = DIRECTION ( 'NONE',  ( 0.000000000000000000, -1.000000000000000000, 0.000000000000000000 ) ) ;
#9575 = CARTESIAN_POINT ( 'NONE',  ( 114.3846081442453197, 0.4262465694468514643, -12.03445270309931736 ) ) ;
#9576 = CARTESIAN_POINT ( 'NONE',  ( 116.0864081442453113, -9.988377603198976828, -10.36322818467138340 ) ) ;
#9577 = CARTESIAN_POINT ( 'NONE',  ( 124.7440798109119697, -7.200787124940443817, -17.81845355600750835 ) ) ;
#9578 = CARTESIAN_POINT ( 'NONE',  ( 112.6828081442453282, -7.893985811506177619, -18.51759400769804742 ) ) ;
#9579 = CARTESIAN_POINT ( 'NONE',  ( 117.0507614775786465, 0.1319031606808879209, -14.10382304977623669 ) ) ;
#9580 = CARTESIAN_POINT ( 'NONE',  ( 125.1059481442452750, -8.166667518702819706, -8.995218007635861213 ) ) ;
#9581 = CARTESIAN_POINT ( 'NONE',  ( 118.1852948109119836, -4.153390946401325223, -8.397313243818185668 ) ) ;
#9582 = VERTEX_POINT ( 'NONE', #17727 ) ;
#9583 = CARTESIAN_POINT ( 'NONE',  ( 113.4769814775786330, -10.63000616557722466, -14.87417383870573495 ) ) ;
#9584 = CARTESIAN_POINT ( 'NONE',  ( 112.5661608795247872, -8.938348069036489818, -9.318865927141430916 ) ) ;
#9585 = CARTESIAN_POINT ( 'NONE',  ( 106.7320983795247855, -8.402594152722688392, -16.93181055722141792 ) ) ;
#9586 = CARTESIAN_POINT ( 'NONE',  ( 105.0652233795248378, -1.325403438956436419, -9.854619843455211026 ) ) ;
#9587 = CIRCLE ( 'NONE', #3743, 1.499999999999996225 ) ;
#9588 = CARTESIAN_POINT ( 'NONE',  ( 64.44034106609326784, -36.97598037384660330, -5.426085069519624327 ) ) ;
#9589 = CARTESIAN_POINT ( 'NONE',  ( 119.6034614775786196, -6.344957434206665248, -7.627207830600338134 ) ) ;
#9590 = EDGE_LOOP ( 'NONE', ( #9737, #20621, #9848, #29851, #3163, #31551, #40147, #7819 ) ) ;
#9591 = CARTESIAN_POINT ( 'NONE',  ( 125.7299414775786346, 0.9020085738987339008, -11.91225656197089222 ) ) ;
#9592 = CARTESIAN_POINT ( 'NONE',  ( 124.7655881442452852, 0.5811942927096102052, -14.16772938898805556 ) ) ;
#9593 = CARTESIAN_POINT ( 'NONE',  ( 115.7460481442453357, -10.15424416112533912, -14.75197769757731336 ) ) ;
#9594 = CARTESIAN_POINT ( 'NONE',  ( 123.4244704359119709, 1.345710702986147034, -13.97328579221134603 ) ) ;
#9595 = CARTESIAN_POINT ( 'NONE',  ( 123.8012348109119642, 0.2603800115204892296, -16.42320221600525088 ) ) ;
#9596 = CARTESIAN_POINT ( 'NONE',  ( 107.4960827545248350, -2.477300249445798297, -19.15521520033831138 ) ) ;
#9597 = DIRECTION ( 'NONE',  ( -1.000000000000000000, 1.214306433183763980E-15, 0.000000000000000000 ) ) ;
#9598 = ORIENTED_EDGE ( 'NONE', *, *, #34790, .F. ) ;
#9599 = VECTOR ( 'NONE', #28548, 1000.000000000000000 ) ;
#9600 = CARTESIAN_POINT ( 'NONE',  ( 123.6877814775786533, -6.222761293078241884, -8.102969835052219238 ) ) ;
#9601 = CARTESIAN_POINT ( 'NONE',  ( 121.5321681442453183, -9.988377603198976828, -10.36322818467138340 ) ) ;
#9602 = EDGE_CURVE ( 'NONE', #9608, #18186, #28225, .T. ) ;
#9603 = CARTESIAN_POINT ( 'NONE',  ( 112.5126281442453120, 0.1319031606808879209, -14.10382304977623669 ) ) ;
#9604 = CARTESIAN_POINT ( 'NONE',  ( 116.2565881442452991, -9.261995988541697145, -16.69588392320189030 ) ) ;
#9605 = CARTESIAN_POINT ( 'NONE',  ( 61.41452964936473791, -3.848961180437260321, -19.39321520033831447 ) ) ;
#9606 = CARTESIAN_POINT ( 'NONE',  ( 128.2184548109119930, -1.191816558809784876, -8.648209655763537285 ) ) ;
#9607 = CARTESIAN_POINT ( 'NONE',  ( 118.2420214775786320, -6.222761293078241884, -8.102969835052219238 ) ) ;
#9608 = VERTEX_POINT ( 'NONE', #21595 ) ;
#9609 = CARTESIAN_POINT ( 'NONE',  ( 122.1743141859119817, -0.8832429491016019485, -18.19431474523657855 ) ) ;
#9610 = CARTESIAN_POINT ( 'NONE',  ( 114.7816948109119863, 0.5811942927096154232, -14.16772938898807155 ) ) ;
#9611 = CARTESIAN_POINT ( 'NONE',  ( 121.9859814775786333, -9.565557343593413364, -10.61323700422348004 ) ) ;
#9612 = ORIENTED_EDGE ( 'NONE', *, *, #21962, .T. ) ;
#9613 = CARTESIAN_POINT ( 'NONE',  ( 123.4939235609119663, -9.645473719204776586, -14.86997237629376656 ) ) ;
#9614 = CARTESIAN_POINT ( 'NONE',  ( 137.4945747549916462, -0.6989084441936219694, -10.59149681938009380 ) ) ;
#9615 = CARTESIAN_POINT ( 'NONE',  ( 118.5256548109119876, -0.4660016031367893996, -10.09054647747474043 ) ) ;
#9616 = CARTESIAN_POINT ( 'NONE',  ( 111.6632702545248605, -10.62599879583958717, -15.77991374673208469 ) ) ;
#9617 = CARTESIAN_POINT ( 'NONE',  ( 115.0086014775786509, -5.574606645277164318, -18.38911715685844683 ) ) ;
#9618 = EDGE_LOOP ( 'NONE', ( #44476, #32317, #14413, #27307, #14116, #1101 ) ) ;
#9619 = ORIENTED_EDGE ( 'NONE', *, *, #36161, .T. ) ;
#9620 = VECTOR ( 'NONE', #27895, 1000.000000000000114 ) ;
#9621 = CARTESIAN_POINT ( 'NONE',  ( 125.9568481442452850, -3.505236298600246325, -18.68346056562440793 ) ) ;
#9622 = CARTESIAN_POINT ( 'NONE',  ( 119.5467348109119712, -5.574606645277164318, -18.38911715685844683 ) ) ;
#9623 = FACE_OUTER_BOUND ( 'NONE', #21419, .T. ) ;
#9624 = CARTESIAN_POINT ( 'NONE',  ( 120.3976348109119812, -1.834011780172310813, -8.268836392978581529 ) ) ;
#9625 = CARTESIAN_POINT ( 'NONE',  ( 108.8851452545248151, 0.8980012041604421569, -11.00651665394454071 ) ) ;
#9626 = VECTOR ( 'NONE', #4068, 1000.000000000000114 ) ;
#9627 = CARTESIAN_POINT ( 'NONE',  ( 119.7169148109119874, -9.988377603198976828, -10.36322818467138340 ) ) ;
#9629 = CARTESIAN_POINT ( 'NONE',  ( 120.2841814775786276, -10.15424416112533912, -14.75197769757731336 ) ) ;
#9628 = CARTESIAN_POINT ( 'NONE',  ( 117.2209414775786485, -7.893985811506177619, -18.51759400769804742 ) ) ;
#9630 = CARTESIAN_POINT ( 'NONE',  ( 125.7299414775786346, -10.15424416112533912, -14.75197769757731336 ) ) ;
#9631 = CARTESIAN_POINT ( 'NONE',  ( 112.3416152477524008, -1.220279397241704755, -16.99638242193885418 ) ) ;
#9632 = B_SPLINE_CURVE_WITH_KNOTS ( 'NONE', 3,
 ( #28526, #36241, #32813, #18705, #14607, #31923, #4785, #18254, #5007, #11195 ),
 .UNSPECIFIED., .F., .F.,
 ( 4, 3, 3, 4 ),
 ( 0.000000000000000000, 1.701546542203775152E-05, 3.403093084406119836E-05, 6.582972837196840747E-05 ),
 .UNSPECIFIED. ) ;
#9633 = ORIENTED_EDGE ( 'NONE', *, *, #10295, .F. ) ;
#9634 = CARTESIAN_POINT ( 'NONE',  ( 123.1772414775786189, -5.574606645277164318, -18.38911715685844683 ) ) ;
#9635 = DIRECTION ( 'NONE',  ( 1.000000000000000000, 0.000000000000000000, 0.000000000000000000 ) ) ;
#9636 = CARTESIAN_POINT ( 'NONE',  ( 86.36631847702263087, -27.84333996136784961, -14.15691383771150136 ) ) ;
#9637 = CARTESIAN_POINT ( 'NONE',  ( 106.8710046295248759, -4.863998795839590272, -7.631215200338315796 ) ) ;
#9638 = CARTESIAN_POINT ( 'NONE',  ( 113.1217858795247935, -8.402594152722688392, -9.854619843455216355 ) ) ;
#9639 = CARTESIAN_POINT ( 'NONE',  ( 108.6073327545248048, -2.477300249445798297, -19.15521520033831138 ) ) ;
#9640 = CARTESIAN_POINT ( 'NONE',  ( 123.4041481442452834, -10.30919188438810075, -12.61870101168855918 ) ) ;
#9641 = CARTESIAN_POINT ( 'NONE',  ( 122.8368814775786291, -7.894159318335828068, -9.358103419637847864 ) ) ;
#9642 = ORIENTED_EDGE ( 'NONE', *, *, #18470, .T. ) ;
#9643 = CARTESIAN_POINT ( 'NONE',  ( 123.9146881442452894, 0.9020085738987339008, -11.91225656197089222 ) ) ;
#9644 = CARTESIAN_POINT ( 'NONE',  ( 113.5337081442453240, -0.8288870151387760510, -10.36305467784173118 ) ) ;
#9645 = CYLINDRICAL_SURFACE ( 'NONE', #40918, 2.000000000000000000 ) ;
#9646 = CARTESIAN_POINT ( 'NONE',  ( 119.2063748109119814, -1.561330072975668504, -17.79121239304076951 ) ) ;
#9647 = CARTESIAN_POINT ( 'NONE',  ( 122.8936081442453059, 0.2603800115204892296, -16.42320221600525088 ) ) ;
#9648 = CARTESIAN_POINT ( 'NONE',  ( 119.4624673109119755, -0.4425889791249831839, -15.72798183378646186 ) ) ;
#9649 = CARTESIAN_POINT ( 'NONE',  ( 125.5030348109119558, -6.222761293078241884, -8.102969835052219238 ) ) ;
#9650 = VECTOR ( 'NONE', #23284, 1000.000000000000227 ) ;
#9651 = CARTESIAN_POINT ( 'NONE',  ( 116.0864081442453113, -9.988377603198973276, -10.36322818467138163 ) ) ;
#9652 = CARTESIAN_POINT ( 'NONE',  ( 122.5910329359119970, -5.367793381288652910, -18.78638297431638904 ) ) ;
#9653 = ORIENTED_EDGE ( 'NONE', *, *, #14201, .F. ) ;
#9654 = CARTESIAN_POINT ( 'NONE',  ( -3.075987277002964593, -7.207016596002466358, -7.393215200338315363 ) ) ;
#9655 = CARTESIAN_POINT ( 'NONE',  ( 135.3184548109119874, -4.863998795839242995, -13.39321520033831447 ) ) ;
#9656 = CIRCLE ( 'NONE', #169, 2.445500000000005336 ) ;
#9657 = CARTESIAN_POINT ( 'NONE',  ( 124.5954081442453116, -6.222761293078241884, -8.102969835052219238 ) ) ;
#9658 = CARTESIAN_POINT ( 'NONE',  ( 109.0935046295247872, -4.863998795839590272, -18.39754474579285315 ) ) ;
#9659 = CARTESIAN_POINT ( 'NONE',  ( 112.3578015045248861, -6.936859964151250502, -18.39754474579286025 ) ) ;
#9660 = CARTESIAN_POINT ( 'NONE',  ( 118.8660148109119774, 0.1319031606808879209, -14.10382304977623669 ) ) ;
#9661 = CARTESIAN_POINT ( 'NONE',  ( 68.68839935636917460, -25.95913848132418522, -5.893215200338315363 ) ) ;
#9662 = CARTESIAN_POINT ( 'NONE',  ( 117.6180281442453150, -8.899110576539710493, -16.42337572283490132 ) ) ;
#9663 = CARTESIAN_POINT ( 'NONE',  ( 122.4397948109119767, -9.988377603198976828, -10.36322818467138340 ) ) ;
#9664 = ORIENTED_EDGE ( 'NONE', *, *, #36685, .T. ) ;
#9665 = CARTESIAN_POINT ( 'NONE',  ( 122.8368814775786291, -7.894159318335828068, -9.358103419637847864 ) ) ;
#9666 = AXIS2_PLACEMENT_3D ( 'NONE', #34604, #3389, #44905 ) ;
#9667 = CARTESIAN_POINT ( 'NONE',  ( 117.2209414775786485, -7.893985811506177619, -18.51759400769804742 ) ) ;
#9668 = CARTESIAN_POINT ( 'NONE',  ( 125.0492214775786266, -6.344957434206665248, -7.627207830600338134 ) ) ;
#9669 = CARTESIAN_POINT ( 'NONE',  ( 124.7088614775786226, -9.565557343593413364, -10.61323700422348004 ) ) ;
#9670 = ORIENTED_EDGE ( 'NONE', *, *, #7465, .F. ) ;
#9671 = CARTESIAN_POINT ( 'NONE',  ( 121.1325173109119788, -9.289237151508432433, -11.05642687123711276 ) ) ;
#9672 = EDGE_CURVE ( 'NONE', #31689, #3470, #8665, .T. ) ;
#9673 = CARTESIAN_POINT ( 'NONE',  ( 125.7299414775786346, 0.9020085738987339008, -11.91225656197089222 ) ) ;
#9674 = CARTESIAN_POINT ( 'NONE',  ( 114.0442481442453300, -7.643976991954077427, -18.09477374809248928 ) ) ;
#9675 = CARTESIAN_POINT ( 'NONE',  ( 125.2194014775786286, -10.30919188438810075, -12.61870101168855918 ) ) ;
#9676 = CARTESIAN_POINT ( 'NONE',  ( 114.6874464091100947, -0.9924539043446216624, -17.29976612834909133 ) ) ;
#9677 = CARTESIAN_POINT ( 'NONE',  ( 121.6881423109119709, -0.4387604401700512802, -15.73000352943951619 ) ) ;
#9678 = ORIENTED_EDGE ( 'NONE', *, *, #41297, .T. ) ;
#9679 = CONICAL_SURFACE ( 'NONE', #22746, 2.999999999999999556, 0.9599310885968830309 ) ;
#9680 = CARTESIAN_POINT ( 'NONE',  ( -7.923679509334008664, -5.078949698970065540, -17.89321520033831447 ) ) ;
#9681 = CARTESIAN_POINT ( 'NONE',  ( 110.7603796295247918, -4.863998795839590272, -8.388885654883775800 ) ) ;
#9682 = CIRCLE ( 'NONE', #26408, 2.999999999999999556 ) ;
#9683 = CARTESIAN_POINT ( 'NONE',  ( 70.19189222814998175, -56.69156685714467159, -35.87943827948784303 ) ) ;
#9684 = CARTESIAN_POINT ( 'NONE',  ( 120.0005481442453146, -4.153390946401325223, -8.397313243818185668 ) ) ;
#9685 = CARTESIAN_POINT ( 'NONE',  ( 115.8595014775786609, -7.643976991954077427, -18.09477374809248928 ) ) ;
#9686 = CARTESIAN_POINT ( 'NONE',  ( 125.1743048082055481, -0.1020945015695004648, -15.74893487844865980 ) ) ;
#9687 = VERTEX_POINT ( 'NONE', #28001 ) ;
#9688 = DIRECTION ( 'NONE',  ( -0.7071067811865480168, -0.5654279342906962658, -0.4246071727182139655 ) ) ;
#9689 = CARTESIAN_POINT ( 'NONE',  ( 121.3619881442452879, -5.574606645277164318, -18.38911715685844683 ) ) ;
#9690 = CARTESIAN_POINT ( 'NONE',  ( 113.8173414775786512, -9.565557343593413364, -10.61323700422348004 ) ) ;
#9691 = EDGE_CURVE ( 'NONE', #28792, #36696, #3800, .T. ) ;
#9692 = CONICAL_SURFACE ( 'NONE', #39539, 5.999999999999997335, 0.4636476090008060935 ) ;
#9693 = CARTESIAN_POINT ( 'NONE',  ( 84.49707967414211396, -25.99489077589524300, -13.39321520033831625 ) ) ;
#9694 = CARTESIAN_POINT ( 'NONE',  ( -2.989246886974374462, -7.181049323750285929, -19.39371206063207254 ) ) ;
#9696 = CARTESIAN_POINT ( 'NONE',  ( 125.8433948109119456, -1.834011780172310813, -8.268836392978581529 ) ) ;
#9695 = FACE_OUTER_BOUND ( 'NONE', #4977, .T. ) ;
#9697 = B_SPLINE_CURVE_WITH_KNOTS ( 'NONE', 3,
 ( #18004, #1342, #4762, #38740, #4310, #894, #14813, #42408, #11172, #35769, #15256, #35308, #28726, #4080, #43076, #18463, #11845, #3861, #28276, #7509, #42632, #17783, #18231, #24848, #11396, #32353, #42184, #11615, #39198, #4539 ),
 .UNSPECIFIED., .F., .F.,
 ( 4, 2, 2, 1, 2, 2, 2, 1, 1, 2, 2, 2, 1, 1, 1, 2, 2, 4 ),
 ( 0.000000000000000000, 0.03125000000000712624, 0.06250000000001425249, 0.09375000000002137179, 0.1093750000000202061, 0.1250000000000190403, 0.1875000000000160982, 0.2187500000000227318, 0.2343750000000259792, 0.2421875000000274780, 0.2500000000000289768, 0.3750000000000738853, 0.4375000000000856537, 0.4687500000000914269, 0.4843750000000939804, 0.4921875000000951461, 0.5000000000000962563, 1.000000000000000000 ),
 .UNSPECIFIED. ) ;
#9698 = CARTESIAN_POINT ( 'NONE',  ( 112.2857214775786474, -4.089484607189486809, -7.948022111789456723 ) ) ;
#9699 = VERTEX_POINT ( 'NONE', #14306 ) ;
#9700 = CARTESIAN_POINT ( 'NONE',  ( 114.9518748109119883, -1.834011780172310813, -8.268836392978581529 ) ) ;
#9701 = CARTESIAN_POINT ( 'NONE',  ( 126.3999550322272540, 0.07939618298893640069, -14.60940398381636562 ) ) ;
#9702 = CARTESIAN_POINT ( 'NONE',  ( 107.0793640045248196, 0.1403307496149616695, -15.46607636864997204 ) ) ;
#9703 = EDGE_CURVE ( 'NONE', #24392, #40611, #28455, .T. ) ;
#9704 = CARTESIAN_POINT ( 'NONE',  ( 112.0588148109119828, 0.5811942927096154232, -14.16772938898807155 ) ) ;
#9705 = CARTESIAN_POINT ( 'NONE',  ( 121.4754414775786131, -1.833838273342659697, -17.42832698103878286 ) ) ;
#9706 = ADVANCED_FACE ( 'NONE', ( #38684 ), #26897, .T. ) ;
#9707 = CARTESIAN_POINT ( 'NONE',  ( 105.6208483795248299, -0.7896495226426338832, -9.318865927141430916 ) ) ;
#9708 = DIRECTION ( 'NONE',  ( 0.000000000000000000, 0.000000000000000000, 1.000000000000000000 ) ) ;
#9709 = CARTESIAN_POINT ( 'NONE',  ( 109.2296347500660829, -1.724019187123235541, -17.33431401656127235 ) ) ;
#9710 = CARTESIAN_POINT ( 'NONE',  ( 113.3635281442453504, -0.1624402480850797581, -16.17319339645315424 ) ) ;
#9711 = CARTESIAN_POINT ( 'NONE',  ( 108.8851452545248151, 0.8980012041604421569, -11.00651665394454071 ) ) ;
#9712 = DIRECTION ( 'NONE',  ( -1.000000000000000000, 0.000000000000000000, -0.000000000000000000 ) ) ;
#9713 = CARTESIAN_POINT ( 'NONE',  ( 114.7886608795247696, -8.938348069036489818, -9.318865927141430916 ) ) ;
#9714 = CARTESIAN_POINT ( 'NONE',  ( 124.3685014775786328, -10.63000616557722466, -14.87417383870573495 ) ) ;
#9715 = CARTESIAN_POINT ( 'NONE',  ( 122.2696148109119889, -4.089484607189486809, -7.948022111789456723 ) ) ;
#9716 = DIRECTION ( 'NONE',  ( 0.000000000000000000, 0.6004852223388323917, -0.7996358532186279566 ) ) ;
#9717 = CARTESIAN_POINT ( 'NONE',  ( 121.3619881442452879, -4.089484607189486809, -7.948022111789456723 ) ) ;
#9718 = CARTESIAN_POINT ( 'NONE',  ( 114.1009748109119784, -4.089484607189486809, -7.948022111789456723 ) ) ;
#9719 = ORIENTED_EDGE ( 'NONE', *, *, #2425, .T. ) ;
#9720 = CARTESIAN_POINT ( 'NONE',  ( 112.6828081442453282, -2.084020599724406786, -8.691656652584148546 ) ) ;
#9721 = CIRCLE ( 'NONE', #230, 1.610000000000000986 ) ;
#9722 = CARTESIAN_POINT ( 'NONE',  ( 126.1270281442452870, -10.30919188438810075, -12.61870101168855918 ) ) ;
#9723 = VECTOR ( 'NONE', #37794, 1000.000000000000000 ) ;
#9724 = CARTESIAN_POINT ( 'NONE',  ( 125.5030348109119558, -3.383040157471821630, -19.15922257007629170 ) ) ;
#9725 = CARTESIAN_POINT ( 'NONE',  ( 113.5337081442453240, -9.261995988541697145, -16.69588392320189030 ) ) ;
#9726 = CARTESIAN_POINT ( 'NONE',  ( 113.5904348109119866, -2.084020599724406786, -8.691656652584148546 ) ) ;
#9727 = ORIENTED_EDGE ( 'NONE', *, *, #11666, .T. ) ;
#9728 = EDGE_CURVE ( 'NONE', #15657, #35973, #27629, .T. ) ;
#9729 = CARTESIAN_POINT ( 'NONE',  ( 118.4689281442453250, -10.15424416112533912, -14.75197769757731336 ) ) ;
#9730 = EDGE_CURVE ( 'NONE', #40512, #30086, #26271, .T. ) ;
#9731 = EDGE_CURVE ( 'NONE', #36064, #37401, #18138, .T. ) ;
#9732 = AXIS2_PLACEMENT_3D ( 'NONE', #10237, #6813, #17304 ) ;
#9733 = CARTESIAN_POINT ( 'NONE',  ( 109.0240515045248202, -6.936859964151250502, -18.39754474579286025 ) ) ;
#9734 = CARTESIAN_POINT ( 'NONE',  ( 122.2128881442453263, -7.643976991954077427, -18.09477374809248928 ) ) ;
#9735 = CARTESIAN_POINT ( 'NONE',  ( 123.9138173109119663, -0.4425889791248522331, -15.72798183378621140 ) ) ;
#9736 = CARTESIAN_POINT ( 'NONE',  ( 111.9410827545248708, -2.477300249445798297, -19.15521520033831138 ) ) ;
#9737 = ORIENTED_EDGE ( 'NONE', *, *, #10396, .F. ) ;
#9738 = CARTESIAN_POINT ( 'NONE',  ( 90.67797751089673852, -17.83979763915464289, -21.89321520033831447 ) ) ;
#9739 = CARTESIAN_POINT ( 'NONE',  ( 126.1837548109119211, -10.63000616557722466, -14.87417383870573495 ) ) ;
#9740 = CARTESIAN_POINT ( 'NONE',  ( 113.1912390045248031, -9.868328341294150263, -11.32035403202671020 ) ) ;
#9741 = CARTESIAN_POINT ( 'NONE',  ( 91.77400275106518279, -25.99489077589524300, -13.39321520033831625 ) ) ;
#9742 = CARTESIAN_POINT ( 'NONE',  ( 112.3424481442453384, -6.344957434206662583, -7.627207830600333693 ) ) ;
#9743 = CARTESIAN_POINT ( 'NONE',  ( 114.2372320646196897, 0.6269505268395592079, -14.64321520033831447 ) ) ;
#9744 = CARTESIAN_POINT ( 'NONE',  ( 108.8156921295247912, -9.868328341294093420, -13.39321520033831447 ) ) ;
#9745 = CARTESIAN_POINT ( 'NONE',  ( 111.5497331777918788, -0.01829820670803256055, -14.64321520033831447 ) ) ;
#9746 = CARTESIAN_POINT ( 'NONE',  ( 117.7314814775786260, -4.089484607189486809, -7.948022111789456723 ) ) ;
#9747 = VECTOR ( 'NONE', #26656, 1000.000000000000000 ) ;
#9748 = DIRECTION ( 'NONE',  ( 0.9999995469159186356, 0.0009519285464175526951, 0.000000000000000000 ) ) ;
#9749 = AXIS2_PLACEMENT_3D ( 'NONE', #22591, #2913, #41243 ) ;
#9750 = DIRECTION ( 'NONE',  ( 1.000000000000000000, 0.000000000000000000, 0.000000000000000000 ) ) ;
#9751 = CARTESIAN_POINT ( 'NONE',  ( 126.0703014775786102, -9.988377603198980381, -10.36322818467138518 ) ) ;
#9752 = CARTESIAN_POINT ( 'NONE',  ( 122.3830681442452857, -1.833838273342659697, -17.42832698103878286 ) ) ;
#9753 = CARTESIAN_POINT ( 'NONE',  ( 125.5597614775786326, -7.894159318335828068, -9.358103419637847864 ) ) ;
#9754 = ORIENTED_EDGE ( 'NONE', *, *, #10899, .T. ) ;
#9755 = CARTESIAN_POINT ( 'NONE',  ( 121.9859814775786333, 0.2603800115204892296, -16.42320221600525088 ) ) ;
#9756 = CARTESIAN_POINT ( 'NONE',  ( 119.5467348109119712, -4.089484607189486809, -7.948022111789456723 ) ) ;
#9757 = LINE ( 'NONE', #2900, #42308 ) ;
#9758 = CARTESIAN_POINT ( 'NONE',  ( 113.7414098793805408, -2.191907684172563986, -18.20049396185734025 ) ) ;
#9759 = CARTESIAN_POINT ( 'NONE',  ( 122.4965214775786251, -10.30919188438810075, -12.61870101168855918 ) ) ;
#9760 = CARTESIAN_POINT ( 'NONE',  ( 111.1076452545248259, 0.8980012041604421569, -11.00651665394454071 ) ) ;
#9761 = EDGE_CURVE ( 'NONE', #21643, #9382, #22047, .T. ) ;
#9762 = CARTESIAN_POINT ( 'NONE',  ( 106.9404577545248145, -2.791137627527939813, -18.39754474579286025 ) ) ;
#9763 = CARTESIAN_POINT ( 'NONE',  ( 83.21177402427441905, -31.92419490535376170, -23.43773257735213988 ) ) ;
#9764 = AXIS2_PLACEMENT_3D ( 'NONE', #9503, #40290, #33196 ) ;
#9765 = CARTESIAN_POINT ( 'NONE',  ( 117.4478481442453131, -9.565557343593413364, -10.61323700422348004 ) ) ;
#9766 = CARTESIAN_POINT ( 'NONE',  ( 116.2565881442453133, -0.8288870151387760510, -10.36305467784173118 ) ) ;
#9767 = CARTESIAN_POINT ( 'NONE',  ( 113.1221837908068011, 0.5115630086001619059, -12.14321520033829493 ) ) ;
#9768 = CARTESIAN_POINT ( 'NONE',  ( 115.5526452545247622, -9.868328341294098749, -15.46607636864997204 ) ) ;
#9769 = ORIENTED_EDGE ( 'NONE', *, *, #28510, .T. ) ;
#9770 = DIRECTION ( 'NONE',  ( 1.000000000000000000, 0.000000000000000000, 0.000000000000000000 ) ) ;
#9771 = CARTESIAN_POINT ( 'NONE',  ( 112.5126281442453120, -10.30919188438810075, -12.61870101168855918 ) ) ;
#9772 = CARTESIAN_POINT ( 'NONE',  ( 79.39048153618716697, 5.042594898335129194, -6.287573381101518422 ) ) ;
#9773 = CARTESIAN_POINT ( 'NONE',  ( 123.1466579359119891, -4.360204210389833968, -8.000047426360245240 ) ) ;
#9774 = CARTESIAN_POINT ( 'NONE',  ( 124.1190016859119680, -9.665098340737509730, -17.37397104707595474 ) ) ;
#9775 = ORIENTED_EDGE ( 'NONE', *, *, #28955, .F. ) ;
#9776 = CARTESIAN_POINT ( 'NONE',  ( 113.9552233795247815, -8.938348069036441856, -17.46756447353520514 ) ) ;
#9777 = CARTESIAN_POINT ( 'NONE',  ( 111.5125327111057345, -1.267766418764825875, -16.93314635290698789 ) ) ;
#9778 = VERTEX_POINT ( 'NONE', #36164 ) ;
#9779 = CARTESIAN_POINT ( 'NONE',  ( 118.0151148109119816, -10.63000616557722466, -14.87417383870573495 ) ) ;
#9780 = CARTESIAN_POINT ( 'NONE',  ( 113.8740681442453138, 0.5811942927096154232, -14.16772938898807155 ) ) ;
#9781 = CARTESIAN_POINT ( 'NONE',  ( 117.9016614775786280, -0.1624402480850797581, -16.17319339645315424 ) ) ;
#9782 =( NAMED_UNIT ( * ) PLANE_ANGLE_UNIT ( ) SI_UNIT ( $, .RADIAN. ) );
#9783 = CARTESIAN_POINT ( 'NONE',  ( 116.0506660444391969, -1.267766418764730840, -16.93314635290706605 ) ) ;
#9784 = CARTESIAN_POINT ( 'NONE',  ( 122.6667014775786413, -7.893985811506177619, -18.51759400769804742 ) ) ;
#9785 = CARTESIAN_POINT ( 'NONE',  ( 120.0005481442453146, -5.638512984488999180, -18.83840828888717311 ) ) ;
#9786 = EDGE_CURVE ( 'NONE', #21756, #36673, #3330, .T. ) ;
#9787 = CIRCLE ( 'NONE', #10496, 2.000000000000000444 ) ;
#9788 = CARTESIAN_POINT ( 'NONE',  ( 106.5931921295248372, -9.868328341294093420, -13.39321520033831447 ) ) ;
#9789 = EDGE_CURVE ( 'NONE', #16272, #27457, #4931, .T. ) ;
#9790 = CARTESIAN_POINT ( 'NONE',  ( 114.3846081442453197, 0.4262465694468514643, -12.03445270309931736 ) ) ;
#9791 = CARTESIAN_POINT ( 'NONE',  ( 124.8790414775786246, -8.899110576539426276, -16.42337572283528146 ) ) ;
#9792 = ORIENTED_EDGE ( 'NONE', *, *, #28832, .T. ) ;
#9793 = EDGE_CURVE ( 'NONE', #16955, #27202, #18885, .T. ) ;
#9794 = CARTESIAN_POINT ( 'NONE',  ( 118.3554748109119998, 0.2603800115204892296, -16.42320221600525088 ) ) ;
#9795 = CARTESIAN_POINT ( 'NONE',  ( 126.3063647503470719, -5.222031867898532909, -18.42446631453262285 ) ) ;
#9796 = CARTESIAN_POINT ( 'NONE',  ( 113.9307948109119906, 0.9020085738987339008, -11.91225656197089222 ) ) ;
#9797 = ORIENTED_EDGE ( 'NONE', *, *, #20886, .F. ) ;
#9798 = CARTESIAN_POINT ( 'NONE',  ( 121.4754414775786131, -8.166667518702819706, -8.995218007635861213 ) ) ;
#9800 = CARTESIAN_POINT ( 'NONE',  ( 71.02242295334774269, -99.02728775972636299, -55.91838671430374319 ) ) ;
#9799 = B_SPLINE_CURVE_WITH_KNOTS ( 'NONE', 3,
 ( #41237, #20025, #33907, #44423, #2677, #12965, #16838, #9767, #13190, #23219 ),
 .UNSPECIFIED., .F., .F.,
 ( 4, 3, 3, 4 ),
 ( 0.000000000000000000, 0.0002476487219222810133, 0.0004952974148303629972, 0.0009534114850261790879 ),
 .UNSPECIFIED. ) ;
#9801 = CARTESIAN_POINT ( 'NONE',  ( 112.3991748109119868, -1.833838273342658809, -17.42832698103878286 ) ) ;
#9802 = CARTESIAN_POINT ( 'NONE',  ( 125.1269327111056953, -1.267766418764818770, -16.93314635290698078 ) ) ;
#9803 =( BOUNDED_CURVE ( )  B_SPLINE_CURVE ( 2, ( #20974, #7277, #28939, #35070, #14352 ),
 .UNSPECIFIED., .F., .F. ) 
 B_SPLINE_CURVE_WITH_KNOTS ( ( 3, 2, 3 ),
 ( 0.6040431156034949955, 0.6125000000000000444, 0.6127876305315190786 ),
 .UNSPECIFIED. ) 
 CURVE ( )  GEOMETRIC_REPRESENTATION_ITEM ( )  RATIONAL_B_SPLINE_CURVE ( ( 0.9666851417651740608, 0.9485006404992010198, 1.000000000000000000, 0.9982484343581399244, 0.9965774773173300405 ) ) 
 REPRESENTATION_ITEM ( '' )  );
#9804 = CARTESIAN_POINT ( 'NONE',  ( 116.0296814775786345, -1.833838273342658809, -17.42832698103878286 ) ) ;
#9805 = DIRECTION ( 'NONE',  ( 0.000000000000000000, 1.000000000000000000, 0.000000000000000000 ) ) ;
#9806 = CARTESIAN_POINT ( 'NONE',  ( 118.9227414775786542, 0.4262465694468514643, -12.03445270309931736 ) ) ;
#9807 = VECTOR ( 'NONE', #1415, 1000.000000000000000 ) ;
#9808 = LINE ( 'NONE', #23717, #36850 ) ;
#9809 = CARTESIAN_POINT ( 'NONE',  ( 114.4413348109119823, -0.8288870151387760510, -10.36305467784173118 ) ) ;
#9810 = CARTESIAN_POINT ( 'NONE',  ( 115.2355081442453155, -10.30919188438810075, -12.61870101168855918 ) ) ;
#9811 = CARTESIAN_POINT ( 'NONE',  ( 122.9382985609119743, -0.08252387247370887580, -11.91645802438286417 ) ) ;
#9812 = CARTESIAN_POINT ( 'NONE',  ( 111.9453614775786434, -1.561330072975668060, -17.79121239304076596 ) ) ;
#9813 = CARTESIAN_POINT ( 'NONE',  ( 116.4834948109119779, -7.894159318335828068, -9.358103419637847864 ) ) ;
#9814 = CARTESIAN_POINT ( 'NONE',  ( 112.6260814775786514, -0.8288870151387760510, -10.36305467784173118 ) ) ;
#9815 = CARTESIAN_POINT ( 'NONE',  ( 118.3554748109119998, -9.565557343593413364, -10.61323700422348004 ) ) ;
#9816 = ORIENTED_EDGE ( 'NONE', *, *, #3869, .F. ) ;
#9817 = CARTESIAN_POINT ( 'NONE',  ( 113.7038881442453402, -3.383040157471821630, -19.15922257007629170 ) ) ;
#9818 = CARTESIAN_POINT ( 'NONE',  ( 107.8433483795247838, -0.7896495226426338832, -9.318865927141430916 ) ) ;
#9819 = CARTESIAN_POINT ( 'NONE',  ( 107.4960827545248350, -6.936859964151250502, -8.388885654883777576 ) ) ;
#9820 = CARTESIAN_POINT ( 'NONE',  ( 106.5237390045248418, -9.868328341294098749, -11.32035403202665869 ) ) ;
#9821 = CARTESIAN_POINT ( 'NONE',  ( 64.35706024680830240, -36.56378831979270672, -5.594626812820024497 ) ) ;
#9822 = CARTESIAN_POINT ( 'NONE',  ( 118.4122014775786340, 0.5811942927096110934, -14.16772938898807510 ) ) ;
#9823 = ORIENTED_EDGE ( 'NONE', *, *, #98, .F. ) ;
#9824 = CARTESIAN_POINT ( 'NONE',  ( 124.8223148109119762, 0.9020085738987339008, -11.91225656197089222 ) ) ;
#9825 = DIRECTION ( 'NONE',  ( 0.000000000000000000, 0.000000000000000000, 1.000000000000000000 ) ) ;
#9826 = CARTESIAN_POINT ( 'NONE',  ( 118.7525614775786380, -1.833838273342659253, -17.42832698103878286 ) ) ;
#9827 = CARTESIAN_POINT ( 'NONE',  ( 95.28169473643895060, -25.99489077589524300, -13.39321520033831447 ) ) ;
#9828 = ADVANCED_FACE ( 'NONE', ( #39823 ), #16696, .T. ) ;
#9829 = CARTESIAN_POINT ( 'NONE',  ( 124.5954081442453116, -3.383040157471821630, -19.15922257007629170 ) ) ;
#9830 = CARTESIAN_POINT ( 'NONE',  ( 115.7610046295247912, -4.863998795839590272, -18.39754474579285315 ) ) ;
#9831 = CARTESIAN_POINT ( 'NONE',  ( 124.3404700565388907, -8.485573535863879968, -17.53172993199661889 ) ) ;
#9832 = ORIENTED_EDGE ( 'NONE', *, *, #24371, .F. ) ;
#9833 = CARTESIAN_POINT ( 'NONE',  ( 96.54708369096698561, -24.20446030063578391, -12.09626349990295147 ) ) ;
#9834 = CARTESIAN_POINT ( 'NONE',  ( 124.3117748109119844, 0.1319031606808879209, -14.10382304977623669 ) ) ;
#9835 = CARTESIAN_POINT ( 'NONE',  ( 118.5823814775786360, -1.834011780172310813, -8.268836392978581529 ) ) ;
#9836 = CARTESIAN_POINT ( 'NONE',  ( 113.8173414775786512, -9.565557343593413364, -10.61323700422348004 ) ) ;
#9837 = CARTESIAN_POINT ( 'NONE',  ( 119.2631014775786298, 0.2603800115204892296, -16.42320221600525088 ) ) ;
#9838 = DIRECTION ( 'NONE',  ( 0.000000000000000000, 0.000000000000000000, -1.000000000000000000 ) ) ;
#9839 = CARTESIAN_POINT ( 'NONE',  ( 126.5254139958947519, -1.171961747752007899, -9.797753127676378071 ) ) ;
#9840 = CARTESIAN_POINT ( 'NONE',  ( 124.7088614775786226, -9.565557343593413364, -10.61323700422348004 ) ) ;
#9841 = EDGE_LOOP ( 'NONE', ( #10360, #6865 ) ) ;
#9842 = B_SPLINE_CURVE_WITH_KNOTS ( 'NONE', 3,
 ( #39852, #1536, #15228, #40303, #43275, #25946, #8837, #40073, #9293, #15913, #43953, #12271, #29136, #9066, #43048, #1986, #5628, #8618, #12495, #22968, #18657, #5180, #22736, #22515, #11815, #12716, #36859, #15457, #25723, #19549, #29811, #32763, #36638, #2206, #18872, #16135, #30036, #39629, #19097, #1758, #15684, #29586, #26619, #22297, #40532, #43727, #32546, #36193, #4958 ),
 .UNSPECIFIED., .F., .F.,
 ( 4, 2, 2, 2, 2, 2, 2, 2, 2, 1, 2, 2, 2, 2, 2, 2, 2, 1, 2, 2, 2, 2, 1, 2, 2, 4 ),
 ( 0.000000000000000000, 0.06250000000002639555, 0.1250000000000527911, 0.1875000000000791867, 0.2187500000000920375, 0.2500000000001049161, 0.3750000000001461609, 0.4375000000001676992, 0.4687500000001784684, 0.4843750000001839640, 0.4921875000001855738, 0.5000000000001870726, 0.5625000000001556533, 0.5937500000001373346, 0.6250000000001189049, 0.6875000000000800471, 0.7187500000000606182, 0.7343750000000504041, 0.7421875000000455191, 0.7500000000000407452, 0.8125000000000127676, 0.8437499999999957812, 0.8593749999999867883, 0.8671874999999870104, 0.8749999999999871214, 1.000000000000000000 ),
 .UNSPECIFIED. ) ;
#9843 = CIRCLE ( 'NONE', #37483, 5.000000000000000000 ) ;
#9844 = CARTESIAN_POINT ( 'NONE',  ( 124.0495485609119584, -10.36940331770106916, -15.09355782777062061 ) ) ;
#9845 = EDGE_CURVE ( 'NONE', #18037, #5517, #9042, .T. ) ;
#9846 = CARTESIAN_POINT ( 'NONE',  ( 117.2209414775786485, -7.893985811506177619, -18.51759400769804742 ) ) ;
#9847 = CARTESIAN_POINT ( 'NONE',  ( 120.4543614775786295, -5.574606645277164318, -18.38911715685844683 ) ) ;
#9848 = ORIENTED_EDGE ( 'NONE', *, *, #9032, .T. ) ;
#9849 = CARTESIAN_POINT ( 'NONE',  ( 122.6604860609119640, -3.387241619883791355, -18.17469012370385073 ) ) ;
#9850 = CARTESIAN_POINT ( 'NONE',  ( 135.3184548109119874, -1.191816558809784876, -8.648209655763537285 ) ) ;
#9851 = CARTESIAN_POINT ( 'NONE',  ( 117.6747548109119919, -1.834011780172310813, -8.268836392978581529 ) ) ;
#9852 = AXIS2_PLACEMENT_3D ( 'NONE', #27473, #27697, #44804 ) ;
#9853 = CARTESIAN_POINT ( 'NONE',  ( 111.7327233795247849, -8.938348069036489818, -17.46756447353520159 ) ) ;
#9854 = CARTESIAN_POINT ( 'NONE',  ( 117.9016614775786280, -0.1624402480850797581, -16.17319339645315424 ) ) ;
#9855 = ORIENTED_EDGE ( 'NONE', *, *, #35878, .F. ) ;
#9856 = VERTEX_POINT ( 'NONE', #39603 ) ;
#9857 = CARTESIAN_POINT ( 'NONE',  ( 126.3539348109119800, -4.153390946401325223, -8.397313243818185668 ) ) ;
#9858 = CARTESIAN_POINT ( 'NONE',  ( 122.9503348109119827, -9.859900752359378018, -12.68260735090039759 ) ) ;
#9859 = PLANE ( 'NONE',  #349 ) ;
#9860 = CARTESIAN_POINT ( 'NONE',  ( 78.69189222814998175, -68.13214146720427777, -20.74076566292613677 ) ) ;
#9861 = CARTESIAN_POINT ( 'NONE',  ( 123.5176014775786228, -9.261995988541697145, -16.69588392320189030 ) ) ;
#9862 = CARTESIAN_POINT ( 'NONE',  ( 64.69189222814998175, -41.76310523276723785, -47.71602681600972318 ) ) ;
#9863 = CARTESIAN_POINT ( 'NONE',  ( 71.09163384711422395, -63.65591304925720095, -42.02869409913880361 ) ) ;
#9864 = CARTESIAN_POINT ( 'NONE',  ( 121.7023481442452777, -9.261995988541697145, -16.69588392320189030 ) ) ;
#9866 = CARTESIAN_POINT ( 'NONE',  ( 118.2987481442453088, -7.894159318335828068, -9.358103419637847864 ) ) ;
#9865 = CARTESIAN_POINT ( 'NONE',  ( 119.7169148109119874, -9.988377603198976828, -10.36322818467138340 ) ) ;
#9867 = CARTESIAN_POINT ( 'NONE',  ( 123.9146881442452894, -10.15424416112533912, -14.75197769757731336 ) ) ;
#9868 = CARTESIAN_POINT ( 'NONE',  ( 112.6260814775786514, -9.261995988541697145, -16.69588392320189030 ) ) ;
#9869 = ORIENTED_EDGE ( 'NONE', *, *, #19486, .F. ) ;
#9870 = CARTESIAN_POINT ( 'NONE',  ( 122.6667014775786413, -2.084020599724406786, -8.691656652584148546 ) ) ;
#9871 = CARTESIAN_POINT ( 'NONE',  ( 123.1205148109119563, -1.834011780172307704, -8.268836392978586858 ) ) ;
#9872 = FACE_OUTER_BOUND ( 'NONE', #10047, .T. ) ;
#9873 = AXIS2_PLACEMENT_3D ( 'NONE', #3769, #3994, #17469 ) ;
#9874 = CARTESIAN_POINT ( 'NONE',  ( 107.7738952545248310, 0.8980012041604421569, -11.00651665394454071 ) ) ;
#9875 = CARTESIAN_POINT ( 'NONE',  ( 115.2053796295247849, -4.863998795839590272, -8.388885654883775800 ) ) ;
#9876 = CARTESIAN_POINT ( 'NONE',  ( 108.8156921295247912, 0.8980012041604618078, -13.39321520033831447 ) ) ;
#9877 = CARTESIAN_POINT ( 'NONE',  ( 123.7445081442452874, -1.561330072975668948, -17.79121239304076951 ) ) ;
#9878 = CARTESIAN_POINT ( 'NONE',  ( 123.2339681442453241, -3.505236298600246325, -18.68346056562440793 ) ) ;
#9879 = ORIENTED_EDGE ( 'NONE', *, *, #22523, .F. ) ;
#9880 = CARTESIAN_POINT ( 'NONE',  ( 125.7299414775786346, 0.9020085738987339008, -11.91225656197089222 ) ) ;
#9881 = CARTESIAN_POINT ( 'NONE',  ( 113.5904348109119866, -2.084020599724406786, -8.691656652584148546 ) ) ;
#9882 = CARTESIAN_POINT ( 'NONE',  ( 121.9292548109119849, -7.894159318335831621, -9.358103419637851417 ) ) ;
#9883 = CARTESIAN_POINT ( 'NONE',  ( 118.6958348109119754, -6.344957434206665248, -7.627207830600338134 ) ) ;
#9884 = CARTESIAN_POINT ( 'NONE',  ( 121.3052614775786111, -1.834011780172310813, -8.268836392978581529 ) ) ;
#9886 = VECTOR ( 'NONE', #42926, 1000.000000000000000 ) ;
#9885 = CARTESIAN_POINT ( 'NONE',  ( 119.6013735609119806, -0.08666061303654916392, -11.91773565553416425 ) ) ;
#9887 = CARTESIAN_POINT ( 'NONE',  ( 126.2404814775786264, -0.8288870151387760510, -10.36305467784173118 ) ) ;
#9888 = CARTESIAN_POINT ( 'NONE',  ( 122.9382985609119743, -0.08252387247370887580, -11.91645802438286417 ) ) ;
#9889 = CARTESIAN_POINT ( 'NONE',  ( 115.8999108795247821, -1.325403438956436419, -16.93181055722141792 ) ) ;
#9890 = ORIENTED_EDGE ( 'NONE', *, *, #1715, .T. ) ;
#9891 = DIRECTION ( 'NONE',  ( 0.000000000000000000, 0.000000000000000000, 1.000000000000000000 ) ) ;
#9892 = CARTESIAN_POINT ( 'NONE',  ( 112.5126281442453120, 0.1319031606808879209, -14.10382304977623669 ) ) ;
#9893 = CARTESIAN_POINT ( 'NONE',  ( 125.3895814775786448, -2.084020599724406786, -8.691656652584148546 ) ) ;
#9894 = CARTESIAN_POINT ( 'NONE',  ( 106.2459265045248173, -2.791137627527939813, -8.388885654883777576 ) ) ;
#9895 = CARTESIAN_POINT ( 'NONE',  ( 111.6632702545248605, 0.1403307496149616695, -11.32035403202665336 ) ) ;
#9896 = CARTESIAN_POINT ( 'NONE',  ( 122.5532481442453019, 0.4262465694468514643, -12.03445270309931736 ) ) ;
#9897 = CARTESIAN_POINT ( 'NONE',  ( 70.19189222814998175, -52.04917782255280656, -34.02249884819201498 ) ) ;
#9898 = CARTESIAN_POINT ( 'NONE',  ( 116.8805814775786445, -3.505236298600246325, -18.68346056562440793 ) ) ;
#9899 = CARTESIAN_POINT ( 'NONE',  ( 121.8725281442453223, -3.383040157471821630, -19.15922257007629170 ) ) ;
#9900 = ORIENTED_EDGE ( 'NONE', *, *, #37536, .T. ) ;
#9901 = CARTESIAN_POINT ( 'NONE',  ( 121.3052614775786111, -7.643976991954077427, -18.09477374809248928 ) ) ;
#9902 = CARTESIAN_POINT ( 'NONE',  ( 118.0151148109119816, -10.63000616557722466, -14.87417383870573495 ) ) ;
#9903 = CARTESIAN_POINT ( 'NONE',  ( 124.0848681442452772, -4.089484607189486809, -7.948022111789456723 ) ) ;
#9904 = EDGE_CURVE ( 'NONE', #40373, #12976, #5010, .T. ) ;
#9905 = CARTESIAN_POINT ( 'NONE',  ( 123.2906948109119867, -1.833838273342659697, -17.42832698103878286 ) ) ;
#9906 = VERTEX_POINT ( 'NONE', #32518 ) ;
#9907 = DIRECTION ( 'NONE',  ( 0.8636456077245080465, -0.5040994586965603652, 0.000000000000000000 ) ) ;
#9908 = AXIS2_PLACEMENT_3D ( 'NONE', #42434, #691, #32599 ) ;
#9909 = CARTESIAN_POINT ( 'NONE',  ( 122.2696148109119889, -4.089484607189486809, -7.948022111789456723 ) ) ;
#9910 = CARTESIAN_POINT ( 'NONE',  ( 115.5191414775786569, -6.222761293078241884, -8.102969835052219238 ) ) ;
#9911 = CARTESIAN_POINT ( 'NONE',  ( 112.9097148109120070, -9.565557343593413364, -10.61323700422348004 ) ) ;
#9912 = DIRECTION ( 'NONE',  ( 2.478482478837576011E-29, 0.6004852223389939292, -0.7996358532185066093 ) ) ;
#9913 = CARTESIAN_POINT ( 'NONE',  ( 123.7022829359119811, -5.367793381288652910, -18.78638297431638904 ) ) ;
#9914 = EDGE_LOOP ( 'NONE', ( #30288, #15330, #1190, #2309, #30814 ) ) ;
#9915 = LINE ( 'NONE', #34060, #6253 ) ;
#9916 = DIRECTION ( 'NONE',  ( -1.000000000000000000, 0.000000000000000000, 0.000000000000000000 ) ) ;
#9917 = CARTESIAN_POINT ( 'NONE',  ( 115.6220983795247861, -0.7896495226426338832, -9.318865927141430916 ) ) ;
#9918 = DIRECTION ( 'NONE',  ( 0.9609149988134843001, -0.1028163501681632064, 0.2570431154366505933 ) ) ;
#9919 = CARTESIAN_POINT ( 'NONE',  ( 124.2550481442452792, -0.1624402480850797581, -16.17319339645315424 ) ) ;
#9920 = CARTESIAN_POINT ( 'NONE',  ( 114.0442481442453300, -7.643976991954077427, -18.09477374809248928 ) ) ;
#9921 = CARTESIAN_POINT ( 'NONE',  ( 127.3665996190938046, -6.875750515655262518, -18.59280027438719429 ) ) ;
#9922 = ORIENTED_EDGE ( 'NONE', *, *, #8010, .F. ) ;
#9923 = CARTESIAN_POINT ( 'NONE',  ( 123.6808719482204992, -5.999156839134923480, -18.26265215102791117 ) ) ;
#9924 = CARTESIAN_POINT ( 'NONE',  ( 114.3278814775786429, 0.1319031606808879209, -14.10382304977623669 ) ) ;
#9925 = CARTESIAN_POINT ( 'NONE',  ( 112.9134265045247787, -7.250697342233347165, -19.15521520033830427 ) ) ;
#9926 = CARTESIAN_POINT ( 'NONE',  ( 111.5588148109119828, 0.08617673920517221475, -14.09731900820172967 ) ) ;
#9928 = CARTESIAN_POINT ( 'NONE',  ( 125.3895814775786448, -7.893985811506177619, -18.51759400769804742 ) ) ;
#9927 = CARTESIAN_POINT ( 'NONE',  ( 64.61935771200890599, -37.86087448816891765, -4.893215200338314474 ) ) ;
#9929 = VECTOR ( 'NONE', #3966, 1000.000000000000114 ) ;
#9930 = CARTESIAN_POINT ( 'NONE',  ( 126.5241148109119393, -9.565557343593413364, -10.61323700422348004 ) ) ;
#9931 = VERTEX_POINT ( 'NONE', #43251 ) ;
#9932 = CARTESIAN_POINT ( 'NONE',  ( 112.2857214775786474, -4.089484607189486809, -7.948022111789456723 ) ) ;
#9933 = CARTESIAN_POINT ( 'NONE',  ( 113.7406697909088393, -1.016270020561755860, -17.26805140881366896 ) ) ;
#9934 = CARTESIAN_POINT ( 'NONE',  ( 114.1635827545248389, -2.477300249445798297, -19.15521520033831138 ) ) ;
#9935 = CARTESIAN_POINT ( 'NONE',  ( 124.4252281442452812, -0.8288870151387760510, -10.36305467784173118 ) ) ;
#9936 = CARTESIAN_POINT ( 'NONE',  ( 124.0281414775786146, -7.643976991954077427, -18.09477374809248928 ) ) ;
#9937 = CARTESIAN_POINT ( 'NONE',  ( 83.72016463086879412, -25.99489077589524300, -13.39321520033831447 ) ) ;
#9938 = CARTESIAN_POINT ( 'NONE',  ( 114.0941296295247867, -4.863998795839590272, -8.388885654883775800 ) ) ;
#9939 = AXIS2_PLACEMENT_3D ( 'NONE', #10201, #2893, #9750 ) ;
#9940 = CARTESIAN_POINT ( 'NONE',  ( 83.75466360696344736, -7.807702403958562520, -16.89321520033831447 ) ) ;
#9941 = LINE ( 'NONE', #30451, #14343 ) ;
#9942 = CARTESIAN_POINT ( 'NONE',  ( 113.9307948109119764, -10.15424416112533912, -14.75197769757731336 ) ) ;
#9943 = CARTESIAN_POINT ( 'NONE',  ( 108.2600671295247992, -10.62599879583958540, -13.39321520033831447 ) ) ;
#9944 = CARTESIAN_POINT ( 'NONE',  ( 111.7184544661070333, -9.250647026409817286, -16.71020059006274039 ) ) ;
#9945 = CARTESIAN_POINT ( 'NONE',  ( 113.3301452545248083, 0.8980012041604421569, -11.00651665394454071 ) ) ;
#9946 = CARTESIAN_POINT ( 'NONE',  ( 69.36136150295220659, -56.26572332408330368, -32.60429470211573033 ) ) ;
#9947 = CARTESIAN_POINT ( 'NONE',  ( 120.3409081442453044, -0.4660016031367893996, -10.09054647747474043 ) ) ;
#9948 = CARTESIAN_POINT ( 'NONE',  ( 127.7184548109119788, -4.863998795839242995, -13.39321520033831447 ) ) ;
#9949 = CARTESIAN_POINT ( 'NONE',  ( 120.0005481442453146, -5.638512984488999180, -18.83840828888717311 ) ) ;
#9950 = DIRECTION ( 'NONE',  ( 0.6049664196031386831, -0.7962509850245457210, 0.000000000000000000 ) ) ;
#9951 = VERTEX_POINT ( 'NONE', #2176 ) ;
#9952 = CARTESIAN_POINT ( 'NONE',  ( 112.5693548109119888, 0.4262465694468514643, -12.03445270309931736 ) ) ;
#9953 = AXIS2_PLACEMENT_3D ( 'NONE', #35771, #24851, #32356 ) ;
#9954 = CARTESIAN_POINT ( 'NONE',  ( 125.0492214775786266, -6.344957434206665248, -7.627207830600338134 ) ) ;
#9955 = CARTESIAN_POINT ( 'NONE',  ( 124.5386814775786206, -5.638512984488999180, -18.83840828888717311 ) ) ;
#9956 = CARTESIAN_POINT ( 'NONE',  ( 114.4980614775786592, -7.893985811506177619, -18.51759400769804742 ) ) ;
#9957 = CARTESIAN_POINT ( 'NONE',  ( 111.7751814775786556, -2.084020599724406786, -8.691656652584148546 ) ) ;
#9958 = ORIENTED_EDGE ( 'NONE', *, *, #17407, .F. ) ;
#9959 = CARTESIAN_POINT ( 'NONE',  ( 118.5823814775786360, -7.643976991954077427, -18.09477374809248928 ) ) ;
#9960 = B_SPLINE_CURVE_WITH_KNOTS ( 'NONE', 3,
 ( #41133, #26761, #34036, #6465, #12860, #13534, #44775, #30178, #13083, #40902 ),
 .UNSPECIFIED., .F., .F.,
 ( 4, 3, 3, 4 ),
 ( 0.000000000000000000, 0.0001671877548681284921, 0.0003343755096277660228, 0.0006463528481650619413 ),
 .UNSPECIFIED. ) ;
#9961 = CARTESIAN_POINT ( 'NONE',  ( 113.2500748109119968, -6.344957434206662583, -7.627207830600332805 ) ) ;
#9962 = CARTESIAN_POINT ( 'NONE',  ( 123.2906948109119867, -1.833838273342659697, -17.42832698103878286 ) ) ;
#9963 = DIRECTION ( 'NONE',  ( 0.2768435750659263284, 0.3568721902840676363, -0.8921882507333129819 ) ) ;
#9964 = AXIS2_PLACEMENT_3D ( 'NONE', #42029, #3494, #24688 ) ;
#9965 = B_SPLINE_CURVE_WITH_KNOTS ( 'NONE', 3,
 ( #45025, #13783, #37946, #10367, #38163, #6719, #27695, #24275, #34938, #34724 ),
 .UNSPECIFIED., .F., .F.,
 ( 4, 3, 3, 4 ),
 ( 0.000000000000000000, 0.0001671877560958085049, 0.0003343755126086545080, 0.0006438490228505469159 ),
 .UNSPECIFIED. ) ;
#9966 = CARTESIAN_POINT ( 'NONE',  ( 115.1359265045248605, -7.250697342233347165, -19.15521520033831138 ) ) ;
#9967 = EDGE_LOOP ( 'NONE', ( #39098, #40475, #39123, #40858 ) ) ;
#9968 = CARTESIAN_POINT ( 'NONE',  ( 89.70384154612264638, -12.43804770190545561, -8.143215200338314474 ) ) ;
#9969 = EDGE_CURVE ( 'NONE', #19203, #1246, #35603, .T. ) ;
#9970 = CARTESIAN_POINT ( 'NONE',  ( 124.9924948109119924, -4.089484607189486809, -7.948022111789456723 ) ) ;
#9971 = CIRCLE ( 'NONE', #35416, 2.000000000000000444 ) ;
#9972 = CARTESIAN_POINT ( 'NONE',  ( 113.7722331777918896, -0.01829820670813664396, -14.64321520033831447 ) ) ;
#9973 = CARTESIAN_POINT ( 'NONE',  ( 117.1003875888201406, 1.599829628806384463, -5.419835913930024063 ) ) ;
#9974 = CARTESIAN_POINT ( 'NONE',  ( 94.20708369096698220, -27.10035099198479358, -13.29271931396930739 ) ) ;
#9975 = CARTESIAN_POINT ( 'NONE',  ( 108.3989733795248753, -1.325403438956436419, -9.854619843455211026 ) ) ;
#9976 = CARTESIAN_POINT ( 'NONE',  ( 78.29371559379771384, 3.878430683262073408, -21.89321520033832513 ) ) ;
#9977 = CARTESIAN_POINT ( 'NONE',  ( 117.6747548109119919, -1.834011780172310813, -8.268836392978581529 ) ) ;
#9978 = DIRECTION ( 'NONE',  ( 0.6049664196031393493, -0.7962509850245451659, -0.000000000000000000 ) ) ;
#9979 = CARTESIAN_POINT ( 'NONE',  ( 125.1309504620138284, -2.495269033102075262, -17.79652296963211455 ) ) ;
#9980 = CARTESIAN_POINT ( 'NONE',  ( 124.1884548109119777, -2.527210466738289529, -8.967976844668992698 ) ) ;
#9981 = CARTESIAN_POINT ( 'NONE',  ( 120.5678148109119832, -1.833838273342659253, -17.42832698103878286 ) ) ;
#9982 = EDGE_CURVE ( 'NONE', #3603, #27652, #44167, .T. ) ;
#9983 = ORIENTED_EDGE ( 'NONE', *, *, #14309, .F. ) ;
#9984 = CARTESIAN_POINT ( 'NONE',  ( 121.9750102976252180, -8.580000213326620440, -17.71054824844518905 ) ) ;
#9985 = CARTESIAN_POINT ( 'NONE',  ( 119.3198281442452924, 0.5811942927096110934, -14.16772938898807510 ) ) ;
#9986 = DIRECTION ( 'NONE',  ( 0.000000000000000000, 0.000000000000000000, -1.000000000000000000 ) ) ;
#9987 = CARTESIAN_POINT ( 'NONE',  ( 115.2922348109119781, 0.4262465694468514643, -12.03445270309931736 ) ) ;
#9988 = EDGE_CURVE ( 'NONE', #43799, #23752, #10858, .T. ) ;
#9989 = EDGE_CURVE ( 'NONE', #21089, #24095, #28334, .T. ) ;
#9990 = CARTESIAN_POINT ( 'NONE',  ( 113.0231681442453180, -10.15424416112533912, -14.75197769757731336 ) ) ;
#9991 = CARTESIAN_POINT ( 'NONE',  ( 109.3018640045248304, -10.62599879583958717, -11.00651665394454604 ) ) ;
#9992 = CARTESIAN_POINT ( 'NONE',  ( 106.1764733795248219, -1.325403438956436419, -9.854619843455211026 ) ) ;
#9993 = CARTESIAN_POINT ( 'NONE',  ( 82.84913590756312374, -31.80416417093374193, -23.17682243723843527 ) ) ;
#9994 = CARTESIAN_POINT ( 'NONE',  ( 117.9016614775786280, -0.1624402480850797581, -16.17319339645315424 ) ) ;
#9995 = CARTESIAN_POINT ( 'NONE',  ( 119.6601881442453106, -1.833838273342659253, -17.42832698103878286 ) ) ;
#9996 = FACE_OUTER_BOUND ( 'NONE', #14627, .T. ) ;
#9997 = CARTESIAN_POINT ( 'NONE',  ( 120.2296266859119953, -0.06289925094097943703, -9.412459353600674206 ) ) ;
#9998 = CARTESIAN_POINT ( 'NONE',  ( 108.4684265045247997, -2.791137627527939813, -8.388885654883777576 ) ) ;
#9999 = ORIENTED_EDGE ( 'NONE', *, *, #19187, .T. ) ;
#10000 = DIRECTION ( 'NONE',  ( 0.000000000000000000, -0.9242245927363027524, -0.3818493186865928868 ) ) ;
#10001 = CARTESIAN_POINT ( 'NONE',  ( 113.3068014775786594, -8.166667518702817929, -8.995218007635859436 ) ) ;
#10002 = CARTESIAN_POINT ( 'NONE',  ( 123.1973327483929097, -2.423081321603731908, -17.89265170041263175 ) ) ;
#10003 = CARTESIAN_POINT ( 'NONE',  ( 122.9382985609119743, -0.08252387247370887580, -11.91645802438286417 ) ) ;
#10004 = CARTESIAN_POINT ( 'NONE',  ( 120.0212673109119805, -9.289237151508434209, -11.05642687123711276 ) ) ;
#10005 = ORIENTED_EDGE ( 'NONE', *, *, #33681, .F. ) ;
#10006 = CARTESIAN_POINT ( 'NONE',  ( 114.0246765045248196, -7.250697342233347165, -19.15521520033830427 ) ) ;
#10007 = VECTOR ( 'NONE', #44477, 1000.000000000000000 ) ;
#10008 = ORIENTED_EDGE ( 'NONE', *, *, #19286, .F. ) ;
#10009 = CARTESIAN_POINT ( 'NONE',  ( 123.5743281442453139, -7.893985811506177619, -18.51759400769804742 ) ) ;
#10010 = CARTESIAN_POINT ( 'NONE',  ( 126.6375681442452930, -10.15424416112533912, -14.75197769757731336 ) ) ;
#10011 = CARTESIAN_POINT ( 'NONE',  ( 118.8092881442453290, -0.1624402480850797581, -16.17319339645315424 ) ) ;
#10012 =( NAMED_UNIT ( * ) PLANE_ANGLE_UNIT ( ) SI_UNIT ( $, .RADIAN. ) );
#10013 = CARTESIAN_POINT ( 'NONE',  ( 85.75809888461174069, -18.45227461768569199, -4.893215200338314474 ) ) ;
#10014 = CARTESIAN_POINT ( 'NONE',  ( 122.4397948109119767, -9.988377603198976828, -10.36322818467138340 ) ) ;
#10015 = CARTESIAN_POINT ( 'NONE',  ( 116.5969481442453031, 0.5811942927096154232, -14.16772938898807155 ) ) ;
#10016 = CIRCLE ( 'NONE', #10717, 0.5000000000000004441 ) ;
#10017 = EDGE_CURVE ( 'NONE', #22169, #40557, #28361, .T. ) ;
#10018 = CARTESIAN_POINT ( 'NONE',  ( 106.1764733795248219, -1.325403438956436419, -9.854619843455211026 ) ) ;
#10019 = CARTESIAN_POINT ( 'NONE',  ( 113.3635281442453504, -0.1624402480850797581, -16.17319339645315424 ) ) ;
#10020 = CARTESIAN_POINT ( 'NONE',  ( 77.44400397045842510, -3.459648945705700473, -12.39321520033831447 ) ) ;
#10021 = ORIENTED_EDGE ( 'NONE', *, *, #37008, .F. ) ;
#10022 = CARTESIAN_POINT ( 'NONE',  ( 116.7104014775786425, -0.4660016031367893996, -10.09054647747474043 ) ) ;
#10023 = EDGE_CURVE ( 'NONE', #41036, #5448, #30538, .T. ) ;
#10024 = LINE ( 'NONE', #30979, #2355 ) ;
#10025 = EDGE_CURVE ( 'NONE', #23154, #34675, #13675, .T. ) ;
#10026 = CARTESIAN_POINT ( 'NONE',  ( 116.8238548109119819, -4.089484607189486809, -7.948022111789456723 ) ) ;
#10027 = ORIENTED_EDGE ( 'NONE', *, *, #34863, .T. ) ;
#10028 = DIRECTION ( 'NONE',  ( 1.000000000000000000, 0.000000000000000000, -0.000000000000000000 ) ) ;
#10030 = CARTESIAN_POINT ( 'NONE',  ( 2.384484203314607420, -10.01861149699890063, -17.89321520033831447 ) ) ;
#10029 = AXIS2_PLACEMENT_3D ( 'NONE', #33824, #2594, #8547 ) ;
#10031 = CARTESIAN_POINT ( 'NONE',  ( 125.2726254169155595, -6.179026137057662460, -18.60327543567144204 ) ) ;
#10032 = LINE ( 'NONE', #9567, #35277 ) ;
#10033 = CARTESIAN_POINT ( 'NONE',  ( 115.4056881442453459, -2.084020599724406786, -8.691656652584148546 ) ) ;
#10034 = DIRECTION ( 'NONE',  ( 0.9609149988134843001, -0.1028163501681632064, 0.2570431154366505933 ) ) ;
#10035 = CARTESIAN_POINT ( 'NONE',  ( 118.8660148109119774, 0.1319031606808879209, -14.10382304977623669 ) ) ;
#10036 = CARTESIAN_POINT ( 'NONE',  ( 74.69189222814998175, -41.76310523276723785, -6.393215200338315363 ) ) ;
#10037 = CARTESIAN_POINT ( 'NONE',  ( 116.2565881442453133, -0.8288870151387760510, -10.36305467784173118 ) ) ;
#10038 = ADVANCED_FACE ( 'NONE', ( #26368 ), #12996, .T. ) ;
#10039 = CARTESIAN_POINT ( 'NONE',  ( 113.8740681442453138, 0.5811942927096154232, -14.16772938898807155 ) ) ;
#10040 = CARTESIAN_POINT ( 'NONE',  ( 121.9659548109119811, -7.554583864224885481, -18.48844787311982785 ) ) ;
#10041 = CARTESIAN_POINT ( 'NONE',  ( 115.1787814775786387, -9.988377603198976828, -10.36322818467138340 ) ) ;
#10042 = CARTESIAN_POINT ( 'NONE',  ( 112.7962614775786676, -6.222761293078241884, -8.102969835052219238 ) ) ;
#10043 = EDGE_CURVE ( 'NONE', #34025, #2582, #25621, .T. ) ;
#10044 = EDGE_CURVE ( 'NONE', #44794, #9699, #8701, .T. ) ;
#10045 = TOROIDAL_SURFACE ( 'NONE', #35489, 5.500000000000000000, 0.5000000000000000000 ) ;
#10046 = CARTESIAN_POINT ( 'NONE',  ( 117.7314814775786260, -5.574606645277164318, -18.38911715685844683 ) ) ;
#10047 = EDGE_LOOP ( 'NONE', ( #34292, #25587, #15430, #22526, #39555 ) ) ;
#10048 = CARTESIAN_POINT ( 'NONE',  ( 112.9097148109120070, 0.2603800115204892296, -16.42320221600525088 ) ) ;
#10049 = CARTESIAN_POINT ( 'NONE',  ( 108.8851452545248151, 0.8980012041604421569, -11.00651665394454071 ) ) ;
#10050 = CARTESIAN_POINT ( 'NONE',  ( 106.8710046295248759, -4.863998795839590272, -18.39754474579285315 ) ) ;
#10051 = CARTESIAN_POINT ( 'NONE',  ( 87.44708369096657918, -23.44614552640564042, -8.393215200338314474 ) ) ;
#10052 = CARTESIAN_POINT ( 'NONE',  ( 94.20708369096698220, -25.99489077589524300, -13.39321520033831447 ) ) ;
#10053 = B_SPLINE_CURVE_WITH_KNOTS ( 'NONE', 3,
 ( #1078, #4266, #42586, #35261, #11800, #18856, #627, #1521, #38921, #25484 ),
 .UNSPECIFIED., .F., .F.,
 ( 4, 3, 3, 4 ),
 ( 7.296002358821220333E-16, 1.415135068336139897E-06, 2.830270136673649871E-06, 5.511645062456799864E-06 ),
 .UNSPECIFIED. ) ;
#10054 = CARTESIAN_POINT ( 'NONE',  ( 117.6180281442453150, -0.4660016031367893996, -10.09054647747474043 ) ) ;
#10055 = ORIENTED_EDGE ( 'NONE', *, *, #17740, .F. ) ;
#10056 = PLANE ( 'NONE',  #17599 ) ;
#10057 = CARTESIAN_POINT ( 'NONE',  ( 119.3198281442452924, -9.859900752359374465, -12.68260735090039404 ) ) ;
#10058 = CARTESIAN_POINT ( 'NONE',  ( 124.5059548109119731, -4.863998795839242995, -13.39321520033831447 ) ) ;
#10059 = CARTESIAN_POINT ( 'NONE',  ( 122.3830681442452857, -8.166667518702819706, -8.995218007635861213 ) ) ;
#10060 = CARTESIAN_POINT ( 'NONE',  ( 106.5931921295248372, 0.8980012041604618078, -13.39321520033831447 ) ) ;
#10061 = CARTESIAN_POINT ( 'NONE',  ( 89.29245855188943892, -9.882163754870950001, -13.29917559099935254 ) ) ;
#10062 = EDGE_LOOP ( 'NONE', ( #44352, #3324, #44313, #29892, #8402, #12885 ) ) ;
#10063 = CARTESIAN_POINT ( 'NONE',  ( 112.0020881442453344, 0.2603800115204892296, -16.42320221600525088 ) ) ;
#10064 = CARTESIAN_POINT ( 'NONE',  ( 121.1350814775786233, -9.859900752359378018, -12.68260735090039759 ) ) ;
#10065 = CARTESIAN_POINT ( 'NONE',  ( 125.1626748109119802, -9.988377603198980381, -10.36322818467138518 ) ) ;
#10066 = VECTOR ( 'NONE', #27308, 1000.000000000000000 ) ;
#10067 = CARTESIAN_POINT ( 'NONE',  ( 118.5256548109119876, -8.899110576539710493, -16.42337572283490132 ) ) ;
#10068 = CARTESIAN_POINT ( 'NONE',  ( 82.71771818927497577, -31.37104225293308701, -22.09381113811972597 ) ) ;
#10069 = CARTESIAN_POINT ( 'NONE',  ( 120.1140014775786398, -1.561330072975668504, -17.79121239304076951 ) ) ;
#10070 = LINE ( 'NONE', #14140, #37326 ) ;
#10071 = CARTESIAN_POINT ( 'NONE',  ( 126.5561942423832420, -1.182158702725811805, -9.765297139248401592 ) ) ;
#10072 = CARTESIAN_POINT ( 'NONE',  ( 122.2128881442453263, -7.643976991954077427, -18.09477374809248928 ) ) ;
#10073 = ORIENTED_EDGE ( 'NONE', *, *, #12505, .F. ) ;
#10074 = DIRECTION ( 'NONE',  ( 1.000000000000000000, 0.000000000000000000, 0.000000000000000000 ) ) ;
#10075 = CARTESIAN_POINT ( 'NONE',  ( 116.9373081442452929, -8.166667518702817929, -8.995218007635861213 ) ) ;
#10076 = CARTESIAN_POINT ( 'NONE',  ( 125.5030348109119558, -6.222761293078241884, -8.102969835052219238 ) ) ;
#10077 = ORIENTED_EDGE ( 'NONE', *, *, #20144, .F. ) ;
#10078 = CARTESIAN_POINT ( 'NONE',  ( 120.9241579359119925, -5.444069387712269226, -19.60292469916370450 ) ) ;
#10079 = CARTESIAN_POINT ( 'NONE',  ( 61.78823460971035786, -12.47025219434260457, -9.744219563062513245 ) ) ;
#10080 = CARTESIAN_POINT ( 'NONE',  ( 123.5743281442453139, -7.893985811506177619, -18.51759400769804742 ) ) ;
#10081 = CARTESIAN_POINT ( 'NONE',  ( 109.9269421295247753, 0.8980012041604618078, -13.39321520033831447 ) ) ;
#10082 = CARTESIAN_POINT ( 'NONE',  ( 118.6958348109119754, -3.505236298600246325, -18.68346056562440793 ) ) ;
#10083 = EDGE_LOOP ( 'NONE', ( #13664, #37109, #1456, #13469, #42028 ) ) ;
#10084 = VERTEX_POINT ( 'NONE', #11446 ) ;
#10085 = CARTESIAN_POINT ( 'NONE',  ( 112.2857214775786474, -4.089484607189486809, -7.948022111789456723 ) ) ;
#10086 = CARTESIAN_POINT ( 'NONE',  ( 124.7655881442452852, -9.859900752359378018, -12.68260735090039759 ) ) ;
#10087 = DIRECTION ( 'NONE',  ( -1.000000000000000000, 0.000000000000000000, -0.000000000000000000 ) ) ;
#10088 = EDGE_CURVE ( 'NONE', #12518, #7405, #7790, .T. ) ;
#10089 = CARTESIAN_POINT ( 'NONE',  ( 73.07463722459043254, -62.21038723923624048, -37.19243930338672754 ) ) ;
#10090 = CARTESIAN_POINT ( 'NONE',  ( 120.6245414775786458, -9.988377603198976828, -10.36322818467138340 ) ) ;
#10091 = CYLINDRICAL_SURFACE ( 'NONE', #41545, 0.5000000000000035527 ) ;
#10092 = AXIS2_PLACEMENT_3D ( 'NONE', #33006, #1556, #33237 ) ;
#10093 = CARTESIAN_POINT ( 'NONE',  ( 71.49305703095983233, -68.94143466658512409, -45.64354135182188799 ) ) ;
#10094 = CARTESIAN_POINT ( 'NONE',  ( 120.0005481442453146, -5.638512984488999180, -18.83840828888717311 ) ) ;
#10096 = CARTESIAN_POINT ( 'NONE',  ( 121.2485348109119769, -8.899110576539710493, -16.42337572283490132 ) ) ;
#10095 = CARTESIAN_POINT ( 'NONE',  ( 119.4900081442453086, -1.834011780172310813, -8.268836392978581529 ) ) ;
#10097 = CARTESIAN_POINT ( 'NONE',  ( 123.5176014775786228, -0.8288870151387760510, -10.36305467784173118 ) ) ;
#10098 = CARTESIAN_POINT ( 'NONE',  ( 115.4056881442453459, -7.893985811506177619, -18.51759400769804742 ) ) ;
#10099 = VERTEX_POINT ( 'NONE', #21699 ) ;
#10100 = CARTESIAN_POINT ( 'NONE',  ( 125.9001214775786224, -5.574606645277164318, -18.38911715685844683 ) ) ;
#10101 = LINE ( 'NONE', #38112, #6724 ) ;
#10102 = CARTESIAN_POINT ( 'NONE',  ( 108.3295202545248657, -10.62599879583958717, -15.77991374673208469 ) ) ;
#10103 = CARTESIAN_POINT ( 'NONE',  ( 115.0664733795247798, -1.325403438956436419, -9.854619843455211026 ) ) ;
#10104 = CARTESIAN_POINT ( 'NONE',  ( 109.3713171295247832, -10.62599879583958540, -13.39321520033831447 ) ) ;
#10105 = CARTESIAN_POINT ( 'NONE',  ( 121.9859814775786333, 0.2603800115204892296, -16.42320221600525088 ) ) ;
#10106 = CARTESIAN_POINT ( 'NONE',  ( 123.0070614775786169, -10.15424416112533912, -14.75197769757731336 ) ) ;
#10107 = ORIENTED_EDGE ( 'NONE', *, *, #22836, .F. ) ;
#10108 = CARTESIAN_POINT ( 'NONE',  ( 124.4819548109119722, -7.893985811506177619, -18.51759400769804742 ) ) ;
#10109 = CARTESIAN_POINT ( 'NONE',  ( 109.6491296295247793, -4.863998795839590272, -19.15521520033831493 ) ) ;
#10110 = CARTESIAN_POINT ( 'NONE',  ( 59.77099224207091765, -14.81899841792058048, -18.19321520033777162 ) ) ;
#10111 = ADVANCED_FACE ( 'NONE', ( #32173 ), #32621, .T. ) ;
#10112 = CARTESIAN_POINT ( 'NONE',  ( 123.5743281442453139, -7.893985811506177619, -18.51759400769804742 ) ) ;
#10113 = CARTESIAN_POINT ( 'NONE',  ( 122.0994348109119443, 0.9020085738987339008, -11.91225656197089222 ) ) ;
#10114 = DIRECTION ( 'NONE',  ( -0.9908103287288504424, 0.1352586133457950590, 0.000000000000000000 ) ) ;
#10115 = CARTESIAN_POINT ( 'NONE',  ( 126.4673881442452910, -7.894159318335828068, -9.358103419637847864 ) ) ;
#10116 = FACE_OUTER_BOUND ( 'NONE', #44753, .T. ) ;
#10117 = CARTESIAN_POINT ( 'NONE',  ( 114.0246765045248196, -2.791137627527939813, -8.388885654883777576 ) ) ;
#10118 = ORIENTED_EDGE ( 'NONE', *, *, #33114, .T. ) ;
#10119 = CARTESIAN_POINT ( 'NONE',  ( 61.69189222814998175, -64.41823023953081417, -19.25521411788945514 ) ) ;
#10120 = LINE ( 'NONE', #40670, #12172 ) ;
#10121 = CARTESIAN_POINT ( 'NONE',  ( 125.3328548109119964, -0.8288870151387760510, -10.36305467784173118 ) ) ;
#10122 = CARTESIAN_POINT ( 'NONE',  ( 109.6491296295247793, -4.863998795839590272, -8.388885654883775800 ) ) ;
#10123 = CARTESIAN_POINT ( 'NONE',  ( 108.8156921295247912, -9.868328341294093420, -13.39321520033831447 ) ) ;
#10124 = CARTESIAN_POINT ( 'NONE',  ( 122.4397948109119767, -0.1624402480850797581, -16.17319339645315424 ) ) ;
#10125 = CARTESIAN_POINT ( 'NONE',  ( 116.0864081442453113, -0.1624402480850797581, -16.17319339645315424 ) ) ;
#10126 = CARTESIAN_POINT ( 'NONE',  ( 112.0020881442453344, -9.565557343593413364, -10.61323700422348004 ) ) ;
#10127 = ORIENTED_EDGE ( 'NONE', *, *, #44846, .F. ) ;
#10128 = CARTESIAN_POINT ( 'NONE',  ( 125.3895814775786448, -2.084020599724406786, -8.691656652584148546 ) ) ;
#10129 = CARTESIAN_POINT ( 'NONE',  ( 117.0507614775786465, -10.30919188438810075, -12.61870101168855918 ) ) ;
#10130 = VECTOR ( 'NONE', #37797, 1000.000000000000000 ) ;
#10131 = DIRECTION ( 'NONE',  ( -0.8636456077245089347, 0.5040994586965589219, 0.000000000000000000 ) ) ;
#10132 = ORIENTED_EDGE ( 'NONE', *, *, #778, .T. ) ;
#10133 = CARTESIAN_POINT ( 'NONE',  ( -13.78505786849281911, -3.796669023460694792, -8.893215200338314474 ) ) ;
#10134 = EDGE_LOOP ( 'NONE', ( #6800, #43372, #6609, #23190, #35517, #2123, #32085, #34222, #10402, #35572, #13202 ) ) ;
#10135 = CARTESIAN_POINT ( 'NONE',  ( 115.4624148109119943, -4.153390946401321671, -8.397313243818183892 ) ) ;
#10136 = CARTESIAN_POINT ( 'NONE',  ( 114.6115148109119986, -6.222761293078241884, -8.102969835052219238 ) ) ;
#10137 = LINE ( 'NONE', #10578, #20238 ) ;
#10138 = CARTESIAN_POINT ( 'NONE',  ( 124.3273610609119686, -6.340755971794695078, -8.611740276972781771 ) ) ;
#10139 = VERTEX_POINT ( 'NONE', #39245 ) ;
#10140 = CARTESIAN_POINT ( 'NONE',  ( 70.19189222814998175, -51.68868231262963775, -33.87830190084585524 ) ) ;
#10141 = CARTESIAN_POINT ( 'NONE',  ( 114.6497546295247929, -4.863998795839590272, -7.631215200338315796 ) ) ;
#10142 = CARTESIAN_POINT ( 'NONE',  ( 121.4187148109119789, -3.505236298600246325, -18.68346056562440793 ) ) ;
#10143 = CARTESIAN_POINT ( 'NONE',  ( 114.4413348109119823, -0.8288870151387760510, -10.36305467784173118 ) ) ;
#10144 = CARTESIAN_POINT ( 'NONE',  ( 67.84197459855160162, -50.86926263129819148, -34.27970990073318802 ) ) ;
#10145 = ORIENTED_EDGE ( 'NONE', *, *, #10574, .F. ) ;
#10146 = CARTESIAN_POINT ( 'NONE',  ( 126.8848622761261993, -2.292895460366377591, -18.06601363898300860 ) ) ;
#10147 = CARTESIAN_POINT ( 'NONE',  ( 116.5564130180080866, 0.7607806665037644134, -14.64321520033833401 ) ) ;
#10148 = CARTESIAN_POINT ( 'NONE',  ( 112.9828796295247884, -4.863998795839590272, -19.15521520033831493 ) ) ;
#10149 = FACE_OUTER_BOUND ( 'NONE', #9320, .T. ) ;
#10151 = CARTESIAN_POINT ( 'NONE',  ( 84.77016061404391678, -26.60966817898065884, -11.90521360603286816 ) ) ;
#10150 = FACE_OUTER_BOUND ( 'NONE', #12800, .T. ) ;
#10152 = EDGE_CURVE ( 'NONE', #3839, #41752, #21823, .T. ) ;
#10153 = VECTOR ( 'NONE', #22268, 1000.000000000000000 ) ;
#10154 = CARTESIAN_POINT ( 'NONE',  ( 124.7088614775786226, -9.565557343593413364, -10.61323700422348004 ) ) ;
#10155 = ORIENTED_EDGE ( 'NONE', *, *, #28971, .F. ) ;
#10156 = CARTESIAN_POINT ( 'NONE',  ( 113.0231681442453322, 0.9020085738987339008, -11.91225656197089222 ) ) ;
#10157 = VECTOR ( 'NONE', #18097, 1000.000000000000000 ) ;
#10158 = CARTESIAN_POINT ( 'NONE',  ( 113.5841162859069016, -1.111561923218668646, -17.14115599315433869 ) ) ;
#10159 = CARTESIAN_POINT ( 'NONE',  ( 107.7738952545248310, -9.868328341294098749, -15.46607636864997204 ) ) ;
#10160 = CARTESIAN_POINT ( 'NONE',  ( 126.0703014775786102, -0.1624402480850797581, -16.17319339645315424 ) ) ;
#10161 = CARTESIAN_POINT ( 'NONE',  ( 123.1772414775786189, -5.574606645277164318, -18.38911715685844683 ) ) ;
#10162 = CARTESIAN_POINT ( 'NONE',  ( 95.62170725701103891, -25.82400229693143245, -12.45813257048188660 ) ) ;
#10163 = CARTESIAN_POINT ( 'NONE',  ( 110.5520202545248054, 0.1403307496149616695, -11.32035403202665336 ) ) ;
#10164 = CARTESIAN_POINT ( 'NONE',  ( 111.8021765045248372, -7.250697342233347165, -19.15521520033830427 ) ) ;
#10165 = DIRECTION ( 'NONE',  ( 1.000000000000000000, 0.000000000000000000, 0.000000000000000000 ) ) ;
#10166 = CARTESIAN_POINT ( 'NONE',  ( 113.7606148109119886, -7.894159318335828068, -9.358103419637847864 ) ) ;
#10167 = PLANE ( 'NONE',  #15280 ) ;
#10168 = CARTESIAN_POINT ( 'NONE',  ( 128.2184548109119930, -4.863998795839242995, -13.39321520033831447 ) ) ;
#10169 = CARTESIAN_POINT ( 'NONE',  ( 109.6491296295247793, -4.863998795839590272, -19.15521520033831493 ) ) ;
#10170 = CARTESIAN_POINT ( 'NONE',  ( 126.0135748109119902, -8.166667518702819706, -8.995218007635861213 ) ) ;
#10171 = CARTESIAN_POINT ( 'NONE',  ( 124.2550481442452792, -9.988377603198980381, -10.36322818467138518 ) ) ;
#10172 = CARTESIAN_POINT ( 'NONE',  ( 111.9664176093651804, 0.5600166689815611054, -14.64321520033831447 ) ) ;
#10173 = B_SPLINE_CURVE_WITH_KNOTS ( 'NONE', 3,
 ( #28938, #43294, #12064, #42623, #39649, #32566, #35760, #38959 ),
 .UNSPECIFIED., .F., .F.,
 ( 4, 2, 2, 4 ),
 ( 0.000000000000000000, 0.0001409761270367683526, 0.0002819522540735367052, 0.0005639045081470742777 ),
 .UNSPECIFIED. ) ;
#10174 = CARTESIAN_POINT ( 'NONE',  ( 119.5467348109119712, -4.089484607189486809, -7.948022111789456723 ) ) ;
#10175 = CARTESIAN_POINT ( 'NONE',  ( 117.1642148109119859, -9.261995988541697145, -16.69588392320189030 ) ) ;
#10176 = ORIENTED_EDGE ( 'NONE', *, *, #4713, .T. ) ;
#10177 = CARTESIAN_POINT ( 'NONE',  ( 111.8319081442453182, -4.153390946401321671, -8.397313243818183892 ) ) ;
#10178 = CARTESIAN_POINT ( 'NONE',  ( 124.3685014775786328, -10.63000616557722466, -14.87417383870573495 ) ) ;
#10180 = EDGE_CURVE ( 'NONE', #35146, #22099, #43119, .T. ) ;
#10179 = CARTESIAN_POINT ( 'NONE',  ( 113.7606148109119886, -1.561330072975668060, -17.79121239304076596 ) ) ;
#10181 = CARTESIAN_POINT ( 'NONE',  ( 115.8027748109119841, -8.899110576539710493, -16.42337572283490132 ) ) ;
#10182 = VERTEX_POINT ( 'NONE', #36264 ) ;
#10183 = CARTESIAN_POINT ( 'NONE',  ( 117.5613014775786525, -10.15424416112533912, -14.75197769757731336 ) ) ;
#10184 = CARTESIAN_POINT ( 'NONE',  ( 116.0864081442453113, -9.988377603198976828, -10.36322818467138340 ) ) ;
#10185 = AXIS2_PLACEMENT_3D ( 'NONE', #26704, #29897, #33981 ) ;
#10186 = CARTESIAN_POINT ( 'NONE',  ( 121.9292548109119849, -7.894159318335828068, -9.358103419637847864 ) ) ;
#10187 = CARTESIAN_POINT ( 'NONE',  ( 116.8576166310760556, -0.4515803448876515303, -16.26233397272304870 ) ) ;
#10188 = CARTESIAN_POINT ( 'NONE',  ( 113.8857702545248003, -10.62599879583958717, -15.77991374673208469 ) ) ;
#10189 = VERTEX_POINT ( 'NONE', #5032 ) ;
#10190 = DIRECTION ( 'NONE',  ( 0.000000000000000000, 0.000000000000000000, -1.000000000000000000 ) ) ;
#10191 = CARTESIAN_POINT ( 'NONE',  ( 124.8223148109119762, 0.9020085738987339008, -11.91225656197089222 ) ) ;
#10192 = CARTESIAN_POINT ( 'NONE',  ( 121.9470836909669913, -24.14644159042263993, -12.62951656296512937 ) ) ;
#10193 = B_SPLINE_CURVE_WITH_KNOTS ( 'NONE', 3,
 ( #43677, #18829, #26353, #40261, #4914, #19732, #22925, #30224, #43911, #36596 ),
 .UNSPECIFIED., .F., .F.,
 ( 4, 3, 3, 4 ),
 ( 8.673617379884039324E-19, 0.0001671877548681299829, 0.0003343755096277710101, 0.0006463528481650640013 ),
 .UNSPECIFIED. ) ;
#10194 = CIRCLE ( 'NONE', #22570, 2.999999999999999556 ) ;
#10195 = CARTESIAN_POINT ( 'NONE',  ( 86.75477599865929790, -26.60966817898065884, -11.90521360603286816 ) ) ;
#10196 = CARTESIAN_POINT ( 'NONE',  ( 112.9664414775786412, -9.859900752359374465, -12.68260735090039404 ) ) ;
#10197 = CARTESIAN_POINT ( 'NONE',  ( 106.4542858795248179, -8.402594152722688392, -9.854619843455216355 ) ) ;
#10198 = DIRECTION ( 'NONE',  ( 0.000000000000000000, -0.9242245927363028635, -0.3818493186865930533 ) ) ;
#10199 = CARTESIAN_POINT ( 'NONE',  ( 117.4478481442453131, 0.2603800115204892296, -16.42320221600525088 ) ) ;
#10200 = CARTESIAN_POINT ( 'NONE',  ( 69.91302804934421999, -34.85583393072344194, -5.893215200338315363 ) ) ;
#10201 = CARTESIAN_POINT ( 'NONE',  ( 69.69189222814998175, -41.76310523276723785, -6.393215200338315363 ) ) ;
#10202 = LINE ( 'NONE', #21118, #9081 ) ;
#10203 = CARTESIAN_POINT ( 'NONE',  ( 120.6812681442452941, 0.1319031606808879209, -14.10382304977623669 ) ) ;
#10204 = ORIENTED_EDGE ( 'NONE', *, *, #8323, .T. ) ;
#10205 = CARTESIAN_POINT ( 'NONE',  ( 125.2761281442453054, -10.63000616557722466, -14.87417383870573495 ) ) ;
#10206 = CARTESIAN_POINT ( 'NONE',  ( 119.4900081442453086, -1.834011780172310813, -8.268836392978581529 ) ) ;
#10207 = CARTESIAN_POINT ( 'NONE',  ( 68.56885555382550024, -20.41671115022304406, -14.39321520033831625 ) ) ;
#10208 = CARTESIAN_POINT ( 'NONE',  ( 114.1009748109119784, -5.574606645277164318, -18.38911715685844683 ) ) ;
#10209 = CARTESIAN_POINT ( 'NONE',  ( 111.3780948109119890, -5.574606645277164318, -18.38911715685844683 ) ) ;
#10210 = CARTESIAN_POINT ( 'NONE',  ( 109.8574890045247940, 0.8980012041604421569, -15.77991374673208469 ) ) ;
#10211 = DIRECTION ( 'NONE',  ( 0.000000000000000000, -0.9242245927363028635, -0.3818493186865927758 ) ) ;
#10212 = CARTESIAN_POINT ( 'NONE',  ( 83.32261893989519308, -31.98912039979894573, -23.53030018102887055 ) ) ;
#10213 = CARTESIAN_POINT ( 'NONE',  ( 117.3343948109119737, -6.222761293078241884, -8.102969835052219238 ) ) ;
#10214 = CARTESIAN_POINT ( 'NONE',  ( 120.3976348109119812, -7.643976991954077427, -18.09477374809248928 ) ) ;
#10215 = AXIS2_PLACEMENT_3D ( 'NONE', #25061, #429, #14346 ) ;
#10216 = CARTESIAN_POINT ( 'NONE',  ( 84.10862215250544693, -25.99489077589524300, -13.39321520033831625 ) ) ;
#10217 = CARTESIAN_POINT ( 'NONE',  ( 122.3826735609119680, 0.6414057260225851653, -11.69287257290600657 ) ) ;
#10218 = CARTESIAN_POINT ( 'NONE',  ( 108.2600671295247992, 0.1403307496149613920, -13.39321520033831447 ) ) ;
#10219 = CARTESIAN_POINT ( 'NONE',  ( 123.9714148109119805, -8.899110576539726480, -16.42337572283488001 ) ) ;
#10220 = CARTESIAN_POINT ( 'NONE',  ( 114.3846081442453197, -10.63000616557722466, -14.87417383870573495 ) ) ;
#10221 = CARTESIAN_POINT ( 'NONE',  ( 113.9307948109119906, 0.9020085738987339008, -11.91225656197089222 ) ) ;
#10222 = CARTESIAN_POINT ( 'NONE',  ( 122.5910329359119970, -5.367793381288652910, -18.78638297431638904 ) ) ;
#10223 = CARTESIAN_POINT ( 'NONE',  ( 122.2437673109119629, -9.289237151508434209, -11.05642687123711276 ) ) ;
#10224 = VERTEX_POINT ( 'NONE', #1605 ) ;
#10225 = DIRECTION ( 'NONE',  ( 0.000000000000000000, 0.3818493186865928868, -0.9242245927363029745 ) ) ;
#10226 = ORIENTED_EDGE ( 'NONE', *, *, #4690, .T. ) ;
#10227 = CARTESIAN_POINT ( 'NONE',  ( 122.0427081442452817, 0.5811942927096110934, -14.16772938898807510 ) ) ;
#10228 = VECTOR ( 'NONE', #33261, 1000.000000000000000 ) ;
#10229 = CARTESIAN_POINT ( 'NONE',  ( 113.6471614775786492, -5.638512984488999180, -18.83840828888717311 ) ) ;
#10230 = CARTESIAN_POINT ( 'NONE',  ( 119.8303681442453126, 0.4262465694468514643, -12.03445270309931736 ) ) ;
#10231 = VECTOR ( 'NONE', #23995, 1000.000000000000000 ) ;
#10232 = DIRECTION ( 'NONE',  ( -1.000000000000000000, 0.000000000000000000, 0.000000000000000000 ) ) ;
#10233 = CARTESIAN_POINT ( 'NONE',  ( 121.4187148109119789, -6.344957434206665248, -7.627207830600338134 ) ) ;
#10234 = CARTESIAN_POINT ( 'NONE',  ( 117.9016614775786280, -9.988377603198976828, -10.36322818467138340 ) ) ;
#10235 = CARTESIAN_POINT ( 'NONE',  ( 115.8999108795247821, -8.938348069036489818, -9.318865927141430916 ) ) ;
#10236 = CARTESIAN_POINT ( 'NONE',  ( 126.0135748109119902, -8.166667518702819706, -8.995218007635861213 ) ) ;
#10237 = CARTESIAN_POINT ( 'NONE',  ( 135.3184548109119874, -4.863998795839242995, -13.39321520033831447 ) ) ;
#10238 = ORIENTED_EDGE ( 'NONE', *, *, #36629, .F. ) ;
#10239 = CARTESIAN_POINT ( 'NONE',  ( 117.4478481442453131, 0.2603800115204892296, -16.42320221600525088 ) ) ;
#10240 = EDGE_CURVE ( 'NONE', #11904, #33939, #44391, .T. ) ;
#10241 = CARTESIAN_POINT ( 'NONE',  ( 120.7157985609119635, -10.36940331770106916, -15.09355782777062061 ) ) ;
#10242 = CARTESIAN_POINT ( 'NONE',  ( 115.4056881442453459, -7.893985811506177619, -18.51759400769804742 ) ) ;
#10243 = ORIENTED_EDGE ( 'NONE', *, *, #5222, .F. ) ;
#10244 = CARTESIAN_POINT ( 'NONE',  ( 114.4413952545248350, 0.8980012041604421569, -11.00651665394454071 ) ) ;
#10245 = CARTESIAN_POINT ( 'NONE',  ( 125.6164881442453094, 0.2603800115204892296, -16.42320221600525088 ) ) ;
#10246 = CIRCLE ( 'NONE', #17521, 2.445500000000004448 ) ;
#10247 = DIRECTION ( 'NONE',  ( 1.000000000000000000, 0.000000000000000000, -0.000000000000000000 ) ) ;
#10248 = CARTESIAN_POINT ( 'NONE',  ( 112.2857214775786474, -5.574606645277164318, -18.38911715685844683 ) ) ;
#10249 = DIRECTION ( 'NONE',  ( 1.000000000000000000, 0.000000000000000000, 0.000000000000000000 ) ) ;
#10250 = CARTESIAN_POINT ( 'NONE',  ( 115.6893214775786447, -9.859900752359374465, -12.68260735090039404 ) ) ;
#10251 = CARTESIAN_POINT ( 'NONE',  ( 86.34560043013698305, -9.320000780048239619, -14.14321520033831625 ) ) ;
#10252 = CARTESIAN_POINT ( 'NONE',  ( 116.5969481442453031, -9.859900752359374465, -12.68260735090039404 ) ) ;
#10253 = CONICAL_SURFACE ( 'NONE', #12429, 2.445500000000004448, 0.9599310885968757034 ) ;
#10254 = DIRECTION ( 'NONE',  ( -0.4461977533474357216, 0.8271203734159379151, 0.3417300876246931463 ) ) ;
#10255 = CARTESIAN_POINT ( 'NONE',  ( 116.9373081442452929, -1.833838273342659253, -17.42832698103878286 ) ) ;
#10256 = CARTESIAN_POINT ( 'NONE',  ( 121.7575954359119805, -11.07370829466463569, -12.81314460846529002 ) ) ;
#10257 = CARTESIAN_POINT ( 'NONE',  ( 115.6325948109119821, 0.2603800115204892296, -16.42320221600525088 ) ) ;
#10258 = CARTESIAN_POINT ( 'NONE',  ( 111.8319081442453182, -4.153390946401321671, -8.397313243818183892 ) ) ;
#10259 = CARTESIAN_POINT ( 'NONE',  ( 116.7671281442453335, -7.643976991954077427, -18.09477374809248928 ) ) ;
#10260 = ORIENTED_EDGE ( 'NONE', *, *, #5598, .T. ) ;
#10261 = CARTESIAN_POINT ( 'NONE',  ( 116.4267681442453153, -3.383040157471821630, -19.15922257007629170 ) ) ;
#10262 = CARTESIAN_POINT ( 'NONE',  ( 108.0517077545248696, -7.250697342233347165, -7.631215200338321125 ) ) ;
#10263 = EDGE_CURVE ( 'NONE', #28337, #21924, #24894, .T. ) ;
#10264 = CARTESIAN_POINT ( 'NONE',  ( 106.3153796295248412, -4.863998795839590272, -8.388885654883775800 ) ) ;
#10265 = CARTESIAN_POINT ( 'NONE',  ( 106.0375671295248310, 0.1403307496149613920, -13.39321520033831447 ) ) ;
#10266 = DIRECTION ( 'NONE',  ( 0.000000000000000000, 0.000000000000000000, 1.000000000000000000 ) ) ;
#10267 = CARTESIAN_POINT ( 'NONE',  ( 121.1918081442452859, 0.9020085738987339008, -11.91225656197089222 ) ) ;
#10268 = ORIENTED_EDGE ( 'NONE', *, *, #6757, .T. ) ;
#10269 = CARTESIAN_POINT ( 'NONE',  ( 2.181596283295915484, -11.50482699009217669, -19.39321520033831447 ) ) ;
#10270 = CARTESIAN_POINT ( 'NONE',  ( 116.8238548109119819, -5.574606645277164318, -18.38911715685844683 ) ) ;
#10271 = ADVANCED_FACE ( 'NONE', ( #4132 ), #3653, .T. ) ;
#10272 = CARTESIAN_POINT ( 'NONE',  ( 123.8411891859119862, -8.844754642576873493, -8.592115655440052180 ) ) ;
#10273 = CARTESIAN_POINT ( 'NONE',  ( 121.9859814775786333, 0.2603800115204892296, -16.42320221600525088 ) ) ;
#10274 = EDGE_CURVE ( 'NONE', #27202, #16290, #38187, .T. ) ;
#10275 = CARTESIAN_POINT ( 'NONE',  ( 107.0793640045248196, -10.62599879583958717, -11.00651665394454604 ) ) ;
#10276 = CARTESIAN_POINT ( 'NONE',  ( 124.4756362859068872, -1.111561923218658210, -17.14115599315433158 ) ) ;
#10277 = ORIENTED_EDGE ( 'NONE', *, *, #42588, .F. ) ;
#10278 = DIRECTION ( 'NONE',  ( 1.000000000000000000, 0.000000000000000000, 0.000000000000000000 ) ) ;
#10279 = CARTESIAN_POINT ( 'NONE',  ( 125.5030348109119558, -6.222761293078241884, -8.102969835052219238 ) ) ;
#10280 = CARTESIAN_POINT ( 'NONE',  ( 124.3117748109119844, -10.30919188438810075, -12.61870101168855918 ) ) ;
#10281 = AXIS2_PLACEMENT_3D ( 'NONE', #35520, #28257, #7056 ) ;
#10282 = CARTESIAN_POINT ( 'NONE',  ( 118.1852948109119836, -4.153390946401325223, -8.397313243818185668 ) ) ;
#10283 = CARTESIAN_POINT ( 'NONE',  ( 84.77016061404391678, -25.99489077589524300, -13.39321520033831625 ) ) ;
#10284 = CARTESIAN_POINT ( 'NONE',  ( 120.6812681442452941, -10.30919188438810075, -12.61870101168855918 ) ) ;
#10285 = DIRECTION ( 'NONE',  ( -0.8949343913984424415, 0.1703803081152067966, -0.4123869368673871993 ) ) ;
#10286 = CARTESIAN_POINT ( 'NONE',  ( 121.2485348109119769, -8.899110576539710493, -16.42337572283490132 ) ) ;
#10287 = VERTEX_POINT ( 'NONE', #9946 ) ;
#10288 = EDGE_CURVE ( 'NONE', #38132, #10759, #12060, .T. ) ;
#10289 = DIRECTION ( 'NONE',  ( 0.000000000000000000, 0.000000000000000000, -1.000000000000000000 ) ) ;
#10290 = CARTESIAN_POINT ( 'NONE',  ( 115.4624148109119943, -5.638512984488999180, -18.83840828888717311 ) ) ;
#10291 = CARTESIAN_POINT ( 'NONE',  ( 125.6732148109119862, -9.859900752359378018, -12.68260735090039759 ) ) ;
#10292 = ORIENTED_EDGE ( 'NONE', *, *, #33887, .F. ) ;
#10293 = CIRCLE ( 'NONE', #1446, 1.499999999999998002 ) ;
#10294 = PRODUCT ( 'Adjuster Locknut', 'Adjuster Locknut', '', ( #7685 ) ) ;
#10295 = EDGE_CURVE ( 'NONE', #14305, #30603, #2138, .T. ) ;
#10296 = CARTESIAN_POINT ( 'NONE',  ( 122.7299391859119737, -8.844754642576884152, -8.592115655440050404 ) ) ;
#10297 = CARTESIAN_POINT ( 'NONE',  ( 137.1399781294065576, -1.251936845180553481, -9.436198808430885876 ) ) ;
#10298 = ADVANCED_FACE ( 'NONE', ( #18118 ), #28836, .T. ) ;
#10299 = EDGE_CURVE ( 'NONE', #38311, #574, #24959, .T. ) ;
#10300 = CARTESIAN_POINT ( 'NONE',  ( 121.7023481442452777, -9.261995988541697145, -16.69588392320189030 ) ) ;
#10301 = CARTESIAN_POINT ( 'NONE',  ( 108.1211608795247798, -8.938348069036489818, -9.318865927141430916 ) ) ;
#10302 = CARTESIAN_POINT ( 'NONE',  ( 120.0572748109119772, -6.222761293078241884, -8.102969835052219238 ) ) ;
#10303 = VERTEX_POINT ( 'NONE', #24730 ) ;
#10304 = ORIENTED_EDGE ( 'NONE', *, *, #14423, .T. ) ;
#10305 = CARTESIAN_POINT ( 'NONE',  ( 114.5547881442453217, -5.638512984488999180, -18.83840828888717311 ) ) ;
#10306 = CARTESIAN_POINT ( 'NONE',  ( 124.8790414775786246, -8.899110576539710493, -16.42337572283490132 ) ) ;
#10307 = SURFACE_STYLE_FILL_AREA ( #13274 ) ;
#10308 = CARTESIAN_POINT ( 'NONE',  ( 59.36680634945873436, -12.84644995903807541, -9.393215200338314474 ) ) ;
#10309 = CARTESIAN_POINT ( 'NONE',  ( 123.5743281442453139, -7.893985811506177619, -18.51759400769804742 ) ) ;
#10310 = DIRECTION ( 'NONE',  ( 0.000000000000000000, 0.000000000000000000, 1.000000000000000000 ) ) ;
#10311 = DIRECTION ( 'NONE',  ( 0.9609149988134838560, -0.1028163501681645386, 0.2570431154366520921 ) ) ;
#10312 = CARTESIAN_POINT ( 'NONE',  ( 119.6601881442453106, -8.166667518702819706, -8.995218007635861213 ) ) ;
#10314 = CARTESIAN_POINT ( 'NONE',  ( 120.9649014775786355, -6.222761293078241884, -8.102969835052219238 ) ) ;
#10313 = CARTESIAN_POINT ( 'NONE',  ( 119.3765548109119834, 0.9020085738987339008, -11.91225656197089222 ) ) ;
#10315 = DIRECTION ( 'NONE',  ( 0.000000000000000000, 0.000000000000000000, 1.000000000000000000 ) ) ;
#10316 = CARTESIAN_POINT ( 'NONE',  ( 117.7882081442453170, -6.344957434206665248, -7.627207830600338134 ) ) ;
#10317 = ORIENTED_EDGE ( 'NONE', *, *, #40402, .F. ) ;
#10318 = CARTESIAN_POINT ( 'NONE',  ( 125.4463081442452932, -4.153390946401325223, -8.397313243818185668 ) ) ;
#10319 = CARTESIAN_POINT ( 'NONE',  ( 72.51188087854242781, -21.10583385764521225, -7.393215200338315363 ) ) ;
#10320 = CARTESIAN_POINT ( 'NONE',  ( 110.4131140045248287, -10.62599879583958717, -11.00651665394454604 ) ) ;
#10321 = VECTOR ( 'NONE', #5256, 1000.000000000000227 ) ;
#10322 = CARTESIAN_POINT ( 'NONE',  ( 108.2600671295247992, 0.1403307496149613920, -13.39321520033831447 ) ) ;
#10323 = CARTESIAN_POINT ( 'NONE',  ( 105.6903015045248253, -2.477300249445798297, -7.631215200338321125 ) ) ;
#10324 = DIRECTION ( 'NONE',  ( -1.000000000000000000, 0.000000000000000000, 0.000000000000000000 ) ) ;
#10325 = CARTESIAN_POINT ( 'NONE',  ( 113.1366214775786432, -1.834011780172310813, -8.268836392978581529 ) ) ;
#10326 = ORIENTED_EDGE ( 'NONE', *, *, #35612, .T. ) ;
#10327 = CARTESIAN_POINT ( 'NONE',  ( 124.7088614775786226, 0.2603800115204892296, -16.42320221600525088 ) ) ;
#10328 = CARTESIAN_POINT ( 'NONE',  ( 109.5102233795247884, -8.938348069036489818, -17.46756447353520159 ) ) ;
#10329 = DIRECTION ( 'NONE',  ( -0.000000000000000000, -0.9284778069183721172, -0.3713878862591650232 ) ) ;
#10330 = CARTESIAN_POINT ( 'NONE',  ( 122.3830681442452857, -8.166667518702819706, -8.995218007635861213 ) ) ;
#10331 = CARTESIAN_POINT ( 'NONE',  ( 124.2550481442452792, -9.988377603198980381, -10.36322818467138518 ) ) ;
#10332 = CARTESIAN_POINT ( 'NONE',  ( 120.1601735609119856, -9.645473719204776586, -14.86997237629376656 ) ) ;
#10333 = CARTESIAN_POINT ( 'NONE',  ( 126.1837548109119496, 0.4262465694468514643, -12.03445270309931736 ) ) ;
#10334 = CARTESIAN_POINT ( 'NONE',  ( 70.19189222814998175, -58.54852247098141049, -36.62221405200617141 ) ) ;
#10335 = CARTESIAN_POINT ( 'NONE',  ( 107.0793640045248196, -10.62599879583958717, -11.00651665394454604 ) ) ;
#10336 = VERTEX_POINT ( 'NONE', #38401 ) ;
#10337 = DIRECTION ( 'NONE',  ( 0.9609149988134843001, -0.1028163501681632064, 0.2570431154366505933 ) ) ;
#10338 = CARTESIAN_POINT ( 'NONE',  ( 115.1787814775786387, -0.1624402480850797581, -16.17319339645315424 ) ) ;
#10339 = CARTESIAN_POINT ( 'NONE',  ( 113.4202548109119846, -10.30919188438810075, -12.61870101168855918 ) ) ;
#10340 = CARTESIAN_POINT ( 'NONE',  ( 115.2748327545248657, -2.477300249445798297, -19.15521520033831138 ) ) ;
#10341 = CARTESIAN_POINT ( 'NONE',  ( 105.4124890045248293, -9.868328341294098749, -11.32035403202665869 ) ) ;
#10342 = CARTESIAN_POINT ( 'NONE',  ( 121.0216281442452981, -7.894159318335828068, -9.358103419637847864 ) ) ;
#10343 = CARTESIAN_POINT ( 'NONE',  ( 116.4834948109119779, -7.894159318335828068, -9.358103419637847864 ) ) ;
#10344 = CARTESIAN_POINT ( 'NONE',  ( 126.1270281442452870, -10.30919188438810075, -12.61870101168855918 ) ) ;
#10345 = ORIENTED_EDGE ( 'NONE', *, *, #33987, .F. ) ;
#10346 = CARTESIAN_POINT ( 'NONE',  ( 124.9924948109119924, -5.574606645277164318, -18.38911715685844683 ) ) ;
#10347 = CARTESIAN_POINT ( 'NONE',  ( 125.3328548109119964, -0.8288870151387760510, -10.36305467784173118 ) ) ;
#10348 = CARTESIAN_POINT ( 'NONE',  ( 113.8173414775786512, -9.565557343593413364, -10.61323700422348004 ) ) ;
#10349 = ORIENTED_EDGE ( 'NONE', *, *, #26741, .T. ) ;
#10350 = DIRECTION ( 'NONE',  ( -0.000000000000000000, -0.9284778069183721172, -0.3713878862591650232 ) ) ;
#10351 = EDGE_CURVE ( 'NONE', #10826, #32113, #12637, .T. ) ;
#10352 = VECTOR ( 'NONE', #4520, 1000.000000000000000 ) ;
#10353 = ORIENTED_EDGE ( 'NONE', *, *, #39824, .T. ) ;
#10354 = CARTESIAN_POINT ( 'NONE',  ( 119.9438214775786378, -2.084020599724406786, -8.691656652584148546 ) ) ;
#10355 = CARTESIAN_POINT ( 'NONE',  ( 113.5337081442453240, -0.8288870151387760510, -10.36305467784173118 ) ) ;
#10356 = ADVANCED_FACE ( 'NONE', ( #21313 ), #10613, .T. ) ;
#10357 = PRODUCT_DEFINITION ( 'UNKNOWN', '', #35863, #15095 ) ;
#10358 = DIRECTION ( 'NONE',  ( -1.000000000000000000, 0.000000000000000000, 0.000000000000000000 ) ) ;
#10359 = CARTESIAN_POINT ( 'NONE',  ( 121.2714235609119697, -9.645473719204776586, -14.86997237629376656 ) ) ;
#10360 = ORIENTED_EDGE ( 'NONE', *, *, #295, .T. ) ;
#10361 = DIRECTION ( 'NONE',  ( 0.9609149988134843001, -0.1028163501681632064, 0.2570431154366505933 ) ) ;
#10362 = CARTESIAN_POINT ( 'NONE',  ( 123.9584548109119737, 3.074545301078819737, -12.40350937470759973 ) ) ;
#10363 = CARTESIAN_POINT ( 'NONE',  ( 115.1359265045248605, -7.250697342233347165, -19.15521520033831138 ) ) ;
#10364 = CARTESIAN_POINT ( 'NONE',  ( 115.3442858795247759, -8.402594152722736354, -9.854619843455244776 ) ) ;
#10365 = CARTESIAN_POINT ( 'NONE',  ( 123.2906948109119867, -1.833838273342659697, -17.42832698103878286 ) ) ;
#10366 = CARTESIAN_POINT ( 'NONE',  ( 117.6180281442453150, -8.899110576539710493, -16.42337572283490132 ) ) ;
#10367 = CARTESIAN_POINT ( 'NONE',  ( 120.0157737256648858, -1.063912429576147511, -17.20460841810472985 ) ) ;
#10368 = ORIENTED_EDGE ( 'NONE', *, *, #43404, .T. ) ;
#10369 = DIRECTION ( 'NONE',  ( -1.000000000000000000, 0.000000000000000000, 0.000000000000000000 ) ) ;
#10370 = CARTESIAN_POINT ( 'NONE',  ( 114.8951481442453115, -8.899110576539710493, -16.42337572283490132 ) ) ;
#10371 = CIRCLE ( 'NONE', #24206, 4.999999999999998224 ) ;
#10372 = CARTESIAN_POINT ( 'NONE',  ( 67.69189222814998175, -55.76310523276723785, -40.89321520033831092 ) ) ;
#10373 = CARTESIAN_POINT ( 'NONE',  ( 125.9001214775786224, -4.089484607189486809, -7.948022111789456723 ) ) ;
#10374 = CARTESIAN_POINT ( 'NONE',  ( 111.8886348109120092, -3.383040157471821630, -19.15922257007629170 ) ) ;
#10375 = EDGE_LOOP ( 'NONE', ( #2289, #25120, #18961, #10801 ) ) ;
#10376 = CARTESIAN_POINT ( 'NONE',  ( 115.1220548109119761, -8.166667518702817929, -8.995218007635861213 ) ) ;
#10377 = FACE_OUTER_BOUND ( 'NONE', #9362, .T. ) ;
#10378 = CARTESIAN_POINT ( 'NONE',  ( 106.2459265045248173, -2.791137627527939813, -8.388885654883777576 ) ) ;
#10379 = CARTESIAN_POINT ( 'NONE',  ( 126.5808414775786446, -9.859900752359378018, -12.68260735090039759 ) ) ;
#10380 = CARTESIAN_POINT ( 'NONE',  ( 115.6893214775786447, 0.5811942927096154232, -14.16772938898807155 ) ) ;
#10381 = CARTESIAN_POINT ( 'NONE',  ( 125.1626748109119802, -0.1624402480850797581, -16.17319339645315424 ) ) ;
#10382 = CARTESIAN_POINT ( 'NONE',  ( 94.20708369096698220, -25.77760949922539879, -12.57042127303408385 ) ) ;
#10383 = CARTESIAN_POINT ( 'NONE',  ( 109.5796765045248122, -2.791137627527939813, -8.388885654883777576 ) ) ;
#10384 = AXIS2_PLACEMENT_3D ( 'NONE', #19366, #33708, #15952 ) ;
#10385 = CARTESIAN_POINT ( 'NONE',  ( 117.3719165460472027, -2.191907684172563986, -18.20049396185734025 ) ) ;
#10386 = CARTESIAN_POINT ( 'NONE',  ( 109.2295573004754061, -4.817128553740947616, -18.58155556397246500 ) ) ;
#10387 = CARTESIAN_POINT ( 'NONE',  ( 117.8449348109119938, -1.833838273342659253, -17.42832698103878286 ) ) ;
#10388 = CARTESIAN_POINT ( 'NONE',  ( 106.5237390045248418, 0.8980012041604421569, -15.77991374673208469 ) ) ;
#10389 = CARTESIAN_POINT ( 'NONE',  ( 77.22947525540432423, -44.03086066871760096, -4.893215200338314474 ) ) ;
#10390 = CARTESIAN_POINT ( 'NONE',  ( 109.0240515045248202, -2.477300249445798297, -7.631215200338321125 ) ) ;
#10391 = CARTESIAN_POINT ( 'NONE',  ( 126.2404814775786264, -9.261995988541697145, -16.69588392320189030 ) ) ;
#10392 = CARTESIAN_POINT ( 'NONE',  ( 111.4915481442453142, -1.833838273342658365, -17.42832698103878286 ) ) ;
#10393 = CARTESIAN_POINT ( 'NONE',  ( 120.1140014775786398, -7.894159318335804976, -9.358103419637831877 ) ) ;
#10394 = CARTESIAN_POINT ( 'NONE',  ( 119.1496481442453046, -3.383040157471821630, -19.15922257007629170 ) ) ;
#10395 = CARTESIAN_POINT ( 'NONE',  ( 114.5547881442453217, -5.638512984488999180, -18.83840828888717311 ) ) ;
#10397 = ORIENTED_EDGE ( 'NONE', *, *, #3274, .F. ) ;
#10396 = EDGE_CURVE ( 'NONE', #12781, #38164, #21537, .T. ) ;
#10398 = CARTESIAN_POINT ( 'NONE',  ( 115.1787814775786387, -0.1624402480850797581, -16.17319339645315424 ) ) ;
#10399 = CARTESIAN_POINT ( 'NONE',  ( 123.8012348109119642, 0.2603800115204892296, -16.42320221600525088 ) ) ;
#10400 = CARTESIAN_POINT ( 'NONE',  ( 113.8740681442453138, 0.5811942927096154232, -14.16772938898807155 ) ) ;
#10401 = CARTESIAN_POINT ( 'NONE',  ( 115.0086014775786509, -5.574606645277164318, -18.38911715685844683 ) ) ;
#10402 = ORIENTED_EDGE ( 'NONE', *, *, #26420, .F. ) ;
#10403 = CARTESIAN_POINT ( 'NONE',  ( 120.8514481442452961, -2.084020599724406786, -8.691656652584148546 ) ) ;
#10404 = B_SPLINE_CURVE_WITH_KNOTS ( 'NONE', 3,
 ( #41221, #30261, #5854, #19777, #33659, #23661, #2436, #23432, #44187, #9979 ),
 .UNSPECIFIED., .F., .F.,
 ( 4, 3, 3, 4 ),
 ( 5.023252700711280216E-16, 1.701546542442415166E-05, 3.403093084891979967E-05, 6.554879158867139171E-05 ),
 .UNSPECIFIED. ) ;
#10405 = AXIS2_PLACEMENT_3D ( 'NONE', #14464, #24507, #18109 ) ;
#10406 = CARTESIAN_POINT ( 'NONE',  ( 116.1998614775786507, -10.63000616557722466, -14.87417383870573495 ) ) ;
#10407 = EDGE_CURVE ( 'NONE', #39007, #42235, #1138, .T. ) ;
#10408 = CARTESIAN_POINT ( 'NONE',  ( 116.8252617111891993, -1.616627641789968317, -17.49395584329565523 ) ) ;
#10409 = CARTESIAN_POINT ( 'NONE',  ( 115.7610046295247912, -4.863998795839590272, -7.631215200338315796 ) ) ;
#10410 = ORIENTED_EDGE ( 'NONE', *, *, #9789, .T. ) ;
#10411 =( GEOMETRIC_REPRESENTATION_CONTEXT ( 3 ) GLOBAL_UNCERTAINTY_ASSIGNED_CONTEXT ( ( #11459 ) ) GLOBAL_UNIT_ASSIGNED_CONTEXT ( ( #4260, #18178, #18849 ) ) REPRESENTATION_CONTEXT ( 'NONE', 'WORKASPACE' ) );
#10412 = CARTESIAN_POINT ( 'NONE',  ( 69.36136150295220659, -59.05115674483842270, -33.71845836089322290 ) ) ;
#10413 = CARTESIAN_POINT ( 'NONE',  ( 125.6732148109119862, 0.5811942927096110934, -14.16772938898807510 ) ) ;
#10414 = DIRECTION ( 'NONE',  ( -0.9495615000563050190, 0.3135808629537517600, 0.000000000000000000 ) ) ;
#10415 = VECTOR ( 'NONE', #27740, 1000.000000000000000 ) ;
#10416 = CARTESIAN_POINT ( 'NONE',  ( 115.0086014775786509, -4.089484607189486809, -7.948022111789456723 ) ) ;
#10417 = CARTESIAN_POINT ( 'NONE',  ( 135.8419766445594234, -10.77193394454819320, -14.12650746913758937 ) ) ;
#10418 = LINE ( 'NONE', #9974, #18547 ) ;
#10419 = CARTESIAN_POINT ( 'NONE',  ( 62.84522113422936940, -12.57561100918773178, -16.63017181072184769 ) ) ;
#10420 = CARTESIAN_POINT ( 'NONE',  ( 115.5950730757767531, -0.9924539043446216624, -17.29976612834909133 ) ) ;
#10421 = CARTESIAN_POINT ( 'NONE',  ( 113.5385046295247804, -4.863998795839590272, -18.39754474579285315 ) ) ;
#10422 = CARTESIAN_POINT ( 'NONE',  ( 119.2631014775786298, 0.2603800115204892296, -16.42320221600525088 ) ) ;
#10423 = PRESENTATION_STYLE_ASSIGNMENT (( #7202 ) ) ;
#10424 = CARTESIAN_POINT ( 'NONE',  ( 111.5491077074049002, -2.419733177069675722, -17.89711025544712086 ) ) ;
#10425 = CARTESIAN_POINT ( 'NONE',  ( 109.2294421295247844, 0.8460904216231607267, -7.393215200338315363 ) ) ;
#10426 = CARTESIAN_POINT ( 'NONE',  ( 121.3619881442452879, -5.574606645277164318, -18.38911715685844683 ) ) ;
#10427 = VERTEX_POINT ( 'NONE', #336 ) ;
#10428 = LINE ( 'NONE', #10648, #33316 ) ;
#10429 = CARTESIAN_POINT ( 'NONE',  ( 119.9438214775786378, -7.893985811506177619, -18.51759400769804742 ) ) ;
#10430 = DIRECTION ( 'NONE',  ( 0.000000000000000000, 0.9242245927363041957, 0.3818493186865896116 ) ) ;
#10431 = CARTESIAN_POINT ( 'NONE',  ( 116.0296814775786345, -1.833838273342658809, -17.42832698103878286 ) ) ;
#10433 = CARTESIAN_POINT ( 'NONE',  ( 111.3213681442453264, -7.643976991954077427, -18.09477374809248928 ) ) ;
#10432 = CIRCLE ( 'NONE', #34428, 3.000000000000001776 ) ;
#10434 = CARTESIAN_POINT ( 'NONE',  ( 105.0652233795248378, -1.325403438956436419, -9.854619843455211026 ) ) ;
#10435 = CARTESIAN_POINT ( 'NONE',  ( 111.5243640045248412, -10.62599879583958717, -11.00651665394454604 ) ) ;
#10436 = CARTESIAN_POINT ( 'NONE',  ( 121.4187148109119789, -3.505236298600246325, -18.68346056562440793 ) ) ;
#10437 = AXIS2_PLACEMENT_3D ( 'NONE', #30174, #24836, #31444 ) ;
#10438 = CARTESIAN_POINT ( 'NONE',  ( 121.9859814775786333, -9.565557343593413364, -10.61323700422348004 ) ) ;
#10439 = DIRECTION ( 'NONE',  ( 0.000000000000000000, 0.000000000000000000, -1.000000000000000000 ) ) ;
#10440 = CARTESIAN_POINT ( 'NONE',  ( 122.5215798109119874, -2.173413727453600508, -8.297982527556802879 ) ) ;
#10441 = B_SPLINE_CURVE_WITH_KNOTS ( 'NONE', 3,
 ( #11555, #9031, #29999, #22703, #36151, #32507, #25463, #43466 ),
 .UNSPECIFIED., .F., .F.,
 ( 4, 2, 2, 4 ),
 ( 0.000000000000000000, 0.0002795070773440827094, 0.0004192606160161267475, 0.0005590141546881708398 ),
 .UNSPECIFIED. ) ;
#10442 = CARTESIAN_POINT ( 'NONE',  ( 107.3571765045248299, -2.791137627527939813, -8.388885654883777576 ) ) ;
#10443 = DIRECTION ( 'NONE',  ( 0.000000000000000000, 0.000000000000000000, -1.000000000000000000 ) ) ;
#10444 = CARTESIAN_POINT ( 'NONE',  ( 113.2500748109119968, -6.344957434206662583, -7.627207830600332805 ) ) ;
#10445 = CARTESIAN_POINT ( 'NONE',  ( 116.0296814775786345, -8.166667518702817929, -8.995218007635861213 ) ) ;
#10446 = CARTESIAN_POINT ( 'NONE',  ( 122.8688454359119646, 0.5291689781388270175, -13.89700978578772705 ) ) ;
#10447 = VERTEX_POINT ( 'NONE', #5486 ) ;
#10448 = CARTESIAN_POINT ( 'NONE',  ( 123.5944003412206484, -3.153399869360316909, -14.42216642652626746 ) ) ;
#10449 = AXIS2_PLACEMENT_3D ( 'NONE', #36622, #36395, #9052 ) ;
#10450 = CARTESIAN_POINT ( 'NONE',  ( 121.0216281442452981, -1.561330072975668948, -17.79121239304076951 ) ) ;
#10451 = CARTESIAN_POINT ( 'NONE',  ( 113.3068014775786594, -8.166667518702817929, -8.995218007635859436 ) ) ;
#10452 = CARTESIAN_POINT ( 'NONE',  ( 118.2987481442453088, -7.894159318335828068, -9.358103419637847864 ) ) ;
#10453 = B_SPLINE_CURVE_WITH_KNOTS ( 'NONE', 3,
 ( #3673, #31708, #27863, #24217, #41773, #28533, #34451, #21458 ),
 .UNSPECIFIED., .F., .F.,
 ( 4, 2, 2, 4 ),
 ( 0.000000000000000000, 0.5000000000000000000, 0.7500000000000000000, 1.000000000000000000 ),
 .UNSPECIFIED. ) ;
#10454 = SURFACE_STYLE_FILL_AREA ( #28448 ) ;
#10455 = CARTESIAN_POINT ( 'NONE',  ( 120.8514481442452961, -7.893985811506177619, -18.51759400769804742 ) ) ;
#10456 = CARTESIAN_POINT ( 'NONE',  ( 119.2631014775786298, 0.2603800115204892296, -16.42320221600525088 ) ) ;
#10457 = CARTESIAN_POINT ( 'NONE',  ( 108.8156921295247912, -9.868328341294093420, -13.39321520033831447 ) ) ;
#10458 = ADVANCED_FACE ( 'NONE', ( #12579 ), #26249, .T. ) ;
#10459 = CARTESIAN_POINT ( 'NONE',  ( 126.2404814775786264, -9.261995988541697145, -16.69588392320189030 ) ) ;
#10460 = DIRECTION ( 'NONE',  ( 3.317300593186674996E-33, -1.668003342285379964E-16, -1.000000000000000000 ) ) ;
#10461 = ORIENTED_EDGE ( 'NONE', *, *, #6916, .F. ) ;
#10462 =( BOUNDED_CURVE ( )  B_SPLINE_CURVE ( 2, ( #29224, #43131, #32408, #32184, #722, #21930, #11901, #8476, #11006, #38800, #7571, #18065, #31956, #14644, #19408, #40163, #2523 ),
 .UNSPECIFIED., .F., .F. ) 
 B_SPLINE_CURVE_WITH_KNOTS ( ( 3, 2, 2, 2, 2, 2, 2, 2, 3 ),
 ( 0.4546282416568590001, 0.4609375000000000000, 0.4687500000000000000, 0.4765625000000000000, 0.4843750000000000000, 0.4921875000000000000, 0.5000000000000000000, 0.5078125000000000000, 0.5141217583431409999 ),
 .UNSPECIFIED. ) 
 CURVE ( )  GEOMETRIC_REPRESENTATION_ITEM ( )  RATIONAL_B_SPLINE_CURVE ( ( 0.9763430640195960297, 0.9385262470928690259, 1.000000000000000000, 0.9238795325112869605, 1.000000000000000000, 0.9238795325112869605, 1.000000000000000000, 0.9238795325112869605, 1.000000000000000000, 0.9238795325112869605, 1.000000000000000000, 0.9238795325112869605, 1.000000000000000000, 0.9238795325112869605, 1.000000000000000000, 0.9385262470928680267, 0.9763430640195970289 ) ) 
 REPRESENTATION_ITEM ( '' )  );
#10463 = CARTESIAN_POINT ( 'NONE',  ( 116.2565881442452991, -9.261995988541697145, -16.69588392320189030 ) ) ;
#10464 = AXIS2_PLACEMENT_3D ( 'NONE', #30007, #19523, #16333 ) ;
#10465 = CARTESIAN_POINT ( 'NONE',  ( 120.3685329359119862, -4.283928203966213211, -7.183505701512925334 ) ) ;
#10466 = CARTESIAN_POINT ( 'NONE',  ( 117.0507614775786465, -10.30919188438810075, -12.61870101168855918 ) ) ;
#10467 = ORIENTED_EDGE ( 'NONE', *, *, #9273, .F. ) ;
#10468 = CARTESIAN_POINT ( 'NONE',  ( 116.2471765045247594, -7.250697342233347165, -19.15521520033831138 ) ) ;
#10469 = VECTOR ( 'NONE', #6177, 1000.000000000000227 ) ;
#10470 = LINE ( 'NONE', #10909, #8545 ) ;
#10471 = CARTESIAN_POINT ( 'NONE',  ( 119.8355804873411756, -2.348512537728041583, -17.99195118506215962 ) ) ;
#10472 = CARTESIAN_POINT ( 'NONE',  ( 125.0949563211859754, -6.092355046118379747, -18.43914408017989004 ) ) ;
#10473 = CYLINDRICAL_SURFACE ( 'NONE', #27348, 1.199999999999998623 ) ;
#10474 = CARTESIAN_POINT ( 'NONE',  ( 118.3554748109119998, -9.565557343593413364, -10.61323700422348004 ) ) ;
#10475 = DIRECTION ( 'NONE',  ( -0.9908103287288504424, 0.1352586133457950313, 0.000000000000000000 ) ) ;
#10476 = CARTESIAN_POINT ( 'NONE',  ( 117.7314814775786260, -5.574606645277164318, -18.38911715685844683 ) ) ;
#10477 = VECTOR ( 'NONE', #14003, 1000.000000000000000 ) ;
#10478 = CARTESIAN_POINT ( 'NONE',  ( 120.9842687714537988, -6.306599966548167124, -18.84486539759072699 ) ) ;
#10479 = CARTESIAN_POINT ( 'NONE',  ( 120.1140014775786398, -7.894159318335828068, -9.358103419637847864 ) ) ;
#10480 = CARTESIAN_POINT ( 'NONE',  ( 111.7751814775786556, -7.893985811506177619, -18.51759400769804742 ) ) ;
#10481 = CARTESIAN_POINT ( 'NONE',  ( 116.3133148109119759, -7.893985811506177619, -18.51759400769804742 ) ) ;
#10482 = CARTESIAN_POINT ( 'NONE',  ( 117.5613014775786525, -10.15424416112533912, -14.75197769757731336 ) ) ;
#10483 = EDGE_LOOP ( 'NONE', ( #9518, #2009, #24364, #6352, #3416 ) ) ;
#10484 = CARTESIAN_POINT ( 'NONE',  ( 116.1998614775786507, -10.63000616557722466, -14.87417383870573495 ) ) ;
#10485 = CARTESIAN_POINT ( 'NONE',  ( 115.8999108795247821, -1.325403438956436419, -16.93181055722141792 ) ) ;
#10486 = CARTESIAN_POINT ( 'NONE',  ( 88.07785292173620917, -25.99489077589524300, -13.39321520033831625 ) ) ;
#10487 = DIRECTION ( 'NONE',  ( 1.000000000000000000, 0.000000000000000000, 0.000000000000000000 ) ) ;
#10488 = DIRECTION ( 'NONE',  ( -0.000000000000000000, -0.9284778069183721172, -0.3713878862591650232 ) ) ;
#10489 = CARTESIAN_POINT ( 'NONE',  ( 122.6667014775786413, -7.893985811506177619, -18.51759400769804742 ) ) ;
#10490 = ORIENTED_EDGE ( 'NONE', *, *, #32531, .F. ) ;
#10491 = CARTESIAN_POINT ( 'NONE',  ( 127.9806007748782406, -9.485509010566754995, -9.755774181203904050 ) ) ;
#10492 = CARTESIAN_POINT ( 'NONE',  ( 119.0361948109119652, -2.084020599724406786, -8.691656652584148546 ) ) ;
#10493 = CARTESIAN_POINT ( 'NONE',  ( 116.0296814775786345, -8.166667518702805495, -8.995218007635852331 ) ) ;
#10494 = CARTESIAN_POINT ( 'NONE',  ( 124.3117748109119844, 0.1319031606808835910, -14.10382304977624734 ) ) ;
#10495 = CARTESIAN_POINT ( 'NONE',  ( 122.2128881442453263, -1.834011780172310813, -8.268836392978581529 ) ) ;
#10496 = AXIS2_PLACEMENT_3D ( 'NONE', #23079, #23769, #13049 ) ;
#10497 = CARTESIAN_POINT ( 'NONE',  ( 112.8439733795247832, -1.325403438956436419, -9.854619843455211026 ) ) ;
#10498 = CARTESIAN_POINT ( 'NONE',  ( 89.27917506468355668, -9.947819920281929740, -13.57505156349929720 ) ) ;
#10499 = VERTEX_POINT ( 'NONE', #2069 ) ;
#10500 = CARTESIAN_POINT ( 'NONE',  ( 113.3068014775786594, -8.166667518702817929, -8.995218007635859436 ) ) ;
#10501 = CARTESIAN_POINT ( 'NONE',  ( 112.0588148109119828, 0.5811942927096154232, -14.16772938898807155 ) ) ;
#10502 = CARTESIAN_POINT ( 'NONE',  ( 121.7590748109119687, -7.893985811506177619, -18.51759400769804742 ) ) ;
#10503 = CARTESIAN_POINT ( 'NONE',  ( 117.2776681442452968, -4.153390946401321671, -8.397313243818183892 ) ) ;
#10504 = DIRECTION ( 'NONE',  ( 0.000000000000000000, -0.3818493186865927203, 0.9242245927363029745 ) ) ;
#10505 = CARTESIAN_POINT ( 'NONE',  ( 119.0361948109119652, -7.893985811506177619, -18.51759400769804742 ) ) ;
#10506 = CARTESIAN_POINT ( 'NONE',  ( 95.62170725701116680, -25.21382792434065934, -13.93499303194756678 ) ) ;
#10507 = CARTESIAN_POINT ( 'NONE',  ( 121.7023481442452777, -0.8288870151387760510, -10.36305467784173118 ) ) ;
#10508 = ORIENTED_EDGE ( 'NONE', *, *, #6734, .T. ) ;
#10509 = CARTESIAN_POINT ( 'NONE',  ( 116.5955426422556940, -9.864956876375439165, -13.35547112582854190 ) ) ;
#10510 = CARTESIAN_POINT ( 'NONE',  ( 116.6536748109119941, 0.9020085738987339008, -11.91225656197089222 ) ) ;
#10511 = CARTESIAN_POINT ( 'NONE',  ( 123.7445081442452874, -7.894159318335828068, -9.358103419637847864 ) ) ;
#10512 = ORIENTED_EDGE ( 'NONE', *, *, #12568, .T. ) ;
#10513 = CARTESIAN_POINT ( 'NONE',  ( 124.0495485609119584, -10.36940331770106916, -15.09355782777062061 ) ) ;
#10514 = CARTESIAN_POINT ( 'NONE',  ( 62.35708470706295969, -12.50172482834998178, -9.937585253968853394 ) ) ;
#10515 = CARTESIAN_POINT ( 'NONE',  ( 122.0427081442452817, 0.5811942927096110934, -14.16772938898807510 ) ) ;
#10516 = CARTESIAN_POINT ( 'NONE',  ( 107.3571765045248299, -7.250697342233347165, -19.15521520033831138 ) ) ;
#10517 = CARTESIAN_POINT ( 'NONE',  ( 118.1852948109119836, -4.153390946401325223, -8.397313243818185668 ) ) ;
#10518 = ADVANCED_FACE ( 'NONE', ( #26484 ), #31622, .T. ) ;
#10519 = ORIENTED_EDGE ( 'NONE', *, *, #12380, .T. ) ;
#10520 = VERTEX_POINT ( 'NONE', #28174 ) ;
#10521 = CARTESIAN_POINT ( 'NONE',  ( 114.6682414775786469, -1.561330072975668060, -17.79121239304076596 ) ) ;
#10522 = CARTESIAN_POINT ( 'NONE',  ( 124.0281414775786146, -7.643976991954077427, -18.09477374809248928 ) ) ;
#10523 =( LENGTH_UNIT ( ) NAMED_UNIT ( * ) SI_UNIT ( .MILLI., .METRE. ) );
#10524 = CARTESIAN_POINT ( 'NONE',  ( 75.95778847736514194, -3.256761025687008537, -10.39321520033831625 ) ) ;
#10525 = ADVANCED_FACE ( 'NONE', ( #35884 ), #39324, .T. ) ;
#10526 = CARTESIAN_POINT ( 'NONE',  ( 122.9503348109119827, 0.5811942927096110934, -14.16772938898807510 ) ) ;
#10527 = DIRECTION ( 'NONE',  ( 0.8949343913984423304, 0.1703803081152067689, -0.4123869368673877545 ) ) ;
#10528 = CARTESIAN_POINT ( 'NONE',  ( 111.2184548109119788, -8.862178061932382889, -16.39564131203247399 ) ) ;
#10529 = CARTESIAN_POINT ( 'NONE',  ( 124.2550481442452792, -9.988377603198980381, -10.36322818467138518 ) ) ;
#10531 = CARTESIAN_POINT ( 'NONE',  ( 122.0994348109119443, -10.15424416112533912, -14.75197769757731336 ) ) ;
#10530 = CARTESIAN_POINT ( 'NONE',  ( 117.3343948109119737, -3.383040157471821630, -19.15922257007629170 ) ) ;
#10532 = CARTESIAN_POINT ( 'NONE',  ( 121.5888948109119809, 0.1319031606808879209, -14.10382304977623669 ) ) ;
#10533 = CARTESIAN_POINT ( 'NONE',  ( 125.2655881442453278, 0.08617673920530924403, -14.09731900820076334 ) ) ;
#10534 = CARTESIAN_POINT ( 'NONE',  ( 115.8027748109119841, -0.4660016031367893996, -10.09054647747474043 ) ) ;
#10535 = ORIENTED_EDGE ( 'NONE', *, *, #1621, .F. ) ;
#10536 = CARTESIAN_POINT ( 'NONE',  ( 109.8574890045247940, 0.8980012041604421569, -15.77991374673208469 ) ) ;
#10537 = CARTESIAN_POINT ( 'NONE',  ( 107.0793640045248196, 0.1403307496149616695, -15.46607636864997204 ) ) ;
#10538 = CARTESIAN_POINT ( 'NONE',  ( 109.1629577545248395, -7.250697342233347165, -7.631215200338321125 ) ) ;
#10539 = LINE ( 'NONE', #10986, #13148 ) ;
#10540 = CARTESIAN_POINT ( 'NONE',  ( 111.8319081442453182, -5.638512984488999180, -18.83840828888717311 ) ) ;
#10541 =( BOUNDED_SURFACE ( )  B_SPLINE_SURFACE ( 1, 2, ( 
 ( #24023, #44544, #19917, #6689, #33802, #20600, #9892, #2574, #34476, #20152, #5760, #37692, #2805, #16731, #30628, #29949, #27215, #23802, #20374, #34261, #3255, #3036, #16957, #30852, #28110, #34906, #42462, #11227, #7339, #34694, #41579, #27885, #28325, #42237, #31733, #24241, #13756, #31069, #38135, #44997, #282, #27665, #24675, #21708, #18062, #6906, #20816, #3482, #17837, #31953, #3696, #21033, #41800, #10338, #7568, #10558, #7123, #35136, #21257, #35595, #11002, #718, #24455, #7799, #17617, #17398, #24902, #14640, #31509, #38795, #35366, #17180, #38562, #4141, #14192, #25134, #503, #21481, #42014, #28557, #39028, #31286, #60, #13973, #38346, #10779, #3918, #14415, #22822, #35819, #18736, #32629, #39709, #28779, #951, #19183, #43355, #12124, #33062, #1836, #18285, #8473, #15765, #18514, #29666, #1395, #39483, #43579, #15310, #39254, #25799, #32845, #32181, #26026, #43128, #22375, #11897, #26247, #8921, #1175, #11671, #11454, #29219, #36272, #1613, #8247, #4815, #22597, #14869, #36047, #42686, #5040, #22154, #40160, #25360, #39932, #8019, #21926, #18954, #15534, #29439, #8692, #36498, #4591, #25580, #5267, #15090, #12349, #4365, #32405, #29001, #42909, #34200, #40613, #2974, #36939, #5484, #16446, #10064, #43811, #16903, #12577, #12802, #40845, #2292, #23516, #13026, #29894, #36714, #30795, #44719, #9371, #13479, #5710, #19404, #30346, #33291, #26481, #27382, #16671, #6173, #40386, #2066, #15990, #9147, #23053, #19861, #19627, #44269, #41304, #37635, #33511, #16220, #30124, #37403, #6408, #23280, #37162, #44038, #26702, #27155, #5939, #33749, #9600, #20094, #2519, #30567, #20316, #26924, #33979, #2747, #44486, #13253, #41077, #9834, #23744, #42181, #42405, #221, #10941, #7069, #31899, #24623, #14359, #27826, #28272, #443, #24844, #28498, #665, #38736, #7506, #38291, #14134, #23966, #10279, #20980, #34853, #28050, #3200, #20540, #21421, #17780, #31673, #35305, #4077, #37852, #41958, #18001, #38076, #14581, #3639, #13915, #6626, #17557, #13700, #10723 ),
 ( #34419, #24184, #17124, #31013, #35077, #44943, #10501, #27608, #41522, #6854, #20761, #17343, #34640, #3426, #38506, #31233, #5, #41737, #24402, #3858, #31452, #7283, #21199, #21645, #18897, #4306, #14810, #22542, #39194, #21871, #1339, #8417, #7960, #8192, #11841, #32572, #22100, #39877, #42629, #1784, #29387, #22323, #29612, #42853, #25073, #38966, #28723, #7735, #4536, #35534, #8642, #25748, #891, #25971, #1116, #36440, #36219, #18460, #5207, #4759, #18228, #32788, #15034, #32122, #11393, #11168, #11612, #25302, #35765, #1559, #19127, #33009, #32350, #43300, #35988, #28945, #15709, #25523, #15253, #39426, #18681, #29159, #4984, #43072, #39654, #15483, #12069, #29839, #41026, #30514, #34151, #2465, #12977, #37347, #44435, #23694, #5884, #20265, #20038, #23229, #12522, #26872, #19353, #37110, #22996, #13203, #9321, #33920, #26647, #6120, #27103, #9779, #37580, #40330, #40562, #36887, #40788, #36662, #16851, #12746, #9095, #2691, #26423, #5657, #6353, #19576, #33241, #16621, #9546, #33455, #16389, #2920, #2235, #43527, #12296, #2014, #19805, #33694, #30289, #16166, #26195, #43757, #40102, #8862, #44216, #30070, #22764, #23461, #5435, #15939, #43982, #3154, #38241, #7231, #41908, #27556, #34805, #21147, #13650, #14307, #394, #34371, #45104, #41688, #10450, #38027, #38460, #17074, #35253, #24575, #24353, #44890, #42132, #14085, #28226, #38685, #23918, #30967, #7020, #37799, #41469, #10892, #10227, #24135, #20931, #28002, #6803, #27776, #31400, #3591, #17501, #24791, #20712, #21370, #3803, #10672, #4030, #17294, #44667, #13429, #34591, #27333, #3374, #41251, #7450, #168, #20492, #30743, #31186, #10009, #35021, #13862, #6574, #17729, #31626, #38911, #28444, #31850, #620, #17951, #25018, #14530, #42356, #11117, #7682, #21596, #35483, #33969, #26692, #33501, #41067, #9824, #5929, #33282, #40148, #26470, #26915, #20306, #33738, #23041, #26238, #2057, #13244, #2737, #6399, #19851, #30334, #9591, #16662, #23734, #23271, #37625, #37392, #40603, #29883, #44260, #36705 ) ),
 .UNSPECIFIED., .F., .F., .T. ) 
 B_SPLINE_SURFACE_WITH_KNOTS ( ( 2, 2 ),
 ( 3, 2, 2, 2, 2, 2, 2, 2, 2, 2, 2, 2, 2, 2, 2, 2, 2, 2, 2, 2, 2, 2, 2, 2, 2, 2, 2, 2, 2, 2, 2, 2, 2, 2, 2, 2, 2, 2, 2, 2, 2, 2, 2, 2, 2, 2, 2, 2, 2, 2, 2, 2, 2, 2, 2, 2, 2, 2, 2, 2, 2, 2, 2, 2, 2, 2, 2, 2, 2, 2, 2, 2, 2, 2, 2, 2, 2, 2, 2, 2, 2, 2, 2, 2, 2, 2, 2, 2, 2, 2, 2, 2, 2, 2, 2, 2, 2, 2, 2, 2, 2, 2, 2, 2, 2, 2, 2, 2, 2, 2, 2, 2, 2, 2, 2, 2, 2, 2, 2, 2, 2, 2, 2, 2, 2, 2, 2, 2, 3 ),
 ( 0.000000000000000000, 1.000000000000000000 ),
 ( 0.000000000000000000, 0.007812500000000000000, 0.01562500000000000000, 0.02343750000000000000, 0.03125000000000000000, 0.03906250000000000000, 0.04687500000000000000, 0.05468750000000000000, 0.06250000000000000000, 0.07031250000000000000, 0.07812500000000000000, 0.08593750000000000000, 0.09375000000000000000, 0.1015625000000000000, 0.1093750000000000000, 0.1171875000000000000, 0.1250000000000000000, 0.1328125000000000000, 0.1406250000000000000, 0.1484375000000000000, 0.1562500000000000000, 0.1640625000000000000, 0.1718750000000000000, 0.1796875000000000000, 0.1875000000000000000, 0.1953125000000000000, 0.2031250000000000000, 0.2109375000000000000, 0.2187500000000000000, 0.2265625000000000000, 0.2343750000000000000, 0.2421875000000000000, 0.2500000000000000000, 0.2578125000000000000, 0.2656250000000000000, 0.2734375000000000000, 0.2812500000000000000, 0.2890625000000000000, 0.2968750000000000000, 0.3046875000000000000, 0.3125000000000000000, 0.3203125000000000000, 0.3281250000000000000, 0.3359375000000000000, 0.3437500000000000000, 0.3515625000000000000, 0.3593750000000000000, 0.3671875000000000000, 0.3750000000000000000, 0.3828125000000000000, 0.3906250000000000000, 0.3984375000000000000, 0.4062500000000000000, 0.4140625000000000000, 0.4218750000000000000, 0.4296875000000000000, 0.4375000000000000000, 0.4453125000000000000, 0.4531250000000000000, 0.4609375000000000000, 0.4687500000000000000, 0.4765625000000000000, 0.4843750000000000000, 0.4921875000000000000, 0.5000000000000000000, 0.5078125000000000000, 0.5156250000000000000, 0.5234375000000000000, 0.5312500000000000000, 0.5390625000000000000, 0.5468750000000000000, 0.5546875000000000000, 0.5625000000000000000, 0.5703125000000000000, 0.5781250000000000000, 0.5859375000000000000, 0.5937500000000000000, 0.6015625000000000000, 0.6093750000000000000, 0.6171875000000000000, 0.6250000000000000000, 0.6328125000000000000, 0.6406250000000000000, 0.6484375000000000000, 0.6562500000000000000, 0.6640625000000000000, 0.6718750000000000000, 0.6796875000000000000, 0.6875000000000000000, 0.6953125000000000000, 0.7031250000000000000, 0.7109375000000000000, 0.7187500000000000000, 0.7265625000000000000, 0.7343750000000000000, 0.7421875000000000000, 0.7500000000000000000, 0.7578125000000000000, 0.7656250000000000000, 0.7734375000000000000, 0.7812500000000000000, 0.7890625000000000000, 0.7968750000000000000, 0.8046875000000000000, 0.8125000000000000000, 0.8203125000000000000, 0.8281250000000000000, 0.8359375000000000000, 0.8437500000000000000, 0.8515625000000000000, 0.8593750000000000000, 0.8671875000000000000, 0.8750000000000000000, 0.8828125000000000000, 0.8906250000000000000, 0.8984375000000000000, 0.9062500000000000000, 0.9140625000000000000, 0.9218750000000000000, 0.9296875000000000000, 0.9375000000000000000, 0.9453125000000000000, 0.9531250000000000000, 0.9609375000000000000, 0.9687500000000000000, 0.9765625000000000000, 0.9843750000000000000, 0.9921875000000000000, 1.000000000000000000 ),
 .UNSPECIFIED. ) 
 GEOMETRIC_REPRESENTATION_ITEM ( )  RATIONAL_B_SPLINE_SURFACE ( (
 ( 1.000000000000000000, 0.9238795325112869605, 1.000000000000000000, 0.9238795325112869605, 1.000000000000000000, 0.9238795325112869605, 1.000000000000000000, 0.9238795325112869605, 1.000000000000000000, 0.9238795325112869605, 1.000000000000000000, 0.9238795325112869605, 1.000000000000000000, 0.9238795325112869605, 1.000000000000000000, 0.9238795325112869605, 1.000000000000000000, 0.9238795325112869605, 1.000000000000000000, 0.9238795325112869605, 1.000000000000000000, 0.9238795325112869605, 1.000000000000000000, 0.9238795325112869605, 1.000000000000000000, 0.9238795325112869605, 1.000000000000000000, 0.9238795325112869605, 1.000000000000000000, 0.9238795325112869605, 1.000000000000000000, 0.9238795325112869605, 1.000000000000000000, 0.9238795325112869605, 1.000000000000000000, 0.9238795325112869605, 1.000000000000000000, 0.9238795325112869605, 1.000000000000000000, 0.9238795325112869605, 1.000000000000000000, 0.9238795325112869605, 1.000000000000000000, 0.9238795325112869605, 1.000000000000000000, 0.9238795325112869605, 1.000000000000000000, 0.9238795325112869605, 1.000000000000000000, 0.9238795325112869605, 1.000000000000000000, 0.9238795325112869605, 1.000000000000000000, 0.9238795325112869605, 1.000000000000000000, 0.9238795325112869605, 1.000000000000000000, 0.9238795325112869605, 1.000000000000000000, 0.9238795325112869605, 1.000000000000000000, 0.9238795325112869605, 1.000000000000000000, 0.9238795325112869605, 1.000000000000000000, 0.9238795325112869605, 1.000000000000000000, 0.9238795325112869605, 1.000000000000000000, 0.9238795325112869605, 1.000000000000000000, 0.9238795325112869605, 1.000000000000000000, 0.9238795325112869605, 1.000000000000000000, 0.9238795325112869605, 1.000000000000000000, 0.9238795325112869605, 1.000000000000000000, 0.9238795325112869605, 1.000000000000000000, 0.9238795325112869605, 1.000000000000000000, 0.9238795325112869605, 1.000000000000000000, 0.9238795325112869605, 1.000000000000000000, 0.9238795325112869605, 1.000000000000000000, 0.9238795325112869605, 1.000000000000000000, 0.9238795325112869605, 1.000000000000000000, 0.9238795325112869605, 1.000000000000000000, 0.9238795325112869605, 1.000000000000000000, 0.9238795325112869605, 1.000000000000000000, 0.9238795325112869605, 1.000000000000000000, 0.9238795325112869605, 1.000000000000000000, 0.9238795325112869605, 1.000000000000000000, 0.9238795325112869605, 1.000000000000000000, 0.9238795325112869605, 1.000000000000000000, 0.9238795325112869605, 1.000000000000000000, 0.9238795325112869605, 1.000000000000000000, 0.9238795325112869605, 1.000000000000000000, 0.9238795325112869605, 1.000000000000000000, 0.9238795325112869605, 1.000000000000000000, 0.9238795325112869605, 1.000000000000000000, 0.9238795325112869605, 1.000000000000000000, 0.9238795325112869605, 1.000000000000000000, 0.9238795325112869605, 1.000000000000000000, 0.9238795325112869605, 1.000000000000000000, 0.9238795325112869605, 1.000000000000000000, 0.9238795325112869605, 1.000000000000000000, 0.9238795325112869605, 1.000000000000000000, 0.9238795325112869605, 1.000000000000000000, 0.9238795325112869605, 1.000000000000000000, 0.9238795325112869605, 1.000000000000000000, 0.9238795325112869605, 1.000000000000000000, 0.9238795325112869605, 1.000000000000000000, 0.9238795325112869605, 1.000000000000000000, 0.9238795325112869605, 1.000000000000000000, 0.9238795325112869605, 1.000000000000000000, 0.9238795325112869605, 1.000000000000000000, 0.9238795325112869605, 1.000000000000000000, 0.9238795325112869605, 1.000000000000000000, 0.9238795325112869605, 1.000000000000000000, 0.9238795325112869605, 1.000000000000000000, 0.9238795325112869605, 1.000000000000000000, 0.9238795325112869605, 1.000000000000000000, 0.9238795325112869605, 1.000000000000000000, 0.9238795325112869605, 1.000000000000000000, 0.9238795325112869605, 1.000000000000000000, 0.9238795325112869605, 1.000000000000000000, 0.9238795325112869605, 1.000000000000000000, 0.9238795325112869605, 1.000000000000000000, 0.9238795325112869605, 1.000000000000000000, 0.9238795325112869605, 1.000000000000000000, 0.9238795325112869605, 1.000000000000000000, 0.9238795325112869605, 1.000000000000000000, 0.9238795325112869605, 1.000000000000000000, 0.9238795325112869605, 1.000000000000000000, 0.9238795325112869605, 1.000000000000000000, 0.9238795325112869605, 1.000000000000000000, 0.9238795325112869605, 1.000000000000000000, 0.9238795325112869605, 1.000000000000000000, 0.9238795325112869605, 1.000000000000000000, 0.9238795325112869605, 1.000000000000000000, 0.9238795325112869605, 1.000000000000000000, 0.9238795325112869605, 1.000000000000000000, 0.9238795325112869605, 1.000000000000000000, 0.9238795325112869605, 1.000000000000000000, 0.9238795325112869605, 1.000000000000000000, 0.9238795325112869605, 1.000000000000000000, 0.9238795325112869605, 1.000000000000000000, 0.9238795325112869605, 1.000000000000000000, 0.9238795325112869605, 1.000000000000000000, 0.9238795325112869605, 1.000000000000000000, 0.9238795325112869605, 1.000000000000000000, 0.9238795325112869605, 1.000000000000000000, 0.9238795325112869605, 1.000000000000000000, 0.9238795325112869605, 1.000000000000000000, 0.9238795325112869605, 1.000000000000000000, 0.9238795325112869605, 1.000000000000000000, 0.9238795325112869605, 1.000000000000000000, 0.9238795325112869605, 1.000000000000000000, 0.9238795325112869605, 1.000000000000000000, 0.9238795325112869605, 1.000000000000000000, 0.9238795325112869605, 1.000000000000000000, 0.9238795325112869605, 1.000000000000000000, 0.9238795325112869605, 1.000000000000000000, 0.9238795325112869605, 1.000000000000000000, 0.9238795325112869605, 1.000000000000000000, 0.9238795325112869605, 1.000000000000000000, 0.9238795325112869605, 1.000000000000000000, 0.9238795325112869605, 1.000000000000000000),
 ( 1.000000000000000000, 0.9238795325112869605, 1.000000000000000000, 0.9238795325112869605, 1.000000000000000000, 0.9238795325112869605, 1.000000000000000000, 0.9238795325112869605, 1.000000000000000000, 0.9238795325112869605, 1.000000000000000000, 0.9238795325112869605, 1.000000000000000000, 0.9238795325112869605, 1.000000000000000000, 0.9238795325112869605, 1.000000000000000000, 0.9238795325112869605, 1.000000000000000000, 0.9238795325112869605, 1.000000000000000000, 0.9238795325112869605, 1.000000000000000000, 0.9238795325112869605, 1.000000000000000000, 0.9238795325112869605, 1.000000000000000000, 0.9238795325112869605, 1.000000000000000000, 0.9238795325112869605, 1.000000000000000000, 0.9238795325112869605, 1.000000000000000000, 0.9238795325112869605, 1.000000000000000000, 0.9238795325112869605, 1.000000000000000000, 0.9238795325112869605, 1.000000000000000000, 0.9238795325112869605, 1.000000000000000000, 0.9238795325112869605, 1.000000000000000000, 0.9238795325112869605, 1.000000000000000000, 0.9238795325112869605, 1.000000000000000000, 0.9238795325112869605, 1.000000000000000000, 0.9238795325112869605, 1.000000000000000000, 0.9238795325112869605, 1.000000000000000000, 0.9238795325112869605, 1.000000000000000000, 0.9238795325112869605, 1.000000000000000000, 0.9238795325112869605, 1.000000000000000000, 0.9238795325112869605, 1.000000000000000000, 0.9238795325112869605, 1.000000000000000000, 0.9238795325112869605, 1.000000000000000000, 0.9238795325112869605, 1.000000000000000000, 0.9238795325112869605, 1.000000000000000000, 0.9238795325112869605, 1.000000000000000000, 0.9238795325112869605, 1.000000000000000000, 0.9238795325112869605, 1.000000000000000000, 0.9238795325112869605, 1.000000000000000000, 0.9238795325112869605, 1.000000000000000000, 0.9238795325112869605, 1.000000000000000000, 0.9238795325112869605, 1.000000000000000000, 0.9238795325112869605, 1.000000000000000000, 0.9238795325112869605, 1.000000000000000000, 0.9238795325112869605, 1.000000000000000000, 0.9238795325112869605, 1.000000000000000000, 0.9238795325112869605, 1.000000000000000000, 0.9238795325112869605, 1.000000000000000000, 0.9238795325112869605, 1.000000000000000000, 0.9238795325112869605, 1.000000000000000000, 0.9238795325112869605, 1.000000000000000000, 0.9238795325112869605, 1.000000000000000000, 0.9238795325112869605, 1.000000000000000000, 0.9238795325112869605, 1.000000000000000000, 0.9238795325112869605, 1.000000000000000000, 0.9238795325112869605, 1.000000000000000000, 0.9238795325112869605, 1.000000000000000000, 0.9238795325112869605, 1.000000000000000000, 0.9238795325112869605, 1.000000000000000000, 0.9238795325112869605, 1.000000000000000000, 0.9238795325112869605, 1.000000000000000000, 0.9238795325112869605, 1.000000000000000000, 0.9238795325112869605, 1.000000000000000000, 0.9238795325112869605, 1.000000000000000000, 0.9238795325112869605, 1.000000000000000000, 0.9238795325112869605, 1.000000000000000000, 0.9238795325112869605, 1.000000000000000000, 0.9238795325112869605, 1.000000000000000000, 0.9238795325112869605, 1.000000000000000000, 0.9238795325112869605, 1.000000000000000000, 0.9238795325112869605, 1.000000000000000000, 0.9238795325112869605, 1.000000000000000000, 0.9238795325112869605, 1.000000000000000000, 0.9238795325112869605, 1.000000000000000000, 0.9238795325112869605, 1.000000000000000000, 0.9238795325112869605, 1.000000000000000000, 0.9238795325112869605, 1.000000000000000000, 0.9238795325112869605, 1.000000000000000000, 0.9238795325112869605, 1.000000000000000000, 0.9238795325112869605, 1.000000000000000000, 0.9238795325112869605, 1.000000000000000000, 0.9238795325112869605, 1.000000000000000000, 0.9238795325112869605, 1.000000000000000000, 0.9238795325112869605, 1.000000000000000000, 0.9238795325112869605, 1.000000000000000000, 0.9238795325112869605, 1.000000000000000000, 0.9238795325112869605, 1.000000000000000000, 0.9238795325112869605, 1.000000000000000000, 0.9238795325112869605, 1.000000000000000000, 0.9238795325112869605, 1.000000000000000000, 0.9238795325112869605, 1.000000000000000000, 0.9238795325112869605, 1.000000000000000000, 0.9238795325112869605, 1.000000000000000000, 0.9238795325112869605, 1.000000000000000000, 0.9238795325112869605, 1.000000000000000000, 0.9238795325112869605, 1.000000000000000000, 0.9238795325112869605, 1.000000000000000000, 0.9238795325112869605, 1.000000000000000000, 0.9238795325112869605, 1.000000000000000000, 0.9238795325112869605, 1.000000000000000000, 0.9238795325112869605, 1.000000000000000000, 0.9238795325112869605, 1.000000000000000000, 0.9238795325112869605, 1.000000000000000000, 0.9238795325112869605, 1.000000000000000000, 0.9238795325112869605, 1.000000000000000000, 0.9238795325112869605, 1.000000000000000000, 0.9238795325112869605, 1.000000000000000000, 0.9238795325112869605, 1.000000000000000000, 0.9238795325112869605, 1.000000000000000000, 0.9238795325112869605, 1.000000000000000000, 0.9238795325112869605, 1.000000000000000000, 0.9238795325112869605, 1.000000000000000000, 0.9238795325112869605, 1.000000000000000000, 0.9238795325112869605, 1.000000000000000000, 0.9238795325112869605, 1.000000000000000000, 0.9238795325112869605, 1.000000000000000000, 0.9238795325112869605, 1.000000000000000000, 0.9238795325112869605, 1.000000000000000000, 0.9238795325112869605, 1.000000000000000000, 0.9238795325112869605, 1.000000000000000000, 0.9238795325112869605, 1.000000000000000000, 0.9238795325112869605, 1.000000000000000000, 0.9238795325112869605, 1.000000000000000000, 0.9238795325112869605, 1.000000000000000000, 0.9238795325112869605, 1.000000000000000000, 0.9238795325112869605, 1.000000000000000000, 0.9238795325112869605, 1.000000000000000000, 0.9238795325112869605, 1.000000000000000000, 0.9238795325112869605, 1.000000000000000000) ) ) 
 REPRESENTATION_ITEM ( '' )  SURFACE ( )  );
#10542 = ORIENTED_EDGE ( 'NONE', *, *, #2301, .T. ) ;
#10543 = EDGE_CURVE ( 'NONE', #20305, #24500, #7983, .T. ) ;
#10544 = CARTESIAN_POINT ( 'NONE',  ( 124.1415948109119540, -6.344957434206665248, -7.627207830600338134 ) ) ;
#10545 = CARTESIAN_POINT ( 'NONE',  ( 110.7603796295247918, -4.863998795839590272, -19.15521520033831493 ) ) ;
#10546 = CARTESIAN_POINT ( 'NONE',  ( 61.69189222814998175, -39.81387020377190566, -6.644606968976401795 ) ) ;
#10547 = CARTESIAN_POINT ( 'NONE',  ( 123.2339681442453241, -6.344957434206665248, -7.627207830600338134 ) ) ;
#10548 = ADVANCED_FACE ( 'NONE', ( #10842 ), #37823, .T. ) ;
#10549 = EDGE_CURVE ( 'NONE', #11473, #37481, #18125, .T. ) ;
#10550 = FACE_BOUND ( 'NONE', #15336, .T. ) ;
#10551 = CARTESIAN_POINT ( 'NONE',  ( 119.7434548109119703, -2.527210466738041728, -8.967976844669124148 ) ) ;
#10552 = CARTESIAN_POINT ( 'NONE',  ( 112.6828081442453282, -7.893985811506177619, -18.51759400769804742 ) ) ;
#10553 = CARTESIAN_POINT ( 'NONE',  ( 116.1082702545247827, -10.62599879583958717, -15.77991374673208469 ) ) ;
#10554 = CARTESIAN_POINT ( 'NONE',  ( 106.0375671295248310, -10.62599879583958540, -13.39321520033831447 ) ) ;
#10555 = CONICAL_SURFACE ( 'NONE', #40394, 2.999999999999999556, 0.9599310885968830309 ) ;
#10556 = ORIENTED_EDGE ( 'NONE', *, *, #2559, .T. ) ;
#10557 = DIRECTION ( 'NONE',  ( -1.000000000000000000, 0.000000000000000000, 0.000000000000000000 ) ) ;
#10558 = CARTESIAN_POINT ( 'NONE',  ( 115.2922348109119781, 0.4262465694468514643, -12.03445270309931736 ) ) ;
#10559 = CARTESIAN_POINT ( 'NONE',  ( 126.0135748109119902, -1.833838273342660141, -17.42832698103878286 ) ) ;
#10560 = CARTESIAN_POINT ( 'NONE',  ( 114.0246765045248196, -7.250697342233347165, -19.15521520033831138 ) ) ;
#10561 = CARTESIAN_POINT ( 'NONE',  ( 107.9822546295247889, -4.863998795839590272, -18.39754474579285315 ) ) ;
#10562 = CARTESIAN_POINT ( 'NONE',  ( 119.9438214775786378, -2.084020599724406786, -8.691656652584148546 ) ) ;
#10563 = PRODUCT_DEFINITION_CONTEXT ( 'detailed design', #9054, 'design' ) ;
#10564 = CARTESIAN_POINT ( 'NONE',  ( 118.7525614775786380, -1.833838273342659253, -17.42832698103878286 ) ) ;
#10565 = CARTESIAN_POINT ( 'NONE',  ( 112.6260814775786514, -0.8288870151387760510, -10.36305467784173118 ) ) ;
#10566 = ORIENTED_EDGE ( 'NONE', *, *, #13240, .F. ) ;
#10567 = AXIS2_PLACEMENT_3D ( 'NONE', #26792, #5796, #2144 ) ;
#10568 = CARTESIAN_POINT ( 'NONE',  ( 124.0848681442452772, -5.574606645277164318, -18.38911715685844683 ) ) ;
#10569 = PLANE ( 'NONE',  #7681 ) ;
#10570 = CARTESIAN_POINT ( 'NONE',  ( 112.8529881442453160, -7.894159318335828068, -9.358103419637847864 ) ) ;
#10571 = ORIENTED_EDGE ( 'NONE', *, *, #20585, .T. ) ;
#10572 = CYLINDRICAL_SURFACE ( 'NONE', #15773, 6.000000000000005329 ) ;
#10573 = CARTESIAN_POINT ( 'NONE',  ( 110.0658483795247804, -8.402594152722688392, -16.93181055722141792 ) ) ;
#10574 = EDGE_CURVE ( 'NONE', #14508, #4821, #21544, .T. ) ;
#10575 = ORIENTED_EDGE ( 'NONE', *, *, #4937, .T. ) ;
#10576 = CARTESIAN_POINT ( 'NONE',  ( 118.3554748109119998, -9.565557343593413364, -10.61323700422348004 ) ) ;
#10577 = CARTESIAN_POINT ( 'NONE',  ( 112.0020881442453344, -9.565557343593413364, -10.61323700422348004 ) ) ;
#10578 = CARTESIAN_POINT ( 'NONE',  ( 70.89841814381148311, -68.89136543047671069, -37.69090763720760151 ) ) ;
#10579 = CARTESIAN_POINT ( 'NONE',  ( 121.4103298109119748, -7.200787124940443817, -17.81845355600750835 ) ) ;
#10580 = ORIENTED_EDGE ( 'NONE', *, *, #16967, .F. ) ;
#10581 = CARTESIAN_POINT ( 'NONE',  ( 112.1533811237171534, -8.920124835228172344, -16.36603124229645090 ) ) ;
#10582 = CARTESIAN_POINT ( 'NONE',  ( 119.7434548109119703, -2.564829167770875884, -8.950426663462648591 ) ) ;
#10583 = EDGE_CURVE ( 'NONE', #37160, #42815, #18176, .T. ) ;
#10584 = AXIS2_PLACEMENT_3D ( 'NONE', #2541, #13724, #34664 ) ;
#10585 = CARTESIAN_POINT ( 'NONE',  ( 106.8710046295248759, -4.863998795839590272, -18.39754474579285315 ) ) ;
#10586 = CARTESIAN_POINT ( 'NONE',  ( 112.7395348109119766, -5.638512984488999180, -18.83840828888717311 ) ) ;
#10587 = CARTESIAN_POINT ( 'NONE',  ( 121.5321681442453183, -0.1624402480850797581, -16.17319339645315424 ) ) ;
#10588 = CARTESIAN_POINT ( 'NONE',  ( 119.2063748109119814, -7.894159318335828068, -9.358103419637847864 ) ) ;
#10589 = CARTESIAN_POINT ( 'NONE',  ( 125.1630841924336295, -7.152576104508079347, -20.44691296307176387 ) ) ;
#10590 = ORIENTED_EDGE ( 'NONE', *, *, #23388, .F. ) ;
#10591 = CARTESIAN_POINT ( 'NONE',  ( 116.7121013948518140, -7.018196182899982816, -18.03571476200153967 ) ) ;
#10592 = CARTESIAN_POINT ( 'NONE',  ( 117.3911214775786505, -7.894159318335828068, -9.358103419637847864 ) ) ;
#10593 = CARTESIAN_POINT ( 'NONE',  ( 125.5030348109119558, -6.222761293078241884, -8.102969835052219238 ) ) ;
#10594 = CARTESIAN_POINT ( 'NONE',  ( 125.1573330740870489, -1.286148409757067679, -16.90866798357478729 ) ) ;
#10595 = DIRECTION ( 'NONE',  ( 0.000000000000000000, -0.3818493186865927203, 0.9242245927363029745 ) ) ;
#10596 = CARTESIAN_POINT ( 'NONE',  ( 114.7816948109119863, 0.5811942927096154232, -14.16772938898807155 ) ) ;
#10597 = ORIENTED_EDGE ( 'NONE', *, *, #35586, .F. ) ;
#10598 = CARTESIAN_POINT ( 'NONE',  ( 113.9875214775786532, -0.4660016031367893996, -10.09054647747474043 ) ) ;
#10599 = LINE ( 'NONE', #21522, #26902 ) ;
#10600 = CARTESIAN_POINT ( 'NONE',  ( 110.2742077545248094, -7.250697342233347165, -7.631215200338321125 ) ) ;
#10601 = CARTESIAN_POINT ( 'NONE',  ( 114.0442481442453300, -1.834011780172310813, -8.268836392978581529 ) ) ;
#10602 = ADVANCED_FACE ( 'NONE', ( #32245 ), #17643, .T. ) ;
#10603 = CARTESIAN_POINT ( 'NONE',  ( 114.6115148109119986, -3.383040157471821630, -19.15922257007629170 ) ) ;
#10604 = CARTESIAN_POINT ( 'NONE',  ( 123.1205148109119563, -7.643976991954077427, -18.09477374809248928 ) ) ;
#10605 = FACE_OUTER_BOUND ( 'NONE', #21746, .T. ) ;
#10606 = CARTESIAN_POINT ( 'NONE',  ( 108.0517077545248696, -2.791137627527939813, -18.39754474579286025 ) ) ;
#10607 = CARTESIAN_POINT ( 'NONE',  ( 117.2209414775786485, -7.893985811506194494, -18.51759400769804031 ) ) ;
#10608 = CARTESIAN_POINT ( 'NONE',  ( 109.2294667191664530, -5.158692816978520668, -18.58770334803330115 ) ) ;
#10609 = CARTESIAN_POINT ( 'NONE',  ( 118.3554748109119998, -9.565557343593413364, -10.61323700422348004 ) ) ;
#10610 = CARTESIAN_POINT ( 'NONE',  ( 71.31713442278437753, 2.423123680056944007, -19.39321520033831447 ) ) ;
#10611 = CARTESIAN_POINT ( 'NONE',  ( 116.3860827545247787, -6.936859964151250502, -8.388885654883777576 ) ) ;
#10612 = CARTESIAN_POINT ( 'NONE',  ( 110.0658483795247804, -0.7896495226426338832, -9.318865927141430916 ) ) ;
#10613 = CYLINDRICAL_SURFACE ( 'NONE', #20376, 1.999999999999998890 ) ;
#10614 = CARTESIAN_POINT ( 'NONE',  ( 125.5030348109119558, -3.383040157471821630, -19.15922257007629170 ) ) ;
#10615 = FACE_OUTER_BOUND ( 'NONE', #33302, .T. ) ;
#10616 = ADVANCED_FACE ( 'NONE', ( #16251 ), #24710, .T. ) ;
#10617 = CARTESIAN_POINT ( 'NONE',  ( 121.8158014775786171, -5.638512984488999180, -18.83840828888717311 ) ) ;
#10618 = CARTESIAN_POINT ( 'NONE',  ( 115.4624148109119943, -5.638512984488999180, -18.83840828888717311 ) ) ;
#10619 = EDGE_LOOP ( 'NONE', ( #10326, #44174, #6008, #24994 ) ) ;
#10620 = AXIS2_PLACEMENT_3D ( 'NONE', #31366, #32035, #14052 ) ;
#10621 = CARTESIAN_POINT ( 'NONE',  ( 116.3133148109120043, -2.084020599724406786, -8.691656652584148546 ) ) ;
#10622 = CARTESIAN_POINT ( 'NONE',  ( 123.2906948109119867, -8.166667518702819706, -8.995218007635861213 ) ) ;
#10623 = CARTESIAN_POINT ( 'NONE',  ( 117.6180281442453150, -0.4660016031367893996, -10.09054647747474043 ) ) ;
#10624 = CARTESIAN_POINT ( 'NONE',  ( 114.4980614775786734, -2.084020599724406786, -8.691656652584148546 ) ) ;
#10625 = EDGE_LOOP ( 'NONE', ( #22534, #22242, #7634, #25651 ) ) ;
#10626 = CARTESIAN_POINT ( 'NONE',  ( 121.4754414775786131, -1.833838273342659697, -17.42832698103878286 ) ) ;
#10627 = CARTESIAN_POINT ( 'NONE',  ( 117.2209414775786485, -7.893985811506177619, -18.51759400769804742 ) ) ;
#10628 = CARTESIAN_POINT ( 'NONE',  ( 137.5120057812997629, 0.07598602772913314041, -14.15343988704196043 ) ) ;
#10629 = CARTESIAN_POINT ( 'NONE',  ( 112.4967077545247633, -7.250697342233347165, -7.631215200338321125 ) ) ;
#10630 = CARTESIAN_POINT ( 'NONE',  ( 64.66985656418735573, -0.6761475757289143740, -10.04201475645285591 ) ) ;
#10631 = CARTESIAN_POINT ( 'NONE',  ( 90.99708770779186295, -27.84333996136784961, -14.15691383771150136 ) ) ;
#10632 = CARTESIAN_POINT ( 'NONE',  ( 78.69189222814998175, -41.90950876995110974, -19.14091845747265808 ) ) ;
#10633 = CARTESIAN_POINT ( 'NONE',  ( 113.4202548109119846, -10.30919188438810075, -12.61870101168855918 ) ) ;
#10634 = AXIS2_PLACEMENT_3D ( 'NONE', #14023, #24071, #37739 ) ;
#10635 = CARTESIAN_POINT ( 'NONE',  ( 136.5847729262740415, -10.54478413941382620, -13.96952502453041944 ) ) ;
#10636 = CARTESIAN_POINT ( 'NONE',  ( 113.1933481442453058, -5.574606645277164318, -18.38911715685844683 ) ) ;
#10637 = CARTESIAN_POINT ( 'NONE',  ( 61.49539530949622446, -12.46540452739392890, -17.12947030793335657 ) ) ;
#10638 = ADVANCED_FACE ( 'NONE', ( #24001 ), #26736, .F. ) ;
#10639 = CARTESIAN_POINT ( 'NONE',  ( 122.8560864091100768, -0.9924539043446216624, -17.29976612834909133 ) ) ;
#10640 = CARTESIAN_POINT ( 'NONE',  ( 116.1082702545247827, 0.1403307496149616695, -11.32035403202665336 ) ) ;
#10641 = CARTESIAN_POINT ( 'NONE',  ( 118.0151148109119816, -10.63000616557722466, -14.87417383870573495 ) ) ;
#10642 = LINE ( 'NONE', #19497, #12210 ) ;
#10643 = DIRECTION ( 'NONE',  ( -0.9063289528979890930, -0.4225728684367167087, -3.263703555153020391E-15 ) ) ;
#10644 = CARTESIAN_POINT ( 'NONE',  ( 124.5059548109119731, -4.863998795839242995, -13.39321520033831447 ) ) ;
#10645 = CARTESIAN_POINT ( 'NONE',  ( 123.1205148109119563, -7.643976991954077427, -18.09477374809248928 ) ) ;
#10646 = CARTESIAN_POINT ( 'NONE',  ( 120.9649014775786355, -6.222761293078241884, -8.102969835052219238 ) ) ;
#10647 = ORIENTED_EDGE ( 'NONE', *, *, #39550, .T. ) ;
#10648 = CARTESIAN_POINT ( 'NONE',  ( 74.64594387179452895, -42.43939829949535181, -7.393215200338315363 ) ) ;
#10649 = CARTESIAN_POINT ( 'NONE',  ( 121.7023481442452777, -9.261995988541697145, -16.69588392320189030 ) ) ;
#10650 = CARTESIAN_POINT ( 'NONE',  ( 115.4831921295247952, -9.868328341294093420, -13.39321520033831447 ) ) ;
#10651 = CARTESIAN_POINT ( 'NONE',  ( 116.6536748109119941, -10.15424416112533912, -14.75197769757731336 ) ) ;
#10652 = CARTESIAN_POINT ( 'NONE',  ( 114.3846081442453197, 0.4262465694468514643, -12.03445270309931736 ) ) ;
#10653 = CARTESIAN_POINT ( 'NONE',  ( 106.6626452545248611, -9.868328341294098749, -15.46607636864997204 ) ) ;
#10654 = CARTESIAN_POINT ( 'NONE',  ( 111.8716296295247901, -4.863998795839590272, -19.15521520033831493 ) ) ;
#10655 = CARTESIAN_POINT ( 'NONE',  ( 119.8870948109119752, -0.8288870151387760510, -10.36305467784173118 ) ) ;
#10656 = CARTESIAN_POINT ( 'NONE',  ( 122.0427081442452817, -9.859900752359378018, -12.68260735090039759 ) ) ;
#10657 = ADVANCED_FACE ( 'NONE', ( #9399 ), #25475, .T. ) ;
#10658 = AXIS2_PLACEMENT_3D ( 'NONE', #7290, #39203, #28507 ) ;
#10659 = CYLINDRICAL_SURFACE ( 'NONE', #12897, 5.999999999999997335 ) ;
#10660 = CARTESIAN_POINT ( 'NONE',  ( 109.2294540793403712, -5.090843144855284663, -7.811289275559451184 ) ) ;
#10661 = CARTESIAN_POINT ( 'NONE',  ( 120.7157985609119635, -10.36940331770106916, -15.09355782777062061 ) ) ;
#10662 = CARTESIAN_POINT ( 'NONE',  ( 111.0381921295247878, -9.868328341294093420, -13.39321520033831447 ) ) ;
#10663 = EDGE_CURVE ( 'NONE', #9021, #34939, #45132, .T. ) ;
#10664 = PRODUCT ( 'Main Bracket', 'Main Bracket', '', ( #32741 ) ) ;
#10665 = DIRECTION ( 'NONE',  ( 0.9609149988134837450, -0.1028163501681639419, 0.2570431154366518145 ) ) ;
#10666 = CARTESIAN_POINT ( 'NONE',  ( 112.2289948109119848, -1.834011780172310813, -8.268836392978581529 ) ) ;
#10667 = CARTESIAN_POINT ( 'NONE',  ( 115.2355081442453155, -10.30919188438810075, -12.61870101168855918 ) ) ;
#10668 = CARTESIAN_POINT ( 'NONE',  ( 112.3578015045248861, -2.477300249445798297, -7.631215200338321125 ) ) ;
#10669 = CARTESIAN_POINT ( 'NONE',  ( 138.2184548109119930, -10.44474571748257041, -15.59668151425567650 ) ) ;
#10670 = ORIENTED_EDGE ( 'NONE', *, *, #27590, .T. ) ;
#10671 = DIRECTION ( 'NONE',  ( 0.000000000000000000, -0.3818493186865936084, 0.9242245927363024194 ) ) ;
#10672 = CARTESIAN_POINT ( 'NONE',  ( 122.7801548109119665, -3.383040157471821630, -19.15922257007629170 ) ) ;
#10673 = CARTESIAN_POINT ( 'NONE',  ( 114.6115148109119986, -3.383040157471821630, -19.15922257007629170 ) ) ;
#10674 = CARTESIAN_POINT ( 'NONE',  ( 123.2339681442453241, -3.505236298600246325, -18.68346056562440793 ) ) ;
#10675 = VECTOR ( 'NONE', #18338, 1000.000000000000114 ) ;
#10676 = CARTESIAN_POINT ( 'NONE',  ( 124.0848681442452772, -4.089484607189486809, -7.948022111789456723 ) ) ;
#10677 = CARTESIAN_POINT ( 'NONE',  ( 118.6391081442452986, -4.089484607189486809, -7.948022111789456723 ) ) ;
#10678 = CIRCLE ( 'NONE', #36133, 1.499999999999999556 ) ;
#10679 = CARTESIAN_POINT ( 'NONE',  ( 107.8433483795247838, -8.402594152722688392, -16.93181055722141792 ) ) ;
#10680 = CARTESIAN_POINT ( 'NONE',  ( 113.8740681442453138, -9.859900752359374465, -12.68260735090039404 ) ) ;
#10681 = CARTESIAN_POINT ( 'NONE',  ( 85.31664890835789095, -21.99489077589589314, -11.39321520033831447 ) ) ;
#10682 = ORIENTED_EDGE ( 'NONE', *, *, #34847, .T. ) ;
#10683 = CARTESIAN_POINT ( 'NONE',  ( 121.1350814775786233, 0.5811942927096110934, -14.16772938898807510 ) ) ;
#10684 = AXIS2_PLACEMENT_3D ( 'NONE', #44910, #5903, #6372 ) ;
#10685 = DIRECTION ( 'NONE',  ( 0.1352586133457950590, 0.9908103287288504424, 0.000000000000000000 ) ) ;
#10686 = CARTESIAN_POINT ( 'NONE',  ( 116.1431348109119881, -10.30919188438810075, -12.61870101168855918 ) ) ;
#10687 = VERTEX_POINT ( 'NONE', #30828 ) ;
#10688 = CARTESIAN_POINT ( 'NONE',  ( 106.9404577545248145, -2.791137627527939813, -18.39754474579286025 ) ) ;
#10689 = CARTESIAN_POINT ( 'NONE',  ( 125.0492214775786266, -6.344957434206665248, -7.627207830600338134 ) ) ;
#10690 = DIRECTION ( 'NONE',  ( -0.9609149988134837450, 0.1028163501681639419, -0.2570431154366518145 ) ) ;
#10691 = CARTESIAN_POINT ( 'NONE',  ( 115.3489614775786407, -0.8288870151387760510, -10.36305467784173118 ) ) ;
#10692 = FACE_OUTER_BOUND ( 'NONE', #15949, .T. ) ;
#10693 = CARTESIAN_POINT ( 'NONE',  ( 120.9649014775786355, -6.222761293078241884, -8.102969835052219238 ) ) ;
#10694 = CARTESIAN_POINT ( 'NONE',  ( 111.2184548109119788, -8.862178061932382889, -16.39564131203247399 ) ) ;
#10695 = CARTESIAN_POINT ( 'NONE',  ( 120.2841814775786276, -10.15424416112533912, -14.75197769757731336 ) ) ;
#10696 = FACE_OUTER_BOUND ( 'NONE', #32936, .T. ) ;
#10697 = AXIS2_PLACEMENT_3D ( 'NONE', #30566, #44268, #10278 ) ;
#10698 = CARTESIAN_POINT ( 'NONE',  ( 119.2631014775786298, -9.565557343593413364, -10.61323700422348004 ) ) ;
#10699 = CARTESIAN_POINT ( 'NONE',  ( 111.8886348109120092, -3.383040157471821630, -19.15922257007629170 ) ) ;
#10700 = CARTESIAN_POINT ( 'NONE',  ( 117.1074881442453233, -10.63000616557722466, -14.87417383870573495 ) ) ;
#10701 = CARTESIAN_POINT ( 'NONE',  ( 123.4608748109119745, -10.63000616557723355, -14.87417383870568344 ) ) ;
#10702 = CARTESIAN_POINT ( 'NONE',  ( 121.8158014775786171, -4.153390946401325223, -8.397313243818185668 ) ) ;
#10703 = ORIENTED_EDGE ( 'NONE', *, *, #34780, .F. ) ;
#10704 = CARTESIAN_POINT ( 'NONE',  ( 117.9583881442453048, -10.30919188438810075, -12.61870101168855918 ) ) ;
#10705 = CARTESIAN_POINT ( 'NONE',  ( 109.0240515045248202, -2.477300249445798297, -7.631215200338321125 ) ) ;
#10706 = AXIS2_PLACEMENT_3D ( 'NONE', #2623, #10165, #16784 ) ;
#10707 = CARTESIAN_POINT ( 'NONE',  ( 73.07463722459043254, -53.64660018989884804, -33.76695433548739089 ) ) ;
#10708 = CYLINDRICAL_SURFACE ( 'NONE', #37828, 1.999999999999998890 ) ;
#10709 = EDGE_CURVE ( 'NONE', #32359, #23226, #35634, .T. ) ;
#10710 = CARTESIAN_POINT ( 'NONE',  ( 91.65862616933031859, -25.99489077589524300, -13.39321520033831447 ) ) ;
#10711 = CARTESIAN_POINT ( 'NONE',  ( 123.8012348109119642, 0.2603800115204892296, -16.42320221600525088 ) ) ;
#10712 = ORIENTED_EDGE ( 'NONE', *, *, #15239, .T. ) ;
#10713 = CARTESIAN_POINT ( 'NONE',  ( 126.4536383592459146, -8.380280027055789560, -9.674679031694752851 ) ) ;
#10714 = CARTESIAN_POINT ( 'NONE',  ( 119.3765548109119834, -10.15424416112533912, -14.75197769757731336 ) ) ;
#10715 = DIRECTION ( 'NONE',  ( 0.000000000000000000, 0.000000000000000000, 1.000000000000000000 ) ) ;
#10716 = CARTESIAN_POINT ( 'NONE',  ( 64.51289607492564926, -15.37840541894191126, -15.84259706628786724 ) ) ;
#10717 = AXIS2_PLACEMENT_3D ( 'NONE', #11583, #40296, #22290 ) ;
#10718 = DIRECTION ( 'NONE',  ( 0.5040994586965589219, 0.8636456077245089347, 0.000000000000000000 ) ) ;
#10719 = CARTESIAN_POINT ( 'NONE',  ( 111.3854577545248645, -2.791137627527939813, -18.39754474579286025 ) ) ;
#10720 = DIRECTION ( 'NONE',  ( -0.5735764363510446051, 0.3127926500124816878, -0.7570804645221042017 ) ) ;
#10721 = ORIENTED_EDGE ( 'NONE', *, *, #15840, .F. ) ;
#10722 = CARTESIAN_POINT ( 'NONE',  ( 113.5337081442453240, -9.261995988541697145, -16.69588392320189030 ) ) ;
#10723 = CARTESIAN_POINT ( 'NONE',  ( 126.6942948109119840, -8.899110576539710493, -16.42337572283490132 ) ) ;
#10724 = CARTESIAN_POINT ( 'NONE',  ( 124.7088614775786226, 0.2603800115204892296, -16.42320221600525088 ) ) ;
#10725 = CARTESIAN_POINT ( 'NONE',  ( 115.5191414775786569, -6.222761293078241884, -8.102969835052219238 ) ) ;
#10726 = DIRECTION ( 'NONE',  ( 0.8636456077245086016, -0.5040994586965593660, 0.000000000000000000 ) ) ;
#10727 = DIRECTION ( 'NONE',  ( 1.000000000000000000, 0.000000000000000000, 0.000000000000000000 ) ) ;
#10728 = CARTESIAN_POINT ( 'NONE',  ( 118.6958348109119754, -6.344957434206665248, -7.627207830600338134 ) ) ;
#10729 = DIRECTION ( 'NONE',  ( 0.1352586133457950590, 0.9908103287288504424, 0.000000000000000000 ) ) ;
#10730 =( BOUNDED_SURFACE ( )  B_SPLINE_SURFACE ( 1, 2, ( 
 ( #20578, #21014, #10760, #37892, #31714, #3677, #38328, #6670, #37672, #483, #24437, #28307, #20356, #34457, #24223, #3236, #14171 ),
 ( #41997, #24657, #38543, #3014, #17162, #13514, #27423, #6887, #44979, #7318, #13737, #27646, #20796, #21463, #25342, #8230, #25783 ) ),
 .UNSPECIFIED., .F., .F., .T. ) 
 B_SPLINE_SURFACE_WITH_KNOTS ( ( 2, 2 ),
 ( 3, 2, 2, 2, 2, 2, 2, 2, 3 ),
 ( 0.000000000000000000, 1.000000000000000000 ),
 ( 0.000000000000000000, 0.1250000000000000000, 0.2500000000000000000, 0.3750000000000000000, 0.5000000000000000000, 0.6250000000000000000, 0.7500000000000000000, 0.8750000000000000000, 1.000000000000000000 ),
 .UNSPECIFIED. ) 
 GEOMETRIC_REPRESENTATION_ITEM ( )  RATIONAL_B_SPLINE_SURFACE ( (
 ( 1.000000000000000000, 0.9238795325112869605, 1.000000000000000000, 0.9238795325112869605, 1.000000000000000000, 0.9238795325112869605, 1.000000000000000000, 0.9238795325112869605, 1.000000000000000000, 0.9238795325112869605, 1.000000000000000000, 0.9238795325112869605, 1.000000000000000000, 0.9238795325112869605, 1.000000000000000000, 0.9238795325112869605, 1.000000000000000000),
 ( 1.000000000000000000, 0.9238795325112869605, 1.000000000000000000, 0.9238795325112869605, 1.000000000000000000, 0.9238795325112869605, 1.000000000000000000, 0.9238795325112869605, 1.000000000000000000, 0.9238795325112869605, 1.000000000000000000, 0.9238795325112869605, 1.000000000000000000, 0.9238795325112869605, 1.000000000000000000, 0.9238795325112869605, 1.000000000000000000) ) ) 
 REPRESENTATION_ITEM ( '' )  SURFACE ( )  );
#10731 = DIRECTION ( 'NONE',  ( 0.000000000000000000, 0.000000000000000000, -1.000000000000000000 ) ) ;
#10732 = CARTESIAN_POINT ( 'NONE',  ( 62.77916120947350720, -64.70587450232225990, -45.96270195078128751 ) ) ;
#10733 = CARTESIAN_POINT ( 'NONE',  ( 122.7234281442452755, -4.153390946401325223, -8.397313243818185668 ) ) ;
#10734 = VERTEX_POINT ( 'NONE', #31931 ) ;
#10735 = CARTESIAN_POINT ( 'NONE',  ( 107.2294421295247844, -9.051693226400931991, -21.89321520033831447 ) ) ;
#10736 = CARTESIAN_POINT ( 'NONE',  ( 117.5045748109119756, 0.5811942927096110934, -14.16772938898807510 ) ) ;
#10737 = CARTESIAN_POINT ( 'NONE',  ( 124.0281414775786146, -7.643976991954077427, -18.09477374809248928 ) ) ;
#10738 = ORIENTED_EDGE ( 'NONE', *, *, #42307, .F. ) ;
#10739 = CARTESIAN_POINT ( 'NONE',  ( 121.3096769858783404, -2.378957183258601393, -17.95140958770220152 ) ) ;
#10740 = CARTESIAN_POINT ( 'NONE',  ( 124.1415948109119540, -6.344957434206665248, -7.627207830600338134 ) ) ;
#10741 = CARTESIAN_POINT ( 'NONE',  ( 105.9681140045248355, -10.62599879583958717, -11.00651665394454604 ) ) ;
#10742 = CARTESIAN_POINT ( 'NONE',  ( 118.9794681442453026, -0.8288870151387760510, -10.36305467784173118 ) ) ;
#10743 = ORIENTED_EDGE ( 'NONE', *, *, #3535, .T. ) ;
#10744 = ORIENTED_EDGE ( 'NONE', *, *, #24000, .T. ) ;
#10745 = CARTESIAN_POINT ( 'NONE',  ( 113.5904348109119866, -7.893985811506177619, -18.51759400769804742 ) ) ;
#10746 = CARTESIAN_POINT ( 'NONE',  ( 124.8223148109119762, -10.15424416112533912, -14.75197769757731336 ) ) ;
#10747 = CARTESIAN_POINT ( 'NONE',  ( 120.6245414775786458, -9.988377603198960841, -10.36322818467135853 ) ) ;
#10748 = AXIS2_PLACEMENT_3D ( 'NONE', #13795, #31110, #44815 ) ;
#10749 = CARTESIAN_POINT ( 'NONE',  ( 109.2294421295247844, -11.83367149576868727, -19.39321520033831447 ) ) ;
#10750 = CARTESIAN_POINT ( 'NONE',  ( 125.6732148109119862, 0.5811942927096110934, -14.16772938898807510 ) ) ;
#10751 = LINE ( 'NONE', #34231, #42983 ) ;
#10752 = PLANE ( 'NONE',  #26653 ) ;
#10753 = CARTESIAN_POINT ( 'NONE',  ( 122.4397948109119767, -9.988377603198976828, -10.36322818467138340 ) ) ;
#10755 = CARTESIAN_POINT ( 'NONE',  ( 123.9146881442452894, -10.15424416112533912, -14.75197769757731336 ) ) ;
#10754 = CARTESIAN_POINT ( 'NONE',  ( 121.7023481442452777, -9.261995988541697145, -16.69588392320189030 ) ) ;
#10756 = CARTESIAN_POINT ( 'NONE',  ( 121.7590748109119687, -2.084020599724406786, -8.691656652584148546 ) ) ;
#10757 = CARTESIAN_POINT ( 'NONE',  ( 125.8328548109119964, -8.862178061931794915, -16.39564131203325559 ) ) ;
#10758 = CARTESIAN_POINT ( 'NONE',  ( 114.4980614775786592, -7.893985811506177619, -18.51759400769804742 ) ) ;
#10759 = VERTEX_POINT ( 'NONE', #3894 ) ;
#10760 = CARTESIAN_POINT ( 'NONE',  ( 125.0386814775786490, -5.568102603701690967, -18.34339073538286513 ) ) ;
#10761 = CARTESIAN_POINT ( 'NONE',  ( 105.4819421295248247, 0.8980012041604618078, -13.39321520033831447 ) ) ;
#10762 = CARTESIAN_POINT ( 'NONE',  ( 110.6214733795247867, -1.325403438956436419, -9.854619843455211026 ) ) ;
#10763 = CARTESIAN_POINT ( 'NONE',  ( 114.3024890045248156, -9.868328341294098749, -11.32035403202665869 ) ) ;
#10764 = AXIS2_PLACEMENT_3D ( 'NONE', #8729, #21967, #15128 ) ;
#10765 = DIRECTION ( 'NONE',  ( 0.000000000000000000, -0.3818493186865927203, 0.9242245927363029745 ) ) ;
#10766 = CARTESIAN_POINT ( 'NONE',  ( 126.3539348109119800, -4.153390946401325223, -8.397313243818185668 ) ) ;
#10767 = VERTEX_POINT ( 'NONE', #14166 ) ;
#10768 = CARTESIAN_POINT ( 'NONE',  ( 112.6828081442453282, -2.084020599724406786, -8.691656652584148546 ) ) ;
#10769 = CARTESIAN_POINT ( 'NONE',  ( 111.9410827545248708, -2.477300249445798297, -19.15521520033831138 ) ) ;
#10770 = CARTESIAN_POINT ( 'NONE',  ( 76.36356431740252049, -0.2843300395004543235, -19.39321520033831447 ) ) ;
#10771 = CARTESIAN_POINT ( 'NONE',  ( 124.8790414775786246, -0.4660016031367893996, -10.09054647747474043 ) ) ;
#10772 = CARTESIAN_POINT ( 'NONE',  ( 124.4819548109119722, -7.893985811506177619, -18.51759400769804742 ) ) ;
#10773 = DIRECTION ( 'NONE',  ( -0.2768435750659253847, -0.3568721902840677473, 0.8921882507333133150 ) ) ;
#10774 = CARTESIAN_POINT ( 'NONE',  ( 113.0231681442453322, 0.9020085738987339008, -11.91225656197089222 ) ) ;
#10775 = CARTESIAN_POINT ( 'NONE',  ( 113.3301452545248083, 0.8980012041604421569, -11.00651665394454071 ) ) ;
#10776 = CARTESIAN_POINT ( 'NONE',  ( 114.5803015045248117, -6.936859964151250502, -18.39754474579286025 ) ) ;
#10777 = ORIENTED_EDGE ( 'NONE', *, *, #22060, .T. ) ;
#10778 = DIRECTION ( 'NONE',  ( 0.000000000000000000, -0.9242245927363028635, -0.3818493186865930533 ) ) ;
#10779 = CARTESIAN_POINT ( 'NONE',  ( 116.9940348109119839, -0.1624402480850797581, -16.17319339645315424 ) ) ;
#10780 = CARTESIAN_POINT ( 'NONE',  ( 111.7184548109119788, -9.261995988541697145, -16.69588392320189030 ) ) ;
#10781 = CARTESIAN_POINT ( 'NONE',  ( 114.9275671295247889, -10.62599879583958540, -13.39321520033831447 ) ) ;
#10782 = CARTESIAN_POINT ( 'NONE',  ( 106.4542858795248179, -8.402594152722688392, -9.854619843455216355 ) ) ;
#10783 = CARTESIAN_POINT ( 'NONE',  ( 122.2696148109119889, -5.574606645277164318, -18.38911715685844683 ) ) ;
#10784 = CARTESIAN_POINT ( 'NONE',  ( 118.5823814775786360, -7.643976991954077427, -18.09477374809248928 ) ) ;
#10785 = CARTESIAN_POINT ( 'NONE',  ( 111.8886348109120092, -6.222761293078241884, -8.102969835052219238 ) ) ;
#10786 = ORIENTED_EDGE ( 'NONE', *, *, #29187, .T. ) ;
#10787 = CARTESIAN_POINT ( 'NONE',  ( 125.6732148109119862, -9.859900752359378018, -12.68260735090039759 ) ) ;
#10788 = DIRECTION ( 'NONE',  ( 0.000000000000000000, 0.000000000000000000, -1.000000000000000000 ) ) ;
#10789 = CARTESIAN_POINT ( 'NONE',  ( 113.0798948109119948, -8.899110576539710493, -16.42337572283490132 ) ) ;
#10790 = ORIENTED_EDGE ( 'NONE', *, *, #10549, .T. ) ;
#10791 = CARTESIAN_POINT ( 'NONE',  ( 126.2202699136527286, -8.897422299132054846, -16.34980449512860545 ) ) ;
#10792 = CARTESIAN_POINT ( 'NONE',  ( 106.1764733795248219, -8.938348069036489818, -17.46756447353520159 ) ) ;
#10793 = CARTESIAN_POINT ( 'NONE',  ( 108.4684265045247997, -2.791137627527939813, -8.388885654883777576 ) ) ;
#10794 = EDGE_LOOP ( 'NONE', ( #21013, #1240, #9167, #3267 ) ) ;
#10795 = CARTESIAN_POINT ( 'NONE',  ( 119.3198281442452924, -9.859900752359374465, -12.68260735090039404 ) ) ;
#10796 = CIRCLE ( 'NONE', #5696, 2.999999999999999556 ) ;
#10797 = CARTESIAN_POINT ( 'NONE',  ( 114.4413348109119823, -0.8288870151387760510, -10.36305467784173118 ) ) ;
#10798 = CARTESIAN_POINT ( 'NONE',  ( 124.5592491210230435, -9.863888965223885918, -13.51979257824428871 ) ) ;
#10799 = EDGE_CURVE ( 'NONE', #16241, #38271, #32739, .T. ) ;
#10800 = DIRECTION ( 'NONE',  ( 1.000000000000000000, 0.000000000000000000, 0.000000000000000000 ) ) ;
#10801 = ORIENTED_EDGE ( 'NONE', *, *, #40662, .F. ) ;
#10802 = CARTESIAN_POINT ( 'NONE',  ( 67.37136766119182596, -67.53150897494617766, -41.09057840265009531 ) ) ;
#10803 = DIRECTION ( 'NONE',  ( 0.000000000000000000, 0.6161630946014892141, 0.7876185884367612466 ) ) ;
#10804 = CARTESIAN_POINT ( 'NONE',  ( 114.5803015045248117, -2.477300249445798297, -7.631215200338321125 ) ) ;
#10805 = SHAPE_REPRESENTATION ( 'Clamp Bolt', ( #12375 ), #32596 ) ;
#10806 = CARTESIAN_POINT ( 'NONE',  ( 114.3278814775786429, -10.30919188438810075, -12.61870101168855918 ) ) ;
#10807 = CARTESIAN_POINT ( 'NONE',  ( 121.5888948109119809, 0.1319031606808879209, -14.10382304977623669 ) ) ;
#10808 = CARTESIAN_POINT ( 'NONE',  ( 117.3911214775786505, -7.894159318335828068, -9.358103419637847864 ) ) ;
#10809 = DIRECTION ( 'NONE',  ( -1.000000000000000000, 0.000000000000000000, 0.000000000000000000 ) ) ;
#10810 = VERTEX_POINT ( 'NONE', #20574 ) ;
#10811 = CARTESIAN_POINT ( 'NONE',  ( 117.3343948109119737, -6.222761293078241884, -8.102969835052219238 ) ) ;
#10812 = CARTESIAN_POINT ( 'NONE',  ( 115.4831921295247952, 0.8980012041604618078, -13.39321520033831447 ) ) ;
#10813 = CARTESIAN_POINT ( 'NONE',  ( 125.1493398804576458, -1.281315077902259958, -16.91510428757999307 ) ) ;
#10814 = CYLINDRICAL_SURFACE ( 'NONE', #25438, 1.999999999999998890 ) ;
#10815 = CARTESIAN_POINT ( 'NONE',  ( 114.6115148109119986, -3.383040157471821630, -19.15922257007629170 ) ) ;
#10816 = ORIENTED_EDGE ( 'NONE', *, *, #1869, .F. ) ;
#10817 = CARTESIAN_POINT ( 'NONE',  ( 116.0864081442453113, -9.988377603198976828, -10.36322818467138340 ) ) ;
#10818 = LINE ( 'NONE', #27930, #15245 ) ;
#10819 = CARTESIAN_POINT ( 'NONE',  ( 109.7880358795247986, -0.7896495226426338832, -17.46756447353520159 ) ) ;
#10820 = CARTESIAN_POINT ( 'NONE',  ( 126.0135748109119902, -1.833838273342660141, -17.42832698103878286 ) ) ;
#10821 = CARTESIAN_POINT ( 'NONE',  ( 112.3991748109119868, -8.166667518702817929, -8.995218007635859436 ) ) ;
#10822 = CARTESIAN_POINT ( 'NONE',  ( 122.9503348109119827, -9.859900752359378018, -12.68260735090039759 ) ) ;
#10823 = CARTESIAN_POINT ( 'NONE',  ( 64.21381391892587942, -15.17632890891008479, -16.20372347372216026 ) ) ;
#10824 = CARTESIAN_POINT ( 'NONE',  ( 109.3018640045248304, 0.1403307496149616695, -15.46607636864997204 ) ) ;
#10825 = EDGE_CURVE ( 'NONE', #16862, #15722, #28084, .T. ) ;
#10826 = VERTEX_POINT ( 'NONE', #34885 ) ;
#10827 = CARTESIAN_POINT ( 'NONE',  ( 120.5102552477523830, -1.220279397241718966, -16.99638242193886484 ) ) ;
#10828 = CARTESIAN_POINT ( 'NONE',  ( 109.2296389617769989, -8.690306221987864177, -17.17721600569922558 ) ) ;
#10829 = CARTESIAN_POINT ( 'NONE',  ( 117.3343948109119737, -6.222761293078241884, -8.102969835052219238 ) ) ;
#10830 = CARTESIAN_POINT ( 'NONE',  ( 106.8710046295248759, -4.863998795839590272, -7.631215200338315796 ) ) ;
#10831 = CARTESIAN_POINT ( 'NONE',  ( 122.6603829525735421, -1.111561923218657322, -17.14115599315433158 ) ) ;
#10832 = CARTESIAN_POINT ( 'NONE',  ( 107.5655358795247736, -0.7896495226426338832, -17.46756447353520159 ) ) ;
#10833 = DIRECTION ( 'NONE',  ( 1.000000000000000000, 0.000000000000000000, -0.000000000000000000 ) ) ;
#10834 = CARTESIAN_POINT ( 'NONE',  ( 111.6050014775786536, 0.1319031606808879209, -14.10382304977623669 ) ) ;
#10835 = CARTESIAN_POINT ( 'NONE',  ( 120.1707281442453166, -9.565557343593393824, -10.61323700422344274 ) ) ;
#10836 = EDGE_CURVE ( 'NONE', #38525, #37456, #11632, .T. ) ;
#10837 = CARTESIAN_POINT ( 'NONE',  ( 123.4041481442452834, -10.30919188438810075, -12.61870101168855918 ) ) ;
#10838 = CARTESIAN_POINT ( 'NONE',  ( 116.0864081442453113, -9.988377603198976828, -10.36322818467138340 ) ) ;
#10839 = EDGE_LOOP ( 'NONE', ( #41284, #4388 ) ) ;
#10840 = EDGE_CURVE ( 'NONE', #19108, #33768, #3613, .T. ) ;
#10841 = CARTESIAN_POINT ( 'NONE',  ( 116.5969481442453031, -9.859900752359374465, -12.68260735090039404 ) ) ;
#10842 = FACE_OUTER_BOUND ( 'NONE', #3316, .T. ) ;
#10843 = CARTESIAN_POINT ( 'NONE',  ( 116.3700414775786527, -5.638512984488999180, -18.83840828888717311 ) ) ;
#10844 = CARTESIAN_POINT ( 'NONE',  ( 117.7314814775786260, -5.574606645277164318, -18.38911715685844683 ) ) ;
#10845 = ORIENTED_EDGE ( 'NONE', *, *, #32665, .T. ) ;
#10846 = CARTESIAN_POINT ( 'NONE',  ( 120.1707281442453166, -9.565557343593413364, -10.61323700422348004 ) ) ;
#10847 = EDGE_CURVE ( 'NONE', #39689, #15722, #11255, .T. ) ;
#10848 = CARTESIAN_POINT ( 'NONE',  ( 115.9162281442453235, -4.089484607189486809, -7.948022111789456723 ) ) ;
#10849 = CARTESIAN_POINT ( 'NONE',  ( 136.8358652995586340, 0.6885668881867501590, -12.92874118612615497 ) ) ;
#10850 = CARTESIAN_POINT ( 'NONE',  ( 110.1353015045248469, -2.477300249445798297, -7.631215200338321125 ) ) ;
#10851 = ADVANCED_FACE ( 'NONE', ( #17814 ), #34908, .F. ) ;
#10852 = EDGE_CURVE ( 'NONE', #24453, #20884, #20793, .T. ) ;
#10853 = EDGE_CURVE ( 'NONE', #40056, #37700, #10453, .T. ) ;
#10854 = CARTESIAN_POINT ( 'NONE',  ( 61.58853448128274266, 6.499901296646661386, -14.64321520033831447 ) ) ;
#10855 = CARTESIAN_POINT ( 'NONE',  ( 126.8198326591488723, 0.4339650712495903284, -13.22324850598036328 ) ) ;
#10856 = CARTESIAN_POINT ( 'NONE',  ( 116.8722546295247895, -4.863998795839590272, -18.39754474579285315 ) ) ;
#10857 = CARTESIAN_POINT ( 'NONE',  ( 115.4056881442453459, -7.893985811506177619, -18.51759400769804742 ) ) ;
#10858 = CIRCLE ( 'NONE', #42168, 0.5000000000000043299 ) ;
#10859 = CARTESIAN_POINT ( 'NONE',  ( 136.7741008876076023, -10.45032920902457363, -13.88867884707207345 ) ) ;
#10860 = CARTESIAN_POINT ( 'NONE',  ( 112.4559014775786778, -0.1624402480850797581, -16.17319339645315424 ) ) ;
#10861 = CARTESIAN_POINT ( 'NONE',  ( 111.2695311052981708, 0.4930828106259610433, -12.14321520033830026 ) ) ;
#10862 = DIRECTION ( 'NONE',  ( 0.000000000000000000, -0.4669533266896293000, -0.8842819633428516957 ) ) ;
#10863 = CARTESIAN_POINT ( 'NONE',  ( 113.4690515045247992, -6.936859964151250502, -18.39754474579286025 ) ) ;
#10864 = CARTESIAN_POINT ( 'NONE',  ( 112.7395348109119766, -4.153390946401321671, -8.397313243818183892 ) ) ;
#10865 = FILL_AREA_STYLE_COLOUR ( '', #42032 ) ;
#10866 = CARTESIAN_POINT ( 'NONE',  ( 70.19189222814998175, -67.83330054016514055, -40.33609291459782753 ) ) ;
#10868 = CARTESIAN_POINT ( 'NONE',  ( 114.8951481442453115, -0.4660016031367893996, -10.09054647747474043 ) ) ;
#10867 = DIRECTION ( 'NONE',  ( 0.000000000000000000, -0.9284778069183718952, -0.3713878862591650232 ) ) ;
#10869 = DIRECTION ( 'NONE',  ( 0.000000000000000000, -0.3818493186865927203, 0.9242245927363029745 ) ) ;
#10870 = CARTESIAN_POINT ( 'NONE',  ( 120.0572748109119772, -6.222761293078241884, -8.102969835052219238 ) ) ;
#10871 = ORIENTED_EDGE ( 'NONE', *, *, #20893, .F. ) ;
#10872 = CARTESIAN_POINT ( 'NONE',  ( 136.9394333025927040, -7.157115554028094628, -8.388523816445465187 ) ) ;
#10873 = CARTESIAN_POINT ( 'NONE',  ( 123.4608748109119745, -10.63000616557722466, -14.87417383870573495 ) ) ;
#10874 = CARTESIAN_POINT ( 'NONE',  ( 115.1359265045248605, -2.791137627527939813, -8.388885654883777576 ) ) ;
#10875 = CARTESIAN_POINT ( 'NONE',  ( 121.1350814775786233, -9.859900752359378018, -12.68260735090039759 ) ) ;
#10876 = CARTESIAN_POINT ( 'NONE',  ( 125.9568481442452850, -6.344957434206665248, -7.627207830600338134 ) ) ;
#10877 = CARTESIAN_POINT ( 'NONE',  ( 85.90559391046389237, -27.46290284877522936, -8.672333233500294725 ) ) ;
#10878 = CARTESIAN_POINT ( 'NONE',  ( 111.9410827545248708, -2.477300249445798297, -19.15521520033831138 ) ) ;
#10879 = CARTESIAN_POINT ( 'NONE',  ( 118.9227414775786542, 0.4262465694468514643, -12.03445270309931736 ) ) ;
#10880 = CARTESIAN_POINT ( 'NONE',  ( 118.9227414775786542, 0.4262465694468514643, -12.03445270309931736 ) ) ;
#10881 = FACE_OUTER_BOUND ( 'NONE', #32444, .T. ) ;
#10882 = CARTESIAN_POINT ( 'NONE',  ( 109.2294421509997591, -4.671552374252124551, -7.823865419768949891 ) ) ;
#10883 = CARTESIAN_POINT ( 'NONE',  ( 120.6463454359119822, -11.07370829466463569, -12.81314460846529002 ) ) ;
#10884 = CARTESIAN_POINT ( 'NONE',  ( 110.5520202545248054, 0.1403307496149616695, -11.32035403202665336 ) ) ;
#10885 = CARTESIAN_POINT ( 'NONE',  ( 116.8295036813193946, 1.973147266281264578, -20.94028373511954655 ) ) ;
#10886 = CARTESIAN_POINT ( 'NONE',  ( 118.2987481442453088, -1.561330072975668504, -17.79121239304076951 ) ) ;
#10887 = CARTESIAN_POINT ( 'NONE',  ( 116.1431348109119881, -10.30919188438810075, -12.61870101168855918 ) ) ;
#10888 = CARTESIAN_POINT ( 'NONE',  ( 110.2047546295247855, -4.863998795839590272, -7.631215200338315796 ) ) ;
#10889 = LINE ( 'NONE', #43017, #22823 ) ;
#10890 = ORIENTED_EDGE ( 'NONE', *, *, #29473, .T. ) ;
#10891 = CARTESIAN_POINT ( 'NONE',  ( 113.1706886996682186, -1.172797794773252189, -17.05961127468924943 ) ) ;
#10892 = CARTESIAN_POINT ( 'NONE',  ( 121.9859814775786333, 0.2603800115204892296, -16.42320221600525088 ) ) ;
#10893 = CARTESIAN_POINT ( 'NONE',  ( 116.6536748109119941, 0.9020085738987339008, -11.91225656197089222 ) ) ;
#10894 = AXIS2_PLACEMENT_3D ( 'NONE', #31945, #29432, #18277 ) ;
#10895 = CARTESIAN_POINT ( 'NONE',  ( 121.1918081442452859, -10.15424416112533912, -14.75197769757731336 ) ) ;
#10896 = AXIS2_PLACEMENT_3D ( 'NONE', #12166, #15581, #32446 ) ;
#10897 = CARTESIAN_POINT ( 'NONE',  ( 111.8886348109120092, -6.222761293078241884, -8.102969835052219238 ) ) ;
#10898 = CARTESIAN_POINT ( 'NONE',  ( 123.1205148109119563, -1.834011780172310813, -8.268836392978581529 ) ) ;
#10899 = EDGE_CURVE ( 'NONE', #8943, #38525, #14391, .T. ) ;
#10900 = CARTESIAN_POINT ( 'NONE',  ( 113.5385046295247804, -4.863998795839590272, -7.631215200338315796 ) ) ;
#10901 = CARTESIAN_POINT ( 'NONE',  ( 116.8805814775786445, -3.505236298600246325, -18.68346056562440793 ) ) ;
#10902 = CARTESIAN_POINT ( 'NONE',  ( 111.4665458264767750, -1.295815253274133161, -16.89579513612386563 ) ) ;
#10903 = EDGE_LOOP ( 'NONE', ( #21547, #7910, #6055, #20690, #12815 ) ) ;
#10904 = CARTESIAN_POINT ( 'NONE',  ( 123.0070614775786169, 0.9020085738987339008, -11.91225656197089222 ) ) ;
#10905 = CARTESIAN_POINT ( 'NONE',  ( 119.3961891859119930, -1.406689858478933353, -17.56299727309130887 ) ) ;
#10906 = CARTESIAN_POINT ( 'NONE',  ( 117.7882081442453170, -6.344957434206665248, -7.627207830600338134 ) ) ;
#10907 = VERTEX_POINT ( 'NONE', #4113 ) ;
#10908 = CARTESIAN_POINT ( 'NONE',  ( 115.2053796295247849, -4.863998795839590272, -19.15521520033831493 ) ) ;
#10909 = CARTESIAN_POINT ( 'NONE',  ( 121.9470836909669913, -29.69178914684045623, -14.92061247508468647 ) ) ;
#10910 = DIRECTION ( 'NONE',  ( 0.000000000000000000, 0.000000000000000000, -1.000000000000000000 ) ) ;
#10911 = CARTESIAN_POINT ( 'NONE',  ( 115.4056881442453459, -2.084020599724406786, -8.691656652584148546 ) ) ;
#10912 = CARTESIAN_POINT ( 'NONE',  ( 126.2184548109105435, -7.866424907533402511, -9.395035934245175469 ) ) ;
#10913 = EDGE_CURVE ( 'NONE', #24167, #4486, #478, .T. ) ;
#10914 = CARTESIAN_POINT ( 'NONE',  ( 121.5888948109119809, 0.1319031606808879209, -14.10382304977623669 ) ) ;
#10915 = DIRECTION ( 'NONE',  ( 0.000000000000000000, 0.000000000000000000, 1.000000000000000000 ) ) ;
#10916 = CARTESIAN_POINT ( 'NONE',  ( 120.8514481442452961, -2.084020599724406786, -8.691656652584148546 ) ) ;
#10917 = AXIS2_PLACEMENT_3D ( 'NONE', #2454, #19343, #27091 ) ;
#10918 = CARTESIAN_POINT ( 'NONE',  ( 119.7434548109119703, -12.80254289275730173, -14.38292102596908784 ) ) ;
#10919 = CARTESIAN_POINT ( 'NONE',  ( 117.7882081442453170, -3.505236298600246325, -18.68346056562440793 ) ) ;
#10920 = DIRECTION ( 'NONE',  ( 0.000000000000000000, -0.3818493186865936084, 0.9242245927363024194 ) ) ;
#10921 = CARTESIAN_POINT ( 'NONE',  ( 114.9518748109119883, -1.834011780172310813, -8.268836392978581529 ) ) ;
#10922 = CARTESIAN_POINT ( 'NONE',  ( 122.6009548109119720, 1.449227268523328505, -18.30678586333412738 ) ) ;
#10923 = CARTESIAN_POINT ( 'NONE',  ( 118.8092881442453290, -0.1624402480850797581, -16.17319339645315424 ) ) ;
#10924 = VERTEX_POINT ( 'NONE', #44975 ) ;
#10925 = CARTESIAN_POINT ( 'NONE',  ( 115.9162281442453235, -4.089484607189486809, -7.948022111789456723 ) ) ;
#10926 = CARTESIAN_POINT ( 'NONE',  ( 112.3578015045248861, -6.936859964151250502, -18.39754474579286025 ) ) ;
#10927 = LINE ( 'NONE', #35290, #19018 ) ;
#10928 = AXIS2_PLACEMENT_3D ( 'NONE', #27548, #6341, #34798 ) ;
#10929 = DIRECTION ( 'NONE',  ( 1.000000000000000000, 0.000000000000000000, 0.000000000000000000 ) ) ;
#10930 = CARTESIAN_POINT ( 'NONE',  ( 122.1561614775786353, -0.4660016031367893996, -10.09054647747474043 ) ) ;
#10931 = ORIENTED_EDGE ( 'NONE', *, *, #20330, .F. ) ;
#10932 = CARTESIAN_POINT ( 'NONE',  ( 126.6211808763552398, -8.557162640264039055, -9.730331182193353357 ) ) ;
#10933 = CARTESIAN_POINT ( 'NONE',  ( 121.6456214775786293, 0.4262465694468514643, -12.03445270309931736 ) ) ;
#10934 = DIRECTION ( 'NONE',  ( -0.7871354856660202071, 0.6167752151498580027, 0.002461946824133919541 ) ) ;
#10935 = CARTESIAN_POINT ( 'NONE',  ( 64.06702676307045863, -13.62987338852582653, -18.19193609654278276 ) ) ;
#10936 = LINE ( 'NONE', #437, #22441 ) ;
#10937 = CARTESIAN_POINT ( 'NONE',  ( 112.5661608795247872, -1.325403438956436419, -16.93181055722141792 ) ) ;
#10938 = DIRECTION ( 'NONE',  ( 0.000000000000000000, -0.3818493186865936084, 0.9242245927363024194 ) ) ;
#10939 = ORIENTED_EDGE ( 'NONE', *, *, #4208, .T. ) ;
#10940 = CARTESIAN_POINT ( 'NONE',  ( 115.9162281442453235, -4.089484607189486809, -7.948022111789456723 ) ) ;
#10941 = CARTESIAN_POINT ( 'NONE',  ( 124.5954081442453116, -6.222761293078241884, -8.102969835052219238 ) ) ;
#10942 = CARTESIAN_POINT ( 'NONE',  ( 123.3474214775786209, -9.988377603198976828, -10.36322818467138340 ) ) ;
#10943 = CARTESIAN_POINT ( 'NONE',  ( 117.1642148109119859, -0.8288870151387760510, -10.36305467784173118 ) ) ;
#10944 = CARTESIAN_POINT ( 'NONE',  ( 112.1722681442453222, -8.899110576539710493, -16.42337572283490132 ) ) ;
#10945 = DIRECTION ( 'NONE',  ( -0.000000000000000000, -0.9284778069183721172, -0.3713878862591650232 ) ) ;
#10946 = CARTESIAN_POINT ( 'NONE',  ( 122.7801548109119665, -3.383040157471821630, -19.15922257007629170 ) ) ;
#10947 = CARTESIAN_POINT ( 'NONE',  ( 74.66232006577804725, -2.500611837642884527, -8.143215200338314474 ) ) ;
#10948 = DIRECTION ( 'NONE',  ( 0.000000000000000000, 0.000000000000000000, -1.000000000000000000 ) ) ;
#10949 = CARTESIAN_POINT ( 'NONE',  ( 31.16203868753470019, 11.28474725185576055, -19.39321520033831447 ) ) ;
#10950 = CARTESIAN_POINT ( 'NONE',  ( 125.7866681442452688, -8.899110576539710493, -16.42337572283490132 ) ) ;
#10951 = ORIENTED_EDGE ( 'NONE', *, *, #17533, .T. ) ;
#10952 = EDGE_CURVE ( 'NONE', #7998, #40668, #38564, .T. ) ;
#10953 = CARTESIAN_POINT ( 'NONE',  ( 73.07463722459043254, -51.99713136313413031, -33.10717255453590013 ) ) ;
#10954 = CARTESIAN_POINT ( 'NONE',  ( 118.8660148109119774, -10.30919188438810075, -12.61870101168855918 ) ) ;
#10955 = CARTESIAN_POINT ( 'NONE',  ( 124.5386814775786206, -4.153390946401325223, -8.397313243818185668 ) ) ;
#10956 = ORIENTED_EDGE ( 'NONE', *, *, #7187, .T. ) ;
#10957 = CARTESIAN_POINT ( 'NONE',  ( 137.0134976903448774, 0.07479499832984452812, -11.07881363349517301 ) ) ;
#10958 = CARTESIAN_POINT ( 'NONE',  ( 122.6667014775786413, -7.893985811506177619, -18.51759400769804742 ) ) ;
#10959 = CARTESIAN_POINT ( 'NONE',  ( 107.6349890045248401, 0.8980012041604421569, -15.77991374673208469 ) ) ;
#10960 = CARTESIAN_POINT ( 'NONE',  ( 120.7947214775786193, -0.8288870151387760510, -10.36305467784173118 ) ) ;
#10961 = VERTEX_POINT ( 'NONE', #3459 ) ;
#10962 = CIRCLE ( 'NONE', #37911, 2.999999999999999556 ) ;
#10963 = CARTESIAN_POINT ( 'NONE',  ( 115.5758681442453053, -1.561330072975668060, -17.79121239304076951 ) ) ;
#10964 = EDGE_CURVE ( 'NONE', #35887, #5874, #44123, .T. ) ;
#10965 = DIRECTION ( 'NONE',  ( 0.000000000000000000, -1.000000000000000000, 0.000000000000000000 ) ) ;
#10966 = CIRCLE ( 'NONE', #26222, 2.000000000000000444 ) ;
#10967 = CARTESIAN_POINT ( 'NONE',  ( 120.8514481442452961, -7.893985811506198047, -18.51759400769803676 ) ) ;
#10968 = CARTESIAN_POINT ( 'NONE',  ( 138.2184548109119930, -9.609004340414083245, -9.721032963308941177 ) ) ;
#10969 = CARTESIAN_POINT ( 'NONE',  ( 125.1059481442452750, -8.166667518702819706, -8.995218007635861213 ) ) ;
#10970 = DIRECTION ( 'NONE',  ( 0.000000000000000000, -0.3818493186865927203, 0.9242245927363029745 ) ) ;
#10971 = CARTESIAN_POINT ( 'NONE',  ( 61.69189222814998175, -49.76310523276723785, -7.393215200338315363 ) ) ;
#10972 = CARTESIAN_POINT ( 'NONE',  ( 124.0848681442452772, -4.089484607189486809, -7.948022111789456723 ) ) ;
#10974 = CARTESIAN_POINT ( 'NONE',  ( 123.6877814775786533, -6.222761293078241884, -8.102969835052219238 ) ) ;
#10973 = CARTESIAN_POINT ( 'NONE',  ( 123.7445081442452874, -1.561330072975668948, -17.79121239304076951 ) ) ;
#10975 = CARTESIAN_POINT ( 'NONE',  ( 119.7169148109119874, -0.1624402480850797581, -16.17319339645315424 ) ) ;
#10976 = CARTESIAN_POINT ( 'NONE',  ( 114.4413348109119823, -9.261995988541697145, -16.69588392320189030 ) ) ;
#10977 = ORIENTED_EDGE ( 'NONE', *, *, #8493, .T. ) ;
#10978 = ORIENTED_EDGE ( 'NONE', *, *, #36456, .T. ) ;
#10979 = CARTESIAN_POINT ( 'NONE',  ( 93.44708369096697709, -25.99489077589524300, -13.39321520033831447 ) ) ;
#10980 = CARTESIAN_POINT ( 'NONE',  ( 69.69189222815028018, -41.76310523276638520, -10.39321520033831625 ) ) ;
#10981 = CARTESIAN_POINT ( 'NONE',  ( 113.9552233795247815, -1.325403438956436419, -9.854619843455211026 ) ) ;
#10982 = CARTESIAN_POINT ( 'NONE',  ( 106.7320983795247855, -8.402594152722688392, -16.93181055722141792 ) ) ;
#10983 = CARTESIAN_POINT ( 'NONE',  ( 115.3442858795247759, -8.402594152722688392, -9.854619843455216355 ) ) ;
#10984 = VECTOR ( 'NONE', #2571, 999.9999999999998863 ) ;
#10985 = EDGE_CURVE ( 'NONE', #35430, #33401, #29194, .T. ) ;
#10986 = CARTESIAN_POINT ( 'NONE',  ( 138.2184548109119930, 1.087851763053662602, -12.63461456455805276 ) ) ;
#10987 = CARTESIAN_POINT ( 'NONE',  ( 112.2289948109119848, -1.834011780172310813, -8.268836392978581529 ) ) ;
#10988 = ORIENTED_EDGE ( 'NONE', *, *, #6360, .F. ) ;
#10989 = CARTESIAN_POINT ( 'NONE',  ( 114.7249681442453237, -9.565557343593413364, -10.61323700422348004 ) ) ;
#10990 = CARTESIAN_POINT ( 'NONE',  ( 111.2465515045248168, -2.477300249445798297, -7.631215200338321125 ) ) ;
#10991 = CARTESIAN_POINT ( 'NONE',  ( 118.8660148109119774, 0.1319031606808853119, -14.10382304977625800 ) ) ;
#10992 = DIRECTION ( 'NONE',  ( -0.5735764363510446051, 0.3127926500124816878, -0.7570804645221042017 ) ) ;
#10993 =( BOUNDED_SURFACE ( )  B_SPLINE_SURFACE ( 3, 2, ( 
 ( #44795, #9448, #24268 ),
 ( #41602, #31093, #30651 ),
 ( #34284, #33827, #38156 ),
 ( #24045, #2598, #23362 ) ),
 .UNSPECIFIED., .F., .F., .F. ) 
 B_SPLINE_SURFACE_WITH_KNOTS ( ( 4, 4 ),
 ( 3, 3 ),
 ( 1.570796326794896558, 1.618943030528137816 ),
 ( 0.000000000000000000, 1.000000000000000000 ),
 .UNSPECIFIED. ) 
 GEOMETRIC_REPRESENTATION_ITEM ( )  RATIONAL_B_SPLINE_SURFACE ( (
 ( 1.000000000000000000, 0.7071067811865475727, 1.000000000000000000),
 ( 1.000000000000000000, 0.7095941637304925553, 1.000000000000000000),
 ( 1.000000000000000000, 0.7120684114869151315, 1.000000000000000000),
 ( 1.000000000000000000, 0.7145271066604789167, 1.000000000000000000) ) ) 
 REPRESENTATION_ITEM ( '' )  SURFACE ( )  );
#10994 = CARTESIAN_POINT ( 'NONE',  ( 124.5386814775786206, -5.638512984488999180, -18.83840828888717311 ) ) ;
#10995 = CARTESIAN_POINT ( 'NONE',  ( -13.23547271986589990, -4.036892331970093117, -19.09970410335115787 ) ) ;
#10996 = CARTESIAN_POINT ( 'NONE',  ( 117.5045748109119756, 0.5811942927096110934, -14.16772938898807510 ) ) ;
#10997 = CARTESIAN_POINT ( 'NONE',  ( 115.0664733795247798, -8.938348069036489818, -17.46756447353520159 ) ) ;
#10998 = CARTESIAN_POINT ( 'NONE',  ( 111.4549108795247747, -1.325403438956436419, -16.93181055722141792 ) ) ;
#10999 = VERTEX_POINT ( 'NONE', #42886 ) ;
#11000 = CARTESIAN_POINT ( 'NONE',  ( 91.65862616933031859, -24.14644159042263993, -12.62951656296512937 ) ) ;
#11001 = CIRCLE ( 'NONE', #15386, 3.499999999999998668 ) ;
#11002 = CARTESIAN_POINT ( 'NONE',  ( 115.5758681442453053, -7.894159318335828068, -9.358103419637847864 ) ) ;
#11003 = CARTESIAN_POINT ( 'NONE',  ( 114.1009748109119784, -4.089484607189486809, -7.948022111789456723 ) ) ;
#11004 = CARTESIAN_POINT ( 'NONE',  ( 108.6767858795247861, -8.402594152722688392, -9.854619843455216355 ) ) ;
#11005 = AXIS2_PLACEMENT_3D ( 'NONE', #384, #28214, #4019 ) ;
#11006 = CARTESIAN_POINT ( 'NONE',  ( 118.2987481442453088, -7.894159318335806752, -9.358103419637831877 ) ) ;
#11007 = CARTESIAN_POINT ( 'NONE',  ( 118.2987481442453088, -7.894159318335828068, -9.358103419637847864 ) ) ;
#11008 = CARTESIAN_POINT ( 'NONE',  ( 126.0703014775786102, -9.988377603198980381, -10.36322818467138518 ) ) ;
#11009 = ORIENTED_EDGE ( 'NONE', *, *, #5018, .T. ) ;
#11010 = CARTESIAN_POINT ( 'NONE',  ( 120.8547048109119686, -2.527210466738041728, -8.967976844669124148 ) ) ;
#11011 = DIRECTION ( 'NONE',  ( 0.000000000000000000, 0.000000000000000000, -1.000000000000000000 ) ) ;
#11012 = CARTESIAN_POINT ( 'NONE',  ( 113.5337081442453240, -0.8288870151387760510, -10.36305467784173118 ) ) ;
#11013 = ORIENTED_EDGE ( 'NONE', *, *, #35176, .F. ) ;
#11014 = CARTESIAN_POINT ( 'NONE',  ( 126.7702028005465422, -9.551180355136843048, -15.81524199167786193 ) ) ;
#11015 = CARTESIAN_POINT ( 'NONE',  ( 106.4542858795248179, -0.7896495226426338832, -17.46756447353520159 ) ) ;
#11016 = CARTESIAN_POINT ( 'NONE',  ( 109.8574890045247940, -9.868328341294098749, -11.32035403202665869 ) ) ;
#11017 = CARTESIAN_POINT ( 'NONE',  ( 124.5954081442453116, -6.222761293078241884, -8.102969835052219238 ) ) ;
#11018 = VERTEX_POINT ( 'NONE', #1591 ) ;
#11019 = VECTOR ( 'NONE', #24170, 1000.000000000000000 ) ;
#11020 = CARTESIAN_POINT ( 'NONE',  ( 119.0929214775786278, -4.153390946401325223, -8.397313243818185668 ) ) ;
#11021 = ADVANCED_FACE ( 'NONE', ( #32383 ), #15312, .T. ) ;
#11022 = CARTESIAN_POINT ( 'NONE',  ( 115.6893214775786447, -9.859900752359374465, -12.68260735090039404 ) ) ;
#11023 = CARTESIAN_POINT ( 'NONE',  ( 124.5466134613335214, -9.859322667160077103, -13.15779651595278565 ) ) ;
#11024 = CARTESIAN_POINT ( 'NONE',  ( 122.7993923109119692, -9.959231468620755479, -10.70263013195267199 ) ) ;
#11025 = EDGE_LOOP ( 'NONE', ( #1417, #7779, #10988, #44727 ) ) ;
#11026 = CARTESIAN_POINT ( 'NONE',  ( 75.95778847736514194, -3.256761025687008537, -7.147228641687434880 ) ) ;
#11027 = DIRECTION ( 'NONE',  ( -1.000000000000000000, 0.000000000000000000, 0.000000000000000000 ) ) ;
#11028 = CARTESIAN_POINT ( 'NONE',  ( 109.0935046295247872, -4.863998795839590272, -7.631215200338315796 ) ) ;
#11029 = VECTOR ( 'NONE', #16048, 1000.000000000000000 ) ;
#11030 = CARTESIAN_POINT ( 'NONE',  ( 69.36136150295220659, -51.83082107656346693, -30.83034926238675411 ) ) ;
#11031 = CARTESIAN_POINT ( 'NONE',  ( 112.7395348109119766, -5.638512984488999180, -18.83840828888717311 ) ) ;
#11032 = CARTESIAN_POINT ( 'NONE',  ( 117.9016614775786280, -0.1624402480850797581, -16.17319339645315424 ) ) ;
#11033 = CARTESIAN_POINT ( 'NONE',  ( 125.2713867217341885, -7.074789275518575948, -20.29960597128161837 ) ) ;
#11034 = ORIENTED_EDGE ( 'NONE', *, *, #34241, .T. ) ;
#11035 = CARTESIAN_POINT ( 'NONE',  ( 115.1220548109119761, -1.833838273342658809, -17.42832698103878286 ) ) ;
#11036 = CARTESIAN_POINT ( 'NONE',  ( 115.7610046295247912, -4.863998795839590272, -7.631215200338315796 ) ) ;
#11037 = CARTESIAN_POINT ( 'NONE',  ( 115.3442858795247759, -0.7896495226426338832, -17.46756447353520159 ) ) ;
#11038 = CARTESIAN_POINT ( 'NONE',  ( 114.6682414775786469, -1.561330072975668060, -17.79121239304076596 ) ) ;
#11039 = ORIENTED_EDGE ( 'NONE', *, *, #39491, .T. ) ;
#11040 = CARTESIAN_POINT ( 'NONE',  ( 115.6893214775786447, 0.5811942927096154232, -14.16772938898807155 ) ) ;
#11041 = LINE ( 'NONE', #28150, #37069 ) ;
#11042 = CARTESIAN_POINT ( 'NONE',  ( 111.5243640045248412, -10.62599879583958717, -11.00651665394454604 ) ) ;
#11043 = CARTESIAN_POINT ( 'NONE',  ( 113.7606148109119886, -1.561330072975668060, -17.79121239304076596 ) ) ;
#11044 = CARTESIAN_POINT ( 'NONE',  ( 113.6471614775786492, -5.638512984488999180, -18.83840828888717311 ) ) ;
#11045 = CARTESIAN_POINT ( 'NONE',  ( 126.5041214912230032, -10.00604656586921593, -13.30322242015582823 ) ) ;
#11046 = CARTESIAN_POINT ( 'NONE',  ( 69.48536631248848039, -69.56066907060868232, -44.09544185076553191 ) ) ;
#11047 = CARTESIAN_POINT ( 'NONE',  ( 111.8021765045248372, -2.791137627527939813, -8.388885654883777576 ) ) ;
#11048 = VERTEX_POINT ( 'NONE', #15287 ) ;
#11049 = CARTESIAN_POINT ( 'NONE',  ( 70.19189222814998175, -54.26662894631272849, -34.90947156805651019 ) ) ;
#11050 = CARTESIAN_POINT ( 'NONE',  ( 109.2294778858186390, -2.837229698210430140, -18.06364092945466382 ) ) ;
#11051 = CIRCLE ( 'NONE', #111, 5.000000000000000000 ) ;
#11052 = CARTESIAN_POINT ( 'NONE',  ( 116.0296814775786345, -1.833838273342658809, -17.42832698103878286 ) ) ;
#11053 = DIRECTION ( 'NONE',  ( -0.9908103287288504424, 0.1352586133457951423, 0.000000000000000000 ) ) ;
#11054 = CARTESIAN_POINT ( 'NONE',  ( 114.7886608795247696, -1.325403438956436419, -16.93181055722141792 ) ) ;
#11055 = CARTESIAN_POINT ( 'NONE',  ( 110.2047546295247855, -4.863998795839590272, -7.631215200338315796 ) ) ;
#11056 = DIRECTION ( 'NONE',  ( -0.000000000000000000, -0.3818493186865896671, 0.9242245927363040847 ) ) ;
#11057 = CARTESIAN_POINT ( 'NONE',  ( 115.3489614775786407, -0.8288870151387760510, -10.36305467784173118 ) ) ;
#11058 = DIRECTION ( 'NONE',  ( -0.000000000000000000, -0.9284778069183721172, -0.3713878862591650232 ) ) ;
#11059 = CARTESIAN_POINT ( 'NONE',  ( 125.5030348109119558, -3.383040157471821630, -19.15922257007629170 ) ) ;
#11060 = EDGE_CURVE ( 'NONE', #42171, #26936, #2877, .T. ) ;
#11061 = CARTESIAN_POINT ( 'NONE',  ( 116.7104014775786425, -0.4660016031367893996, -10.09054647747474043 ) ) ;
#11062 = ORIENTED_EDGE ( 'NONE', *, *, #44306, .F. ) ;
#11063 = CARTESIAN_POINT ( 'NONE',  ( 113.3635281442453504, -0.1624402480850797581, -16.17319339645315424 ) ) ;
#11064 = CARTESIAN_POINT ( 'NONE',  ( 111.8886348109120092, -3.383040157471821630, -19.15922257007629170 ) ) ;
#11065 = CARTESIAN_POINT ( 'NONE',  ( 117.2209414775786485, -7.893985811506177619, -18.51759400769804742 ) ) ;
#11066 = CARTESIAN_POINT ( 'NONE',  ( 116.0296814775786345, -1.833838273342658809, -17.42832698103878286 ) ) ;
#11067 = VERTEX_POINT ( 'NONE', #15512 ) ;
#11068 = CARTESIAN_POINT ( 'NONE',  ( 120.3976348109119812, -7.643976991954077427, -18.09477374809248928 ) ) ;
#11069 = CARTESIAN_POINT ( 'NONE',  ( 118.5256548109119876, -0.4660016031367893996, -10.09054647747474043 ) ) ;
#11070 = CARTESIAN_POINT ( 'NONE',  ( 136.7439301332540538, 0.3743339856268463883, -15.44589132379487317 ) ) ;
#11071 = CARTESIAN_POINT ( 'NONE',  ( 109.8574890045247940, 0.8980012041604421569, -15.77991374673208469 ) ) ;
#11072 = CARTESIAN_POINT ( 'NONE',  ( 61.76166819791257012, -14.46743153019240147, -8.940005687461745509 ) ) ;
#11073 = CARTESIAN_POINT ( 'NONE',  ( 126.8093656611956845, 0.4289529172945278357, -13.23035857857622766 ) ) ;
#11074 = ADVANCED_FACE ( 'NONE', ( #39230 ), #43106, .T. ) ;
#11075 = B_SPLINE_CURVE_WITH_KNOTS ( 'NONE', 3,
 ( #44096, #41363, #13307, #27441, #37912, #23113, #2345, #37458, #36990, #33568 ),
 .UNSPECIFIED., .F., .F.,
 ( 4, 3, 3, 4 ),
 ( 0.000000000000000000, 0.0001671877548681235048, 0.0003343755096277615233, 0.0006463528481650619413 ),
 .UNSPECIFIED. ) ;
#11076 = CARTESIAN_POINT ( 'NONE',  ( 116.0388171295248014, 0.1403307496149613920, -13.39321520033831447 ) ) ;
#11077 = CARTESIAN_POINT ( 'NONE',  ( 113.3068014775786594, -8.166667518702817929, -8.995218007635859436 ) ) ;
#11078 = CARTESIAN_POINT ( 'NONE',  ( 117.1872882340475996, 1.416175236645604851, -5.259658493298883464 ) ) ;
#11079 = CARTESIAN_POINT ( 'NONE',  ( 115.0653281442453277, -3.505236298600246325, -18.68346056562440793 ) ) ;
#11080 = EDGE_CURVE ( 'NONE', #19235, #8204, #40046, .T. ) ;
#11081 = CARTESIAN_POINT ( 'NONE',  ( 111.2212166496844787, 0.5600166689815611054, -12.14321520033830026 ) ) ;
#11082 = CARTESIAN_POINT ( 'NONE',  ( -13.78505786849281911, -3.796669023460695680, -8.693443890614471314 ) ) ;
#11083 = CARTESIAN_POINT ( 'NONE',  ( 114.2330358795247776, -8.402594152722688392, -9.854619843455216355 ) ) ;
#11084 = CARTESIAN_POINT ( 'NONE',  ( 114.2711548109119803, -0.1624402480850797581, -16.17319339645315424 ) ) ;
#11085 = ADVANCED_FACE ( 'NONE', ( #8226 ), #21903, .T. ) ;
#11086 = AXIS2_PLACEMENT_3D ( 'NONE', #21179, #38487, #34833 ) ;
#11087 = CARTESIAN_POINT ( 'NONE',  ( 125.1733191598100916, -1.295815253274133161, -16.89579513612386563 ) ) ;
#11089 = CARTESIAN_POINT ( 'NONE',  ( 119.4332814775786318, -0.4660016031367893996, -10.09054647747474043 ) ) ;
#11088 = LINE ( 'NONE', #3349, #28742 ) ;
#11090 = CARTESIAN_POINT ( 'NONE',  ( 125.1626748109119802, -0.1624402480850797581, -16.17319339645315424 ) ) ;
#11091 = CARTESIAN_POINT ( 'NONE',  ( 120.6245414775786458, -0.1624402480850797581, -16.17319339645315424 ) ) ;
#11092 = CARTESIAN_POINT ( 'NONE',  ( 112.0588148109119828, -9.859900752359374465, -12.68260735090039404 ) ) ;
#11093 = EDGE_LOOP ( 'NONE', ( #24112, #23835, #30626, #11180 ) ) ;
#11094 = CARTESIAN_POINT ( 'NONE',  ( 137.2618751060991258, -7.298444271412085627, -8.736063270064514441 ) ) ;
#11095 = CARTESIAN_POINT ( 'NONE',  ( 121.7590748109119687, -7.893985811506177619, -18.51759400769804742 ) ) ;
#11096 = CARTESIAN_POINT ( 'NONE',  ( 115.7610046295247912, -4.863998795839590272, -18.39754474579285315 ) ) ;
#11097 = CARTESIAN_POINT ( 'NONE',  ( 120.3976348109119812, -7.643976991954077427, -18.09477374809248928 ) ) ;
#11098 = CARTESIAN_POINT ( 'NONE',  ( 117.0507614775786465, 0.1319031606808879209, -14.10382304977623669 ) ) ;
#11099 = CARTESIAN_POINT ( 'NONE',  ( 85.99639782577784786, -27.24303960391588220, -8.592445736787643895 ) ) ;
#11100 = CARTESIAN_POINT ( 'NONE',  ( 113.9552233795247815, -8.938348069036489818, -17.46756447353520159 ) ) ;
#11101 = CARTESIAN_POINT ( 'NONE',  ( 118.5823814775786360, -7.643976991954077427, -18.09477374809248928 ) ) ;
#11102 = CARTESIAN_POINT ( 'NONE',  ( 125.5597614775786326, -7.894159318335828068, -9.358103419637847864 ) ) ;
#11103 = FACE_OUTER_BOUND ( 'NONE', #15141, .T. ) ;
#11104 = CARTESIAN_POINT ( 'NONE',  ( 109.2294582674637269, -1.259376031108396354, -9.372254076597803518 ) ) ;
#11105 = CARTESIAN_POINT ( 'NONE',  ( 122.0354079359119908, -4.360204210389833968, -8.000047426360245240 ) ) ;
#11106 = CARTESIAN_POINT ( 'NONE',  ( 113.5385046295247804, -4.863998795839590272, -7.631215200338315796 ) ) ;
#11107 = EDGE_CURVE ( 'NONE', #42191, #21542, #37128, .T. ) ;
#11108 = CARTESIAN_POINT ( 'NONE',  ( 83.86216108596053687, -31.76310523276723430, -22.89321520033831803 ) ) ;
#11109 = CARTESIAN_POINT ( 'NONE',  ( 117.9016614775786280, -9.988377603198976828, -10.36322818467138340 ) ) ;
#11110 = CARTESIAN_POINT ( 'NONE',  ( 114.2144281442453178, -8.166667518702817929, -8.995218007635859436 ) ) ;
#11111 = CARTESIAN_POINT ( 'NONE',  ( 112.6356140045247827, -10.62599879583958717, -11.00651665394454604 ) ) ;
#11112 = CARTESIAN_POINT ( 'NONE',  ( 111.7751814775786556, -7.893985811506177619, -18.51759400769804742 ) ) ;
#11113 = ADVANCED_FACE ( 'NONE', ( #8671 ), #32800, .T. ) ;
#11114 = EDGE_CURVE ( 'NONE', #3780, #4318, #14, .T. ) ;
#11115 = ORIENTED_EDGE ( 'NONE', *, *, #8880, .F. ) ;
#11116 = CONICAL_SURFACE ( 'NONE', #43203, 2.999999999999999556, 0.9599310885968830309 ) ;
#11117 = CARTESIAN_POINT ( 'NONE',  ( 124.3685014775786328, -10.63000616557722466, -14.87417383870573495 ) ) ;
#11118 = AXIS2_PLACEMENT_3D ( 'NONE', #44874, #6332, #13630 ) ;
#11119 = CARTESIAN_POINT ( 'NONE',  ( 117.5045748109119756, 0.5811942927096110934, -14.16772938898807510 ) ) ;
#11120 = CARTESIAN_POINT ( 'NONE',  ( 120.6812681442452941, 0.1319031606808879209, -14.10382304977623669 ) ) ;
#11121 = CARTESIAN_POINT ( 'NONE',  ( 125.5030348109119558, -3.383040157471821630, -19.15922257007629170 ) ) ;
#11122 = CARTESIAN_POINT ( 'NONE',  ( 123.0070614775786169, 0.9020085738987339008, -11.91225656197089222 ) ) ;
#11123 = CARTESIAN_POINT ( 'NONE',  ( 113.7468640045248236, -10.62599879583958717, -11.00651665394454604 ) ) ;
#11124 = CIRCLE ( 'NONE', #18380, 12.50000000000000178 ) ;
#11125 = CARTESIAN_POINT ( 'NONE',  ( 116.5402214775786405, -9.565557343593413364, -10.61323700422348004 ) ) ;
#11126 = DIRECTION ( 'NONE',  ( -1.000000000000000000, 0.000000000000000000, 0.000000000000000000 ) ) ;
#11127 = VERTEX_POINT ( 'NONE', #24227 ) ;
#11128 = CARTESIAN_POINT ( 'NONE',  ( 120.5110881442453206, -6.344957434206665248, -7.627207830600338134 ) ) ;
#11129 = CARTESIAN_POINT ( 'NONE',  ( 119.7434548109119703, -2.527210466738041728, -8.967976844669124148 ) ) ;
#11130 = CARTESIAN_POINT ( 'NONE',  ( 117.9016614775786280, -9.988377603198976828, -10.36322818467138340 ) ) ;
#11131 = ORIENTED_EDGE ( 'NONE', *, *, #41046, .F. ) ;
#11132 = CARTESIAN_POINT ( 'NONE',  ( 115.7610046295247912, -4.863998795839590272, -7.631215200338315796 ) ) ;
#11133 = CARTESIAN_POINT ( 'NONE',  ( 64.70242381814703947, -2.666228601359576622, -8.189135705538296506 ) ) ;
#11134 = CARTESIAN_POINT ( 'NONE',  ( 71.02242295334774269, -58.76687921697075723, -39.81436363781143228 ) ) ;
#11135 = CARTESIAN_POINT ( 'NONE',  ( 114.3846081442453197, 0.4262465694468514643, -12.03445270309931736 ) ) ;
#11136 = CARTESIAN_POINT ( 'NONE',  ( 65.34289968162609341, -37.75951406093616214, -4.893215200338314474 ) ) ;
#11137 = CARTESIAN_POINT ( 'NONE',  ( 123.8818742721482664, -2.287189184988711155, -18.07361239780447448 ) ) ;
#11138 = CARTESIAN_POINT ( 'NONE',  ( 121.6456214775786293, 0.4262465694468514643, -12.03445270309931736 ) ) ;
#11139 = CARTESIAN_POINT ( 'NONE',  ( 121.0890424739651507, 0.3208234527006196823, -15.99825685930876595 ) ) ;
#11140 = AXIS2_PLACEMENT_3D ( 'NONE', #17078, #6123, #20042 ) ;
#11141 = CARTESIAN_POINT ( 'NONE',  ( 121.9859814775786333, -9.565557343593413364, -10.61323700422348004 ) ) ;
#11142 = ADVANCED_FACE ( 'NONE', ( #32167 ), #32762, .T. ) ;
#11143 = DIRECTION ( 'NONE',  ( 0.000000000000000000, -0.9242245927363029745, -0.3818493186865927203 ) ) ;
#11144 = CARTESIAN_POINT ( 'NONE',  ( 119.1496481442453046, -6.222761293078241884, -8.102969835052219238 ) ) ;
#11145 = CARTESIAN_POINT ( 'NONE',  ( 114.0442481442453300, -1.834011780172310813, -8.268836392978581529 ) ) ;
#11146 = CARTESIAN_POINT ( 'NONE',  ( 119.3765548109119834, 0.9020085738987339008, -11.91225656197089222 ) ) ;
#11147 = CARTESIAN_POINT ( 'NONE',  ( 112.6828081442453282, -7.893985811506177619, -18.51759400769804742 ) ) ;
#11148 = DIRECTION ( 'NONE',  ( 0.000000000000000000, 0.9284778069183720062, 0.3713878862591650232 ) ) ;
#11149 = CARTESIAN_POINT ( 'NONE',  ( 120.9649014775786355, -6.222761293078241884, -8.102969835052219238 ) ) ;
#11150 = VERTEX_POINT ( 'NONE', #27870 ) ;
#11151 = CARTESIAN_POINT ( 'NONE',  ( 117.4478481442453131, 0.2603800115204892296, -16.42320221600525088 ) ) ;
#11152 = CARTESIAN_POINT ( 'NONE',  ( 115.4831921295247952, -9.868328341294093420, -13.39321520033831447 ) ) ;
#11153 = DIRECTION ( 'NONE',  ( -1.000000000000000000, 0.000000000000000000, 0.000000000000000000 ) ) ;
#11154 = AXIS2_PLACEMENT_3D ( 'NONE', #26153, #15671, #43491 ) ;
#11155 = CARTESIAN_POINT ( 'NONE',  ( 114.4413952545248350, -9.868328341294102302, -15.46607636865002355 ) ) ;
#11156 = LINE ( 'NONE', #44930, #38589 ) ;
#11157 = CARTESIAN_POINT ( 'NONE',  ( 122.2696148109119889, -4.089484607189486809, -7.948022111789456723 ) ) ;
#11158 = ORIENTED_EDGE ( 'NONE', *, *, #38394, .F. ) ;
#11159 = CARTESIAN_POINT ( 'NONE',  ( 126.3444272079758406, -8.232969492540654244, -9.613686683291632562 ) ) ;
#11160 = CARTESIAN_POINT ( 'NONE',  ( 121.4187148109119789, -3.505236298600246325, -18.68346056562440793 ) ) ;
#11161 = CARTESIAN_POINT ( 'NONE',  ( 59.41476255453773803, -13.68180535374018092, -19.39321520033831803 ) ) ;
#11162 = CARTESIAN_POINT ( 'NONE',  ( 64.18180727272476815, -15.10249645379742667, -18.01844049509142920 ) ) ;
#11163 = EDGE_CURVE ( 'NONE', #33002, #19823, #35670, .T. ) ;
#11164 = CARTESIAN_POINT ( 'NONE',  ( 126.0135748109119902, -8.166667518702819706, -8.995218007635861213 ) ) ;
#11165 = CARTESIAN_POINT ( 'NONE',  ( 111.1770983795247787, -8.402594152722688392, -16.93181055722141792 ) ) ;
#11166 = ORIENTED_EDGE ( 'NONE', *, *, #26228, .T. ) ;
#11167 = CARTESIAN_POINT ( 'NONE',  ( 115.7460481442453357, 0.9020085738987339008, -11.91225656197089222 ) ) ;
#11168 = CARTESIAN_POINT ( 'NONE',  ( 115.4056881442453459, -7.893985811506177619, -18.51759400769804742 ) ) ;
#11169 = CARTESIAN_POINT ( 'NONE',  ( 88.69904943327698277, -11.18046741462036842, -14.08431115565796254 ) ) ;
#11170 = EDGE_CURVE ( 'NONE', #20392, #8490, #10539, .T. ) ;
#11171 = CARTESIAN_POINT ( 'NONE',  ( 120.5678148109119832, -1.833838273342659253, -17.42832698103878286 ) ) ;
#11172 = CARTESIAN_POINT ( 'NONE',  ( 126.2872529661399597, -3.846216389819564707, -8.462751213476616741 ) ) ;
#11173 = CARTESIAN_POINT ( 'NONE',  ( 68.68839935636917460, -25.95913848132418522, -5.893215200338315363 ) ) ;
#11174 = CARTESIAN_POINT ( 'NONE',  ( 122.3263414775786373, -6.344957434206665248, -7.627207830600338134 ) ) ;
#11175 = CARTESIAN_POINT ( 'NONE',  ( 111.4915481442453142, -1.833838273342658365, -17.42832698103878286 ) ) ;
#11176 = ADVANCED_FACE ( 'NONE', ( #14401 ), #20321, .T. ) ;
#11177 = CARTESIAN_POINT ( 'NONE',  ( 67.37136766119182596, -67.53150897494617766, -41.09057840265009531 ) ) ;
#11178 = LINE ( 'NONE', #35544, #11368 ) ;
#11179 = CARTESIAN_POINT ( 'NONE',  ( 112.5126281442453120, -10.30919188438810075, -12.61870101168855918 ) ) ;
#11180 = ORIENTED_EDGE ( 'NONE', *, *, #18143, .F. ) ;
#11181 = CIRCLE ( 'NONE', #43950, 2.000000000000000444 ) ;
#11182 = CARTESIAN_POINT ( 'NONE',  ( 115.5526452545247622, -9.868328341294098749, -15.46607636864997204 ) ) ;
#11183 = CARTESIAN_POINT ( 'NONE',  ( 120.6245414775786458, -9.988377603198976828, -10.36322818467138340 ) ) ;
#11184 = CARTESIAN_POINT ( 'NONE',  ( 59.90552009294157898, -2.897503654462289191, -17.89321520033831447 ) ) ;
#11185 = ORIENTED_EDGE ( 'NONE', *, *, #26323, .T. ) ;
#11186 = CARTESIAN_POINT ( 'NONE',  ( 135.5886503745695677, 0.7166931025281868539, -11.18974842684922066 ) ) ;
#11187 = CARTESIAN_POINT ( 'NONE',  ( 125.2761281442453054, -10.63000616557722466, -14.87417383870573495 ) ) ;
#11188 = DIRECTION ( 'NONE',  ( 0.000000000000000000, -0.9242245927363029745, -0.3818493186865927758 ) ) ;
#11189 = CARTESIAN_POINT ( 'NONE',  ( 123.3474214775786209, -0.1624402480850797581, -16.17319339645315424 ) ) ;
#11190 = AXIS2_PLACEMENT_3D ( 'NONE', #38038, #17511, #38467 ) ;
#11191 = ORIENTED_EDGE ( 'NONE', *, *, #14710, .T. ) ;
#11192 = CARTESIAN_POINT ( 'NONE',  ( 113.8173414775786512, 0.2603800115204892296, -16.42320221600525088 ) ) ;
#11193 = CARTESIAN_POINT ( 'NONE',  ( 117.2294421295247844, 1.035107641088057973, -5.059859068394715109 ) ) ;
#11194 = CARTESIAN_POINT ( 'NONE',  ( 112.8721930757767495, -0.9924539043446216624, -17.29976612834909133 ) ) ;
#11195 = CARTESIAN_POINT ( 'NONE',  ( 111.4705635773848940, -2.467220198592768199, -17.83387418641523325 ) ) ;
#11196 = CARTESIAN_POINT ( 'NONE',  ( 125.5030348109119558, -3.383040157471821630, -19.15922257007629170 ) ) ;
#11197 = DIRECTION ( 'NONE',  ( -1.000000000000000000, 0.000000000000000000, 0.000000000000000000 ) ) ;
#11198 = CARTESIAN_POINT ( 'NONE',  ( 70.19189222814998175, -57.62004466406304459, -36.25082616574700722 ) ) ;
#11199 = CARTESIAN_POINT ( 'NONE',  ( 124.6521348109119884, -1.561330072975668948, -17.79121239304076951 ) ) ;
#11201 = CARTESIAN_POINT ( 'NONE',  ( 122.6667014775786413, -2.084020599724406786, -8.691656652584148546 ) ) ;
#11200 = CARTESIAN_POINT ( 'NONE',  ( 123.8579614775786126, 0.5811942927096110934, -14.16772938898807510 ) ) ;
#11202 = CARTESIAN_POINT ( 'NONE',  ( 121.8158014775786171, -4.153390946401325223, -8.397313243818185668 ) ) ;
#11203 = B_SPLINE_CURVE_WITH_KNOTS ( 'NONE', 3,
 ( #16450, #1839, #26030, #9375, #15768, #1617, #19632, #15538, #37168, #2296 ),
 .UNSPECIFIED., .F., .F.,
 ( 4, 3, 3, 4 ),
 ( 0.000000000000000000, 0.0001671877560958130043, 0.0003343755126086615011, 0.0006438490228505480001 ),
 .UNSPECIFIED. ) ;
#11204 = DIRECTION ( 'NONE',  ( 1.000000000000000000, -1.488292102367680609E-29, 1.981883451652704298E-29 ) ) ;
#11205 = CARTESIAN_POINT ( 'NONE',  ( 120.5678148109119832, -8.166667518702819706, -8.995218007635861213 ) ) ;
#11206 = VERTEX_POINT ( 'NONE', #29652 ) ;
#11207 = EDGE_CURVE ( 'NONE', #17, #2333, #7294, .T. ) ;
#11208 = ORIENTED_EDGE ( 'NONE', *, *, #31399, .T. ) ;
#11209 = DIRECTION ( 'NONE',  ( 1.000000000000000000, 0.000000000000000000, -0.000000000000000000 ) ) ;
#11210 = CARTESIAN_POINT ( 'NONE',  ( 115.0664733795247798, -8.938348069036489818, -17.46756447353520159 ) ) ;
#11211 = CARTESIAN_POINT ( 'NONE',  ( 113.8857702545248003, 0.1403307496149616695, -11.32035403202665336 ) ) ;
#11212 = CARTESIAN_POINT ( 'NONE',  ( 112.1494421295248003, -9.868328341294093420, -13.39321520033831447 ) ) ;
#11213 = CARTESIAN_POINT ( 'NONE',  ( 125.9001214775786224, -4.089484607189486809, -7.948022111789456723 ) ) ;
#11214 = CARTESIAN_POINT ( 'NONE',  ( 126.1270281442452870, 0.1319031606808879209, -14.10382304977623669 ) ) ;
#11215 = ORIENTED_EDGE ( 'NONE', *, *, #3272, .T. ) ;
#11216 = CARTESIAN_POINT ( 'NONE',  ( 114.1577014775786552, -3.505236298600246325, -18.68346056562440793 ) ) ;
#11217 = CARTESIAN_POINT ( 'NONE',  ( 107.1488171295247867, -10.62599879583958540, -13.39321520033831447 ) ) ;
#11218 = CARTESIAN_POINT ( 'NONE',  ( 118.8209181415389111, -0.1020945015694968705, -15.74893487844867757 ) ) ;
#11219 = CARTESIAN_POINT ( 'NONE',  ( 125.6732148109119862, 0.5811942927096110934, -14.16772938898807510 ) ) ;
#11220 = CARTESIAN_POINT ( 'NONE',  ( 126.1837548109119211, -10.63000616557722466, -14.87417383870573495 ) ) ;
#11221 = CARTESIAN_POINT ( 'NONE',  ( -13.60484295501412433, -3.877462935949435252, -18.65581272914820588 ) ) ;
#11222 = CARTESIAN_POINT ( 'NONE',  ( 117.1074881442453233, -10.63000616557722466, -14.87417383870573495 ) ) ;
#11223 = CARTESIAN_POINT ( 'NONE',  ( 113.4690515045247992, -2.477300249445798297, -7.631215200338321125 ) ) ;
#11224 = CARTESIAN_POINT ( 'NONE',  ( 113.1912390045248031, -9.868328341294098749, -11.32035403202665869 ) ) ;
#11225 = ORIENTED_EDGE ( 'NONE', *, *, #16779, .T. ) ;
#11226 = LINE ( 'NONE', #25133, #39827 ) ;
#11227 = CARTESIAN_POINT ( 'NONE',  ( 113.7038881442453402, -6.222761293078241884, -8.102969835052219238 ) ) ;
#11228 = CARTESIAN_POINT ( 'NONE',  ( 126.6942948109119840, -8.899110576539710493, -16.42337572283490132 ) ) ;
#11229 = FACE_OUTER_BOUND ( 'NONE', #17341, .T. ) ;
#11230 = CARTESIAN_POINT ( 'NONE',  ( 124.0281414775786146, -7.643976991954077427, -18.09477374809248928 ) ) ;
#11231 = CARTESIAN_POINT ( 'NONE',  ( 118.5256548109119876, -8.899110576539710493, -16.42337572283490132 ) ) ;
#11232 = CARTESIAN_POINT ( 'NONE',  ( 115.8595014775786609, -7.643976991954077427, -18.09477374809248928 ) ) ;
#11233 = ORIENTED_EDGE ( 'NONE', *, *, #12476, .F. ) ;
#11234 = CARTESIAN_POINT ( 'NONE',  ( 123.8411891859119862, -1.406689858478933353, -17.56299727309130887 ) ) ;
#11235 = CARTESIAN_POINT ( 'NONE',  ( 121.5722776481213856, -2.395992375830759524, -17.92872468182853396 ) ) ;
#11236 = CARTESIAN_POINT ( 'NONE',  ( 115.9729548109119861, -3.505236298600246325, -18.68346056562440793 ) ) ;
#11237 = VERTEX_POINT ( 'NONE', #36259 ) ;
#11238 = FACE_OUTER_BOUND ( 'NONE', #22988, .T. ) ;
#11239 = DIRECTION ( 'NONE',  ( -0.9659258262890692004, -0.2588190451025175753, -8.979589471384751973E-16 ) ) ;
#11240 = AXIS2_PLACEMENT_3D ( 'NONE', #44294, #41102, #20345 ) ;
#11241 = CARTESIAN_POINT ( 'NONE',  ( 115.8999108795247821, -8.938348069036489818, -9.318865927141430916 ) ) ;
#11242 = CARTESIAN_POINT ( 'NONE',  ( 77.25325688895158294, -4.012910213732562070, -7.993215200338315007 ) ) ;
#11243 = ORIENTED_EDGE ( 'NONE', *, *, #12602, .F. ) ;
#11244 = ORIENTED_EDGE ( 'NONE', *, *, #27590, .F. ) ;
#11245 = CARTESIAN_POINT ( 'NONE',  ( 118.6391081442452986, -5.574606645277164318, -18.38911715685844683 ) ) ;
#11246 = CARTESIAN_POINT ( 'NONE',  ( 118.9794681442453026, -0.8288870151387760510, -10.36305467784173118 ) ) ;
#11247 = CARTESIAN_POINT ( 'NONE',  ( 110.5511732076914200, -2.900984314291613408, -17.25625241347383110 ) ) ;
#11248 = CARTESIAN_POINT ( 'NONE',  ( 123.4244704359119709, 1.345710702986147034, -13.97328579221134426 ) ) ;
#11249 = ORIENTED_EDGE ( 'NONE', *, *, #18431, .T. ) ;
#11250 = CARTESIAN_POINT ( 'NONE',  ( 67.30914723170953096, -60.45752454423683275, -38.28031611818062174 ) ) ;
#11251 = CARTESIAN_POINT ( 'NONE',  ( 125.0480389746927159, -0.4397842399129161528, -7.298781581902527904 ) ) ;
#11252 = CARTESIAN_POINT ( 'NONE',  ( 111.1076452545248259, 0.8980012041604421569, -11.00651665394454071 ) ) ;
#11253 = CARTESIAN_POINT ( 'NONE',  ( 113.3635281442453504, -9.988377603198976828, -10.36322818467138340 ) ) ;
#11254 = CARTESIAN_POINT ( 'NONE',  ( 124.8790414775786246, -8.899110576539710493, -16.42337572283490132 ) ) ;
#11255 =( BOUNDED_CURVE ( )  B_SPLINE_CURVE ( 2, ( #27642, #7315, #10533, #24879, #21235, #14616, #41556, #17376, #31488, #38771, #17594, #7541, #10757 ),
 .UNSPECIFIED., .F., .F. ) 
 B_SPLINE_CURVE_WITH_KNOTS ( ( 3, 2, 2, 2, 2, 2, 3 ),
 ( 0.2742732506792325275, 0.3750000000000000000, 0.5000000000000000000, 0.6250000000000000000, 0.7500000000000000000, 0.8750000000000000000, 1.000000000000000222 ),
 .UNSPECIFIED. ) 
 CURVE ( )  GEOMETRIC_REPRESENTATION_ITEM ( )  RATIONAL_B_SPLINE_CURVE ( ( 0.9761776733140340445, 0.9386610620246780279, 1.000000000000000000, 0.9238795325112869605, 1.000000000000000000, 0.9238795325112869605, 1.000000000000000000, 0.9238795325112869605, 1.000000000000000000, 0.9238795325112869605, 1.000000000000000000, 0.9238795325112869605, 1.000000000000000000 ) ) 
 REPRESENTATION_ITEM ( '' )  );
#11256 = CARTESIAN_POINT ( 'NONE',  ( 116.4267681442453153, -6.222761293078241884, -8.102969835052219238 ) ) ;
#11257 = CARTESIAN_POINT ( 'NONE',  ( -13.56828337869050927, -4.779084862086334873, -8.893215200338314474 ) ) ;
#11258 = ORIENTED_EDGE ( 'NONE', *, *, #5890, .F. ) ;
#11259 = CARTESIAN_POINT ( 'NONE',  ( 118.0151148109119816, 0.4262465694468514643, -12.03445270309931736 ) ) ;
#11260 = VECTOR ( 'NONE', #8043, 1000.000000000000114 ) ;
#11261 = CARTESIAN_POINT ( 'NONE',  ( 115.6915515045247531, -2.477300249445798297, -7.631215200338321125 ) ) ;
#11262 = CARTESIAN_POINT ( 'NONE',  ( 64.43740640915127926, -35.20632691772231482, -5.871463680831255694 ) ) ;
#11263 = LINE ( 'NONE', #4180, #10157 ) ;
#11264 = CARTESIAN_POINT ( 'NONE',  ( 113.9875214775786532, -0.4660016031367893996, -10.09054647747474043 ) ) ;
#11265 = ORIENTED_EDGE ( 'NONE', *, *, #778, .F. ) ;
#11266 = CARTESIAN_POINT ( 'NONE',  ( 115.8027748109119841, -0.4660016031367893996, -10.09054647747474043 ) ) ;
#11267 = CARTESIAN_POINT ( 'NONE',  ( 109.6052378519203927, 0.2518737723193609224, -12.14321520033833757 ) ) ;
#11268 = CARTESIAN_POINT ( 'NONE',  ( 112.7050671295247923, -10.62599879583958540, -13.39321520033831447 ) ) ;
#11269 = CARTESIAN_POINT ( 'NONE',  ( 118.1285681442453068, -7.893985811506177619, -18.51759400769804742 ) ) ;
#11270 = CARTESIAN_POINT ( 'NONE',  ( 113.9875214775786532, -0.4660016031367893996, -10.09054647747474043 ) ) ;
#11271 = LINE ( 'NONE', #8296, #6791 ) ;
#11272 = DIRECTION ( 'NONE',  ( -1.000000000000000000, 0.000000000000000000, 0.000000000000000000 ) ) ;
#11273 = DIRECTION ( 'NONE',  ( -0.1352586133457950590, -0.9908103287288504424, 0.000000000000000000 ) ) ;
#11274 = EDGE_LOOP ( 'NONE', ( #24859, #4803, #32248, #19208, #15271 ) ) ;
#11275 = CARTESIAN_POINT ( 'NONE',  ( 115.8999108795247821, -8.938348069036489818, -9.318865927141430916 ) ) ;
#11276 = CARTESIAN_POINT ( 'NONE',  ( 109.2294308679984596, -7.595023145029839995, -17.96264590402594763 ) ) ;
#11277 = CARTESIAN_POINT ( 'NONE',  ( 116.9940348109119839, -0.1624402480850797581, -16.17319339645315424 ) ) ;
#11278 = EDGE_CURVE ( 'NONE', #2634, #38747, #3882, .T. ) ;
#11279 = CARTESIAN_POINT ( 'NONE',  ( 65.37216319521120056, -13.55122928640068913, -12.15172136135480230 ) ) ;
#11280 = CARTESIAN_POINT ( 'NONE',  ( 117.1500671295247713, 0.1403307496149613920, -13.39321520033831447 ) ) ;
#11281 = CARTESIAN_POINT ( 'NONE',  ( 114.0246765045248196, -2.791137627527939813, -8.388885654883777576 ) ) ;
#11282 = CARTESIAN_POINT ( 'NONE',  ( 121.8310270589982309, -1.063912429576147511, -17.20460841810472985 ) ) ;
#11283 = CARTESIAN_POINT ( 'NONE',  ( 114.2711548109119803, -0.1624402480850797581, -16.17319339645315424 ) ) ;
#11284 = CARTESIAN_POINT ( 'NONE',  ( 120.2274548109119934, -9.859900752359374465, -12.68260735090039404 ) ) ;
#11285 = CARTESIAN_POINT ( 'NONE',  ( 123.1205148109119563, -1.834011780172310813, -8.268836392978581529 ) ) ;
#11286 = CARTESIAN_POINT ( 'NONE',  ( 120.1140014775786398, -1.561330072975668504, -17.79121239304076951 ) ) ;
#11287 = ORIENTED_EDGE ( 'NONE', *, *, #4454, .F. ) ;
#11288 = CARTESIAN_POINT ( 'NONE',  ( 113.7606148109119886, -7.894159318335828068, -9.358103419637847864 ) ) ;
#11289 = CARTESIAN_POINT ( 'NONE',  ( 112.8529881442453302, -1.561330072975668060, -17.79121239304076596 ) ) ;
#11290 = CARTESIAN_POINT ( 'NONE',  ( 118.5823814775786360, -1.834011780172310813, -8.268836392978581529 ) ) ;
#11291 = CARTESIAN_POINT ( 'NONE',  ( 118.0718414775786442, -0.8288870151387760510, -10.36305467784173118 ) ) ;
#11292 = VERTEX_POINT ( 'NONE', #12335 ) ;
#11293 = CARTESIAN_POINT ( 'NONE',  ( 122.7801548109119665, -6.222761293078241884, -8.102969835052219238 ) ) ;
#11294 = CARTESIAN_POINT ( 'NONE',  ( 120.6245414775786458, -9.988377603198976828, -10.36322818467138340 ) ) ;
#11295 = CARTESIAN_POINT ( 'NONE',  ( 137.0728789364823683, 0.5386892458729081179, -13.08566328863867056 ) ) ;
#11296 = CARTESIAN_POINT ( 'NONE',  ( 111.1076452545248259, 0.8980012041604421569, -11.00651665394454071 ) ) ;
#11297 = AXIS2_PLACEMENT_3D ( 'NONE', #45072, #30712, #806 ) ;
#11298 = CARTESIAN_POINT ( 'NONE',  ( 116.0070878430555723, -11.05288298065394059, -20.89321520033831447 ) ) ;
#11299 = CARTESIAN_POINT ( 'NONE',  ( 126.4325107881277575, 0.2402159677550416428, -13.56302502275812039 ) ) ;
#11300 = CARTESIAN_POINT ( 'NONE',  ( 112.0799890045248475, -9.868328341294098749, -11.32035403202665869 ) ) ;
#11301 = CARTESIAN_POINT ( 'NONE',  ( 116.1998614775786507, -10.63000616557722466, -14.87417383870573495 ) ) ;
#11302 = CARTESIAN_POINT ( 'NONE',  ( 135.4522060580572145, -10.81582635000027359, -14.15180293287611413 ) ) ;
#11303 = CARTESIAN_POINT ( 'NONE',  ( 114.1577014775786552, -3.505236298600246325, -18.68346056562440793 ) ) ;
#11304 = DIRECTION ( 'NONE',  ( 0.000000000000000000, -0.3818493186865927203, 0.9242245927363029745 ) ) ;
#11305 = DIRECTION ( 'NONE',  ( -0.000000000000000000, -0.9284778069183721172, -0.3713878862591650232 ) ) ;
#11306 = CARTESIAN_POINT ( 'NONE',  ( 110.2742077545248094, -2.791137627527939813, -18.39754474579286025 ) ) ;
#11307 = CARTESIAN_POINT ( 'NONE',  ( 115.5084538145250406, -3.807985514183278131, -19.09877912889401941 ) ) ;
#11308 = DIRECTION ( 'NONE',  ( 0.000000000000000000, 0.6004852223388323917, -0.7996358532186279566 ) ) ;
#11309 = CARTESIAN_POINT ( 'NONE',  ( 126.2184548109119788, -4.863998795839242995, -13.39321520033831447 ) ) ;
#11311 = CARTESIAN_POINT ( 'NONE',  ( 119.6034614775786196, -6.344957434206665248, -7.627207830600338134 ) ) ;
#11310 = CARTESIAN_POINT ( 'NONE',  ( 64.39952598912073256, -15.22865974175013015, -8.907941765600535078 ) ) ;
#11312 = AXIS2_PLACEMENT_3D ( 'NONE', #19957, #19725, #16084 ) ;
#11313 = CARTESIAN_POINT ( 'NONE',  ( 120.0005481442453146, -4.153390946401325223, -8.397313243818185668 ) ) ;
#11314 = CARTESIAN_POINT ( 'NONE',  ( 126.0703014775786102, -9.988377603198980381, -10.36322818467138518 ) ) ;
#11315 = ORIENTED_EDGE ( 'NONE', *, *, #1112, .F. ) ;
#11316 = CARTESIAN_POINT ( 'NONE',  ( 136.8611794030174735, -7.138509913861316392, -8.324458807404662153 ) ) ;
#11317 = CARTESIAN_POINT ( 'NONE',  ( 123.9146881442452894, 0.9020085738987339008, -11.91225656197089222 ) ) ;
#11318 = CARTESIAN_POINT ( 'NONE',  ( 116.2471765045247594, -2.791137627527939813, -8.388885654883777576 ) ) ;
#11319 = CARTESIAN_POINT ( 'NONE',  ( 117.6180281442453150, -8.899110576539710493, -16.42337572283490132 ) ) ;
#11320 = CARTESIAN_POINT ( 'NONE',  ( 115.2922348109119781, 0.4262465694468514643, -12.03445270309931736 ) ) ;
#11321 = DIRECTION ( 'NONE',  ( -0.8949343913984424415, -0.4123869368673878100, -0.1703803081152053811 ) ) ;
#11322 = CARTESIAN_POINT ( 'NONE',  ( 112.4272546295247821, -4.863998795839590272, -7.631215200338315796 ) ) ;
#11323 = CIRCLE ( 'NONE', #11353, 25.00000000000000355 ) ;
#11324 = CARTESIAN_POINT ( 'NONE',  ( 121.4754414775786131, -1.833838273342659697, -17.42832698103878286 ) ) ;
#11325 = CARTESIAN_POINT ( 'NONE',  ( 125.1059481442452750, -1.833838273342660141, -17.42832698103878286 ) ) ;
#11326 = CARTESIAN_POINT ( 'NONE',  ( 126.2184548109119788, -5.568102603702699049, -18.34339073538272302 ) ) ;
#11327 = CARTESIAN_POINT ( 'NONE',  ( 109.2294421295831768, -1.052844768949616094, -9.585856251807371109 ) ) ;
#11328 = CARTESIAN_POINT ( 'NONE',  ( 120.2296266859119953, -9.033780868592240054, -16.85052413769862056 ) ) ;
#11329 = CARTESIAN_POINT ( 'NONE',  ( 106.6626452545248611, -9.868328341294098749, -15.46607636864997204 ) ) ;
#11330 = CARTESIAN_POINT ( 'NONE',  ( 116.9575464499618676, 1.831790677941273149, -21.12945952840510344 ) ) ;
#11331 = CARTESIAN_POINT ( 'NONE',  ( 83.85919441564438159, -31.77118883039085162, -23.13280229721742742 ) ) ;
#11332 = CARTESIAN_POINT ( 'NONE',  ( 119.2631014775786298, 0.2603800115204892296, -16.42320221600525088 ) ) ;
#11333 = CARTESIAN_POINT ( 'NONE',  ( 118.1852948109119836, -5.638512984488999180, -18.83840828888717311 ) ) ;
#11334 = CARTESIAN_POINT ( 'NONE',  ( 112.0105358795247810, -0.7896495226426338832, -17.46756447353520159 ) ) ;
#11335 = CARTESIAN_POINT ( 'NONE',  ( 114.8384214775786489, 0.9020085738987339008, -11.91225656197089222 ) ) ;
#11336 = ORIENTED_EDGE ( 'NONE', *, *, #6443, .F. ) ;
#11337 = DIRECTION ( 'NONE',  ( 0.000000000000000000, 1.000000000000000000, 0.000000000000000000 ) ) ;
#11338 = VECTOR ( 'NONE', #28335, 1000.000000000000227 ) ;
#11339 = CARTESIAN_POINT ( 'NONE',  ( 115.6893214775786447, 0.5811942927096154232, -14.16772938898807155 ) ) ;
#11340 = CARTESIAN_POINT ( 'NONE',  ( 123.1205148109119563, -7.643976991954077427, -18.09477374809248928 ) ) ;
#11341 = SHAPE_DEFINITION_REPRESENTATION ( #28516, #36667 ) ;
#11342 = CARTESIAN_POINT ( 'NONE',  ( 124.1983214775786166, -8.166667518702819706, -8.995218007635861213 ) ) ;
#11343 = CARTESIAN_POINT ( 'NONE',  ( 123.5176014775786228, -9.261995988541697145, -16.69588392320189030 ) ) ;
#11344 = CARTESIAN_POINT ( 'NONE',  ( 114.0941296295247867, -4.863998795839590272, -19.15521520033831493 ) ) ;
#11345 = CARTESIAN_POINT ( 'NONE',  ( 116.0296814775786345, -1.833838273342658809, -17.42832698103878286 ) ) ;
#11346 = CARTESIAN_POINT ( 'NONE',  ( 120.3685329359119862, -4.283928203966213211, -7.183505701512925334 ) ) ;
#11347 = AXIS2_PLACEMENT_3D ( 'NONE', #29769, #43679, #27036 ) ;
#11348 = DIRECTION ( 'NONE',  ( 0.000000000000000000, 0.000000000000000000, -1.000000000000000000 ) ) ;
#11349 = ORIENTED_EDGE ( 'NONE', *, *, #40755, .F. ) ;
#11350 = B_SPLINE_CURVE_WITH_KNOTS ( 'NONE', 3,
 ( #950, #4364, #281, #39253, #8246, #14868, #38561, #4590, #42908, #28778, #11453, #14414, #21925, #18513, #28109, #8018, #28324, #42236, #11670, #35818, #32404, #24901, #21256, #1174, #14638, #39482, #502, #24674, #31952, #36046 ),
 .UNSPECIFIED., .F., .F.,
 ( 4, 2, 2, 1, 2, 2, 2, 1, 1, 2, 2, 2, 1, 1, 1, 2, 2, 4 ),
 ( 0.000000000000000000, 0.03125000000005303397, 0.06250000000010677570, 0.09375000000016052437, 0.1093750000001824374, 0.1250000000002043643, 0.1875000000002640388, 0.2187500000002932932, 0.2343750000002999823, 0.2421875000003030909, 0.2500000000003061995, 0.3750000000002949307, 0.4375000000002782219, 0.4687500000002805534, 0.4843750000002921552, 0.4921875000002978728, 0.5000000000003035350, 1.000000000000000000 ),
 .UNSPECIFIED. ) ;
#11351 = CARTESIAN_POINT ( 'NONE',  ( 120.3685329359119862, -5.367793381288652910, -18.78638297431638904 ) ) ;
#11352 = CARTESIAN_POINT ( 'NONE',  ( 118.0151148109119816, -10.63000616557722466, -14.87417383870573495 ) ) ;
#11353 = AXIS2_PLACEMENT_3D ( 'NONE', #42655, #25332, #18257 ) ;
#11354 = EDGE_LOOP ( 'NONE', ( #18321, #5491, #39145, #13144, #18243 ) ) ;
#11355 = CARTESIAN_POINT ( 'NONE',  ( 86.34560043013698305, -9.320000780048239619, -8.143215200338314474 ) ) ;
#11356 = CARTESIAN_POINT ( 'NONE',  ( 127.7425183523502881, -7.050714571525749541, -18.72418924296322729 ) ) ;
#11357 = CARTESIAN_POINT ( 'NONE',  ( 70.36267391504962632, -5.685877709920933221, -4.893215200338314474 ) ) ;
#11358 = CARTESIAN_POINT ( 'NONE',  ( 117.5045748109119756, -9.859900752359374465, -12.68260735090039404 ) ) ;
#11359 = ADVANCED_FACE ( 'NONE', ( #26235 ), #25499, .T. ) ;
#11360 = CARTESIAN_POINT ( 'NONE',  ( 77.39250032628930853, -56.65331561251068848, -1.789128725675272369 ) ) ;
#11361 = CARTESIAN_POINT ( 'NONE',  ( 124.5219894712939919, -9.778352389574830994, -12.46904186487667054 ) ) ;
#11362 = CARTESIAN_POINT ( 'NONE',  ( 119.8303681442453126, 0.4262465694468514643, -12.03445270309931736 ) ) ;
#11363 = EDGE_CURVE ( 'NONE', #38132, #3542, #39331, .T. ) ;
#11364 = EDGE_CURVE ( 'NONE', #11150, #16401, #20080, .T. ) ;
#11365 = DIRECTION ( 'NONE',  ( 0.000000000000000000, 0.000000000000000000, -1.000000000000000000 ) ) ;
#11366 = AXIS2_PLACEMENT_3D ( 'NONE', #14047, #27964, #41871 ) ;
#11367 = CARTESIAN_POINT ( 'NONE',  ( 122.1561614775786353, -8.899110576539710493, -16.42337572283490132 ) ) ;
#11368 = VECTOR ( 'NONE', #18467, 1000.000000000000114 ) ;
#11369 = CARTESIAN_POINT ( 'NONE',  ( 121.4544569107182070, -2.467220198592778413, -17.83387418641524391 ) ) ;
#11370 = CARTESIAN_POINT ( 'NONE',  ( 122.3263414775786373, -3.505236298600246325, -18.68346056562440793 ) ) ;
#11371 = CARTESIAN_POINT ( 'NONE',  ( 113.9875214775786532, -0.4660016031367893996, -10.09054647747474043 ) ) ;
#11372 = CARTESIAN_POINT ( 'NONE',  ( 119.0361948109119652, -7.893985811506177619, -18.51759400769804742 ) ) ;
#11373 = CARTESIAN_POINT ( 'NONE',  ( 125.9568481442452850, -3.505236298600246325, -18.68346056562440793 ) ) ;
#11374 = CARTESIAN_POINT ( 'NONE',  ( 88.35093386163799778, -27.84333996136784961, -14.15691383771150136 ) ) ;
#11375 = CARTESIAN_POINT ( 'NONE',  ( 122.2696148109119889, -5.574606645277164318, -18.38911715685844683 ) ) ;
#11376 = ORIENTED_EDGE ( 'NONE', *, *, #33178, .T. ) ;
#11377 = CARTESIAN_POINT ( 'NONE',  ( 121.5321681442453183, -9.988377603198976828, -10.36322818467138340 ) ) ;
#11378 = CARTESIAN_POINT ( 'NONE',  ( 114.5108483795247878, -8.402594152722688392, -16.93181055722141792 ) ) ;
#11379 = CARTESIAN_POINT ( 'NONE',  ( 114.5803015045248259, -6.936859964151197211, -18.39754474579287447 ) ) ;
#11380 = CARTESIAN_POINT ( 'NONE',  ( 122.3826735609119680, -9.645473719204778362, -14.86997237629376123 ) ) ;
#11381 = CARTESIAN_POINT ( 'NONE',  ( 124.8223148109119762, 0.9020085738987339008, -11.91225656197089222 ) ) ;
#11382 = ORIENTED_EDGE ( 'NONE', *, *, #203, .F. ) ;
#11383 = APPLICATION_CONTEXT ( 'automotive_design' ) ;
#11384 = DIRECTION ( 'NONE',  ( -1.000000000000000000, 0.000000000000000000, 0.000000000000000000 ) ) ;
#11385 = CARTESIAN_POINT ( 'NONE',  ( 120.3409081442453044, -8.899110576539710493, -16.42337572283490132 ) ) ;
#11386 = CARTESIAN_POINT ( 'NONE',  ( 121.8270485609119760, -10.36940331770106916, -15.09355782777062061 ) ) ;
#11387 = CARTESIAN_POINT ( 'NONE',  ( 111.6722681442453222, -0.8658195297461032114, -10.39078908864415496 ) ) ;
#11388 = CARTESIAN_POINT ( 'NONE',  ( 107.1488171295248861, 0.1403307496149613920, -13.39321520033831447 ) ) ;
#11389 = EDGE_CURVE ( 'NONE', #42441, #34283, #29135, .T. ) ;
#11390 = AXIS2_PLACEMENT_3D ( 'NONE', #37774, #12947, #38002 ) ;
#11391 = ORIENTED_EDGE ( 'NONE', *, *, #2358, .F. ) ;
#11392 = CARTESIAN_POINT ( 'NONE',  ( 115.2355081442453155, -10.30919188438810075, -12.61870101168855918 ) ) ;
#11393 = CARTESIAN_POINT ( 'NONE',  ( 115.3489614775786407, -9.261995988541697145, -16.69588392320189030 ) ) ;
#11394 = CARTESIAN_POINT ( 'NONE',  ( 79.05243529145373316, 4.793396140045460108, -21.04957699274893557 ) ) ;
#11395 = CARTESIAN_POINT ( 'NONE',  ( 119.8303681442453126, 0.4262465694468514643, -12.03445270309931736 ) ) ;
#11396 = CARTESIAN_POINT ( 'NONE',  ( 126.9932531981140755, -3.096686212419476281, -8.303943172126736272 ) ) ;
#11397 = CARTESIAN_POINT ( 'NONE',  ( 123.9146881442452894, 0.9020085738987339008, -11.91225656197089222 ) ) ;
#11398 = CARTESIAN_POINT ( 'NONE',  ( 111.5482748109120053, -0.1624402480850797581, -16.17319339645315424 ) ) ;
#11399 = COLOUR_RGB ( '',0.7921568627450980005, 0.8196078431372548767, 0.9333333333333333481 ) ;
#11400 = CARTESIAN_POINT ( 'NONE',  ( 69.69189222815028018, -41.76310523276638520, -7.393215200338315363 ) ) ;
#11401 = CARTESIAN_POINT ( 'NONE',  ( 59.90552009294157898, -2.897503654462289191, -8.893215200338314474 ) ) ;
#11402 = EDGE_CURVE ( 'NONE', #42526, #30491, #3398, .T. ) ;
#11403 = CARTESIAN_POINT ( 'NONE',  ( 112.6828081442453282, -7.893985811506177619, -18.51759400769804742 ) ) ;
#11404 = ORIENTED_EDGE ( 'NONE', *, *, #13912, .F. ) ;
#11405 = AXIS2_PLACEMENT_3D ( 'NONE', #1418, #15117, #12376 ) ;
#11406 = EDGE_CURVE ( 'NONE', #14403, #38773, #38590, .T. ) ;
#11407 = CARTESIAN_POINT ( 'NONE',  ( 115.9693640045247776, 0.1403307496149616695, -15.46607636864997204 ) ) ;
#11408 = CARTESIAN_POINT ( 'NONE',  ( 118.9227414775786400, -10.63000616557722466, -14.87417383870573495 ) ) ;
#11409 = CARTESIAN_POINT ( 'NONE',  ( 65.53668513659742700, -0.2719916286899254909, -18.52721583069677180 ) ) ;
#11410 = VERTEX_POINT ( 'NONE', #44257 ) ;
#11411 = CARTESIAN_POINT ( 'NONE',  ( 136.8192643132360615, 0.2368078868278960802, -11.12719817101369379 ) ) ;
#11412 = CARTESIAN_POINT ( 'NONE',  ( 112.6260814775786514, -0.8288870151387760510, -10.36305467784173118 ) ) ;
#11413 = CARTESIAN_POINT ( 'NONE',  ( 105.5513952545248060, 0.8980012041604421569, -11.00651665394454071 ) ) ;
#11414 = CARTESIAN_POINT ( 'NONE',  ( 122.8936081442453059, -9.565557343593413364, -10.61323700422348004 ) ) ;
#11415 = VERTEX_POINT ( 'NONE', #16207 ) ;
#11416 = CARTESIAN_POINT ( 'NONE',  ( 116.9940348109119839, -9.988377603198976828, -10.36322818467138340 ) ) ;
#11417 = PLANE ( 'NONE',  #88 ) ;
#11418 = ADVANCED_FACE ( 'NONE', ( #30109 ), #13241, .T. ) ;
#11419 = CARTESIAN_POINT ( 'NONE',  ( 117.2294421295247844, 0.2335149919452661482, -21.89321520033831447 ) ) ;
#11420 = ADVANCED_FACE ( 'NONE', ( #44706 ), #26213, .T. ) ;
#11421 = EDGE_CURVE ( 'NONE', #37865, #7716, #9491, .T. ) ;
#11422 = CARTESIAN_POINT ( 'NONE',  ( 135.5837700375882946, -5.617920683068854615, -7.449848511264947959 ) ) ;
#11423 = CARTESIAN_POINT ( 'NONE',  ( 124.5386814775786206, -5.638512984488999180, -18.83840828888717311 ) ) ;
#11424 = AXIS2_PLACEMENT_3D ( 'NONE', #9655, #9203, #6230 ) ;
#11425 = DIRECTION ( 'NONE',  ( 1.000000000000000000, 0.000000000000000000, 0.000000000000000000 ) ) ;
#11426 = CARTESIAN_POINT ( 'NONE',  ( 77.77634386988383142, 3.254514819260860392, -21.89321520033831447 ) ) ;
#11427 = CARTESIAN_POINT ( 'NONE',  ( 123.9714148109119805, -0.4660016031367893996, -10.09054647747474043 ) ) ;
#11429 = CARTESIAN_POINT ( 'NONE',  ( 122.1561614775786353, -8.899110576539710493, -16.42337572283490132 ) ) ;
#11428 = CARTESIAN_POINT ( 'NONE',  ( 122.0994348109119443, 0.9020085738987339008, -11.91225656197089222 ) ) ;
#11430 = CARTESIAN_POINT ( 'NONE',  ( 120.9241579359119925, -4.360204210389833968, -8.000047426360245240 ) ) ;
#11431 = CARTESIAN_POINT ( 'NONE',  ( 122.6099748109119929, -0.8288870151387760510, -10.36305467784173118 ) ) ;
#11432 = CARTESIAN_POINT ( 'NONE',  ( 113.7038881442453402, -6.222761293078241884, -8.102969835052219238 ) ) ;
#11433 = CARTESIAN_POINT ( 'NONE',  ( 120.3976348109119812, -1.834011780172310813, -8.268836392978581529 ) ) ;
#11434 = ORIENTED_EDGE ( 'NONE', *, *, #22836, .T. ) ;
#11435 = ORIENTED_EDGE ( 'NONE', *, *, #23104, .F. ) ;
#11436 = CARTESIAN_POINT ( 'NONE',  ( 77.05532149770296257, 0.06670422450934243574, -9.893215200338316251 ) ) ;
#11437 = CARTESIAN_POINT ( 'NONE',  ( 85.45605303719084134, -15.74807682313488222, -9.893215200338316251 ) ) ;
#11438 = CARTESIAN_POINT ( 'NONE',  ( 106.1070202545248407, -10.62599879583958717, -15.77991374673208469 ) ) ;
#11439 = CARTESIAN_POINT ( 'NONE',  ( 111.4549108795247747, -1.325403438956436419, -16.93181055722141792 ) ) ;
#11440 = CARTESIAN_POINT ( 'NONE',  ( 125.4357681442453156, -2.109465145233854422, -8.734689011828928429 ) ) ;
#11441 = CARTESIAN_POINT ( 'NONE',  ( 113.5337081442453240, -9.261995988541697145, -16.69588392320189030 ) ) ;
#11442 = ORIENTED_EDGE ( 'NONE', *, *, #30988, .T. ) ;
#11443 = CARTESIAN_POINT ( 'NONE',  ( 112.1155414775786454, -10.15424416112533912, -14.75197769757731336 ) ) ;
#11444 = CARTESIAN_POINT ( 'NONE',  ( 117.2294421295247844, 1.035107641088057973, -14.64321520033831447 ) ) ;
#11445 = CARTESIAN_POINT ( 'NONE',  ( 119.3765548109119550, -10.15424416112534622, -14.75197769757730448 ) ) ;
#11446 = CARTESIAN_POINT ( 'NONE',  ( 31.16856251326850824, -20.50830283073288385, -8.593215200338315540 ) ) ;
#11447 = LINE ( 'NONE', #16156, #34942 ) ;
#11448 = CARTESIAN_POINT ( 'NONE',  ( 59.75121349346655109, -13.58877957849837692, -19.38162691376808411 ) ) ;
#11449 = CARTESIAN_POINT ( 'NONE',  ( 116.5402214775786405, 0.2603800115204892296, -16.42320221600525088 ) ) ;
#11450 = CARTESIAN_POINT ( 'NONE',  ( 90.33554924625337890, -25.99489077589524300, -13.39321520033831447 ) ) ;
#11451 = CARTESIAN_POINT ( 'NONE',  ( 112.4272546295247821, -4.863998795839590272, -18.39754474579285315 ) ) ;
#11452 = ORIENTED_EDGE ( 'NONE', *, *, #36446, .T. ) ;
#11453 = CARTESIAN_POINT ( 'NONE',  ( 126.3230600034226967, -7.578048725806381114, -9.131528562227654078 ) ) ;
#11454 = CARTESIAN_POINT ( 'NONE',  ( 119.0361948109119652, -2.084020599724406786, -8.691656652584148546 ) ) ;
#11455 = CARTESIAN_POINT ( 'NONE',  ( 115.0086014775786509, -4.089484607189486809, -7.948022111789456723 ) ) ;
#11456 = AXIS2_PLACEMENT_3D ( 'NONE', #16345, #20223, #26832 ) ;
#11457 = CARTESIAN_POINT ( 'NONE',  ( 113.6471614775786492, -5.638512984488999180, -18.83840828888717311 ) ) ;
#11458 = CARTESIAN_POINT ( 'NONE',  ( 124.5954081442453116, -6.222761293078241884, -8.102969835052219238 ) ) ;
#11459 = UNCERTAINTY_MEASURE_WITH_UNIT (LENGTH_MEASURE( 1.000000000000000082E-05 ), #4260, 'distance_accuracy_value', 'NONE');
#11460 = CARTESIAN_POINT ( 'NONE',  ( 119.7736414775786358, 0.1319031606808879209, -14.10382304977623669 ) ) ;
#11461 = CARTESIAN_POINT ( 'NONE',  ( 115.9729548109119861, -3.505236298600246325, -18.68346056562440793 ) ) ;
#11462 = ORIENTED_EDGE ( 'NONE', *, *, #16709, .F. ) ;
#11463 = AXIS2_PLACEMENT_3D ( 'NONE', #19545, #33423, #16128 ) ;
#11464 = CARTESIAN_POINT ( 'NONE',  ( 123.4939235609119663, -9.645473719204776586, -14.86997237629376656 ) ) ;
#11465 = CARTESIAN_POINT ( 'NONE',  ( 113.7722331777918896, -0.01829820670813664396, -14.64321520033831447 ) ) ;
#11466 = CARTESIAN_POINT ( 'NONE',  ( 119.1496481442453046, -6.222761293078241884, -8.102969835052219238 ) ) ;
#11467 = ORIENTED_EDGE ( 'NONE', *, *, #7032, .F. ) ;
#11468 = DIRECTION ( 'NONE',  ( -0.9063289528979890930, -0.4225728684367167087, 0.000000000000000000 ) ) ;
#11469 = EDGE_CURVE ( 'NONE', #1246, #42627, #578, .T. ) ;
#11470 = CARTESIAN_POINT ( 'NONE',  ( 115.8027748109119841, -0.4660016031367893996, -10.09054647747474043 ) ) ;
#11471 = CARTESIAN_POINT ( 'NONE',  ( 108.0517077545248696, -2.791137627527939813, -18.39754474579286025 ) ) ;
#11472 = CARTESIAN_POINT ( 'NONE',  ( 119.2255797424434149, -0.9924539043446216624, -17.29976612834909133 ) ) ;
#11473 = VERTEX_POINT ( 'NONE', #24172 ) ;
#11474 = ORIENTED_EDGE ( 'NONE', *, *, #15835, .T. ) ;
#11475 = CARTESIAN_POINT ( 'NONE',  ( 121.5321681442453183, -0.1624402480850797581, -16.17319339645315424 ) ) ;
#11476 = CARTESIAN_POINT ( 'NONE',  ( 116.0864081442453113, -0.1624402480850797581, -16.17319339645315424 ) ) ;
#11477 = CARTESIAN_POINT ( 'NONE',  ( 124.5359554805749269, -9.835730394904578233, -12.85701071798697015 ) ) ;
#11478 = DIRECTION ( 'NONE',  ( 0.5735764363510499342, 0.3127926500124801890, -0.7570804645221008711 ) ) ;
#11479 = VERTEX_POINT ( 'NONE', #7494 ) ;
#11480 = DIRECTION ( 'NONE',  ( -1.000000000000000000, 0.000000000000000000, 0.000000000000000000 ) ) ;
#11481 = CARTESIAN_POINT ( 'NONE',  ( 124.9063227527172160, -0.2774853123688953982, -7.249199867253821594 ) ) ;
#11482 = CARTESIAN_POINT ( 'NONE',  ( 113.1217858795247935, -0.7896495226426338832, -17.46756447353520159 ) ) ;
#11483 = CARTESIAN_POINT ( 'NONE',  ( 113.8740681442453138, 0.5811942927096154232, -14.16772938898807155 ) ) ;
#11484 = CARTESIAN_POINT ( 'NONE',  ( 111.8886348109120092, -3.383040157471821630, -19.15922257007629170 ) ) ;
#11485 = EDGE_CURVE ( 'NONE', #31092, #13251, #11156, .T. ) ;
#11486 = CARTESIAN_POINT ( 'NONE',  ( 119.6601881442453106, -1.833838273342659253, -17.42832698103878286 ) ) ;
#11487 = CARTESIAN_POINT ( 'NONE',  ( 119.7434548109119703, -12.36944789948969614, -14.53642012792675509 ) ) ;
#11488 = ORIENTED_EDGE ( 'NONE', *, *, #25570, .F. ) ;
#11489 = CARTESIAN_POINT ( 'NONE',  ( 120.6812681442452941, 0.1319031606808879209, -14.10382304977623669 ) ) ;
#11490 = LINE ( 'NONE', #39066, #28432 ) ;
#11491 = CARTESIAN_POINT ( 'NONE',  ( 70.19189222814998175, -50.19222220871606766, -33.27972307567368659 ) ) ;
#11492 = CARTESIAN_POINT ( 'NONE',  ( 115.2748327545248657, -2.477300249445798297, -19.15521520033831138 ) ) ;
#11493 = CARTESIAN_POINT ( 'NONE',  ( 116.7671281442453335, -1.834011780172310813, -8.268836392978581529 ) ) ;
#11494 = ORIENTED_EDGE ( 'NONE', *, *, #38212, .T. ) ;
#11495 = CARTESIAN_POINT ( 'NONE',  ( 117.7314814775786260, -4.089484607189486809, -7.948022111789456723 ) ) ;
#11496 = CARTESIAN_POINT ( 'NONE',  ( 62.29163388691242886, -36.90296252317118331, -5.462008551790970223 ) ) ;
#11497 = CARTESIAN_POINT ( 'NONE',  ( 112.0105358795247810, -0.7896495226426338832, -17.46756447353520159 ) ) ;
#11498 = CARTESIAN_POINT ( 'NONE',  ( 116.5402214775786405, 0.2603800115204892296, -16.42320221600525088 ) ) ;
#11499 = CARTESIAN_POINT ( 'NONE',  ( 118.1852948109119836, -5.638512984488999180, -18.83840828888717311 ) ) ;
#11500 = AXIS2_PLACEMENT_3D ( 'NONE', #13354, #19726, #27483 ) ;
#11501 = CARTESIAN_POINT ( 'NONE',  ( 127.7617783745462816, -10.60212575679465630, -14.01825014569091366 ) ) ;
#11502 = CARTESIAN_POINT ( 'NONE',  ( 111.6869545411902465, -0.3595008806742185925, -10.82052240173743130 ) ) ;
#11503 = CARTESIAN_POINT ( 'NONE',  ( 128.2184548109119930, -1.191816558809784876, -8.648209655763537285 ) ) ;
#11504 = ORIENTED_EDGE ( 'NONE', *, *, #36012, .T. ) ;
#11505 = CARTESIAN_POINT ( 'NONE',  ( 115.5732721536726899, 0.3967854368540359999, -10.50530088663808925 ) ) ;
#11506 = CARTESIAN_POINT ( 'NONE',  ( 109.2295713675052298, -10.43732579977344699, -13.23368918432362484 ) ) ;
#11507 = CARTESIAN_POINT ( 'NONE',  ( 120.1140014775786398, -7.894159318335828068, -9.358103419637847864 ) ) ;
#11508 = DIRECTION ( 'NONE',  ( -1.000000000000000000, 0.000000000000000000, -0.000000000000000000 ) ) ;
#11509 = CARTESIAN_POINT ( 'NONE',  ( 115.8304577545247582, -2.791137627527939813, -18.39754474579286025 ) ) ;
#11510 = CARTESIAN_POINT ( 'NONE',  ( 115.1359265045248605, -2.791137627527939813, -8.388885654883777576 ) ) ;
#11511 = CARTESIAN_POINT ( 'NONE',  ( 126.2184548109108704, -4.273267060618931801, -8.426913831475415506 ) ) ;
#11512 = CARTESIAN_POINT ( 'NONE',  ( 114.7249681442453237, -9.565557343593413364, -10.61323700422348004 ) ) ;
#11513 = CARTESIAN_POINT ( 'NONE',  ( 143.3676850761856940, -49.76310523276723785, -40.89321520033831092 ) ) ;
#11514 = CARTESIAN_POINT ( 'NONE',  ( 124.3685014775786328, -10.63000616557722466, -14.87417383870573495 ) ) ;
#11515 = CARTESIAN_POINT ( 'NONE',  ( 120.6245414775786458, -9.988377603198976828, -10.36322818467138340 ) ) ;
#11516 = ORIENTED_EDGE ( 'NONE', *, *, #37597, .F. ) ;
#11517 = CARTESIAN_POINT ( 'NONE',  ( 117.6180281442453150, -8.899110576539710493, -16.42337572283490132 ) ) ;
#11518 = CARTESIAN_POINT ( 'NONE',  ( 112.3424481442453384, -6.344957434206662583, -7.627207830600332805 ) ) ;
#11519 = CARTESIAN_POINT ( 'NONE',  ( 119.3765548109119834, 0.9020085738987339008, -11.91225656197089222 ) ) ;
#11520 = TOROIDAL_SURFACE ( 'NONE', #36963, 5.500000000000000000, 0.5000000000000000000 ) ;
#11521 = CARTESIAN_POINT ( 'NONE',  ( 121.0783548109119749, -9.565557343593413364, -10.61323700422348004 ) ) ;
#11522 = EDGE_LOOP ( 'NONE', ( #39728, #35352, #42419, #23312 ) ) ;
#11523 = CARTESIAN_POINT ( 'NONE',  ( 125.4463081442452932, -4.153390946401325223, -8.397313243818185668 ) ) ;
#11524 = CARTESIAN_POINT ( 'NONE',  ( 119.1496481442453046, -3.383040157471821630, -19.15922257007629170 ) ) ;
#11525 = CARTESIAN_POINT ( 'NONE',  ( 137.1351618658244433, 0.2097776830087426103, -15.12324877602753048 ) ) ;
#11526 = CARTESIAN_POINT ( 'NONE',  ( 110.8992858795247827, -0.7896495226426338832, -17.46756447353520159 ) ) ;
#11527 = DIRECTION ( 'NONE',  ( 0.000000000000000000, 0.000000000000000000, -1.000000000000000000 ) ) ;
#11528 = DIRECTION ( 'NONE',  ( -0.000000000000000000, -0.9284778069183721172, -0.3713878862591650232 ) ) ;
#11529 = CARTESIAN_POINT ( 'NONE',  ( 114.6497546295247929, -4.863998795839590272, -18.39754474579285315 ) ) ;
#11530 = CARTESIAN_POINT ( 'NONE',  ( 116.9940348109119839, -9.988377603198976828, -10.36322818467138340 ) ) ;
#11531 = ADVANCED_FACE ( 'NONE', ( #3626 ), #21186, .F. ) ;
#11532 = PLANE ( 'NONE',  #4769 ) ;
#11533 = CARTESIAN_POINT ( 'NONE',  ( 114.7816948109119863, -9.859900752359374465, -12.68260735090039404 ) ) ;
#11534 = CARTESIAN_POINT ( 'NONE',  ( 111.7184548109119788, -9.142054238649166109, -15.98131134002176523 ) ) ;
#11535 = DIRECTION ( 'NONE',  ( 0.000000000000000000, 0.000000000000000000, -1.000000000000000000 ) ) ;
#11536 = CARTESIAN_POINT ( 'NONE',  ( 108.6767858795247861, -8.402594152722688392, -9.854619843455216355 ) ) ;
#11537 = LINE ( 'NONE', #31819, #2749 ) ;
#11538 = CARTESIAN_POINT ( 'NONE',  ( 93.24708369096698846, -25.99489077589524300, -13.39321520033831447 ) ) ;
#11539 = CARTESIAN_POINT ( 'NONE',  ( 122.4767535264548854, -8.247323210606174015, -17.08054893949881858 ) ) ;
#11541 = CARTESIAN_POINT ( 'NONE',  ( 119.5467348109119712, -4.089484607189486809, -7.948022111789456723 ) ) ;
#11540 = CARTESIAN_POINT ( 'NONE',  ( 66.12481753886987690, -14.57890275351189402, -10.17775628694920087 ) ) ;
#11542 = CARTESIAN_POINT ( 'NONE',  ( 119.8870948109119752, -0.8288870151387760510, -10.36305467784173118 ) ) ;
#11543 = CARTESIAN_POINT ( 'NONE',  ( 114.2144281442453178, -1.833838273342658809, -17.42832698103878286 ) ) ;
#11544 = EDGE_LOOP ( 'NONE', ( #16285, #11452, #2304, #14563, #16383 ) ) ;
#11545 = CARTESIAN_POINT ( 'NONE',  ( 137.3930029278097891, -7.442204666858849293, -8.961833290247417594 ) ) ;
#11546 = CARTESIAN_POINT ( 'NONE',  ( 124.1415948109119540, -6.344957434206665248, -7.627207830600338134 ) ) ;
#11547 = CARTESIAN_POINT ( 'NONE',  ( 112.7745202545247878, 0.1403307496149616695, -11.32035403202665336 ) ) ;
#11548 = CARTESIAN_POINT ( 'NONE',  ( 119.4900081442453086, -7.643976991954077427, -18.09477374809248928 ) ) ;
#11549 = CARTESIAN_POINT ( 'NONE',  ( 115.5191414775786569, -6.222761293078241884, -8.102969835052219238 ) ) ;
#11550 = CARTESIAN_POINT ( 'NONE',  ( 86.31085725162986932, -26.48153815035164627, -8.422460282204015769 ) ) ;
#11551 = CARTESIAN_POINT ( 'NONE',  ( 109.4407702545248355, -10.62599879583958717, -15.77991374673208469 ) ) ;
#11552 = CARTESIAN_POINT ( 'NONE',  ( 123.8012348109119642, -9.565557343593413364, -10.61323700422348004 ) ) ;
#11553 = CARTESIAN_POINT ( 'NONE',  ( 123.4041481442452834, 0.1319031606808879209, -14.10382304977623669 ) ) ;
#11554 = CARTESIAN_POINT ( 'NONE',  ( 115.0536981469516888, -3.929494816604748753, -18.62311481910882449 ) ) ;
#11555 = CARTESIAN_POINT ( 'NONE',  ( -13.32377113153209791, -5.100909530930220370, -8.593215200338315540 ) ) ;
#11556 = ADVANCED_FACE ( 'NONE', ( #17330 ), #38065, .T. ) ;
#11557 = CARTESIAN_POINT ( 'NONE',  ( 120.5074391859119913, -1.406689858478933353, -17.56299727309130887 ) ) ;
#11558 = CARTESIAN_POINT ( 'NONE',  ( 115.6915515045247531, -2.477300249445798297, -7.631215200338321125 ) ) ;
#11559 = CARTESIAN_POINT ( 'NONE',  ( 116.8677062910727074, 1.935364965237992285, -20.99533717236457164 ) ) ;
#11560 = CARTESIAN_POINT ( 'NONE',  ( 83.96184352754465863, -31.49149003370463262, -22.09312770924474734 ) ) ;
#11561 = CARTESIAN_POINT ( 'NONE',  ( 117.5613014775786525, 0.9020085738987339008, -11.91225656197089222 ) ) ;
#11562 = CARTESIAN_POINT ( 'NONE',  ( 119.5467348109119712, -4.089484607189486809, -7.948022111789456723 ) ) ;
#11563 = CARTESIAN_POINT ( 'NONE',  ( 109.5102233795247884, -8.938348069036489818, -17.46756447353520159 ) ) ;
#11564 = CARTESIAN_POINT ( 'NONE',  ( 112.0588148109119828, 0.5811942927096154232, -14.16772938898807155 ) ) ;
#11565 = EDGE_LOOP ( 'NONE', ( #12650, #23778, #10556, #37976, #28797, #26274 ) ) ;
#11566 = DIRECTION ( 'NONE',  ( -0.2768435750659243300, -0.3568721902840674698, 0.8921882507333136481 ) ) ;
#11567 = CARTESIAN_POINT ( 'NONE',  ( 117.8449348109119938, -8.166667518702817929, -8.995218007635861213 ) ) ;
#11568 = CARTESIAN_POINT ( 'NONE',  ( 120.5678148109119832, -1.833838273342659253, -17.42832698103878286 ) ) ;
#11569 = APPLICATION_PROTOCOL_DEFINITION ( 'draft international standard', 'automotive_design', 1998, #30024 ) ;
#11570 = CARTESIAN_POINT ( 'NONE',  ( 115.5758681442453053, -7.894159318335828068, -9.358103419637847864 ) ) ;
#11571 = CARTESIAN_POINT ( 'NONE',  ( 120.1707281442453166, 0.2603800115204892296, -16.42320221600525088 ) ) ;
#11572 = CARTESIAN_POINT ( 'NONE',  ( 113.8163171295247764, -10.62599879583958540, -13.39321520033831447 ) ) ;
#11573 = CIRCLE ( 'NONE', #35563, 1.999999999999997558 ) ;
#11574 = CARTESIAN_POINT ( 'NONE',  ( 115.5191414775786569, -6.222761293078241884, -8.102969835052219238 ) ) ;
#11575 = CARTESIAN_POINT ( 'NONE',  ( 120.9936110609119737, -3.163656168406935087, -18.89861972220014508 ) ) ;
#11576 = LINE ( 'NONE', #35494, #30850 ) ;
#11577 = ORIENTED_EDGE ( 'NONE', *, *, #30872, .F. ) ;
#11578 = CARTESIAN_POINT ( 'NONE',  ( 122.2437673109119629, 0.2312338769422704887, -16.08380026872395874 ) ) ;
#11579 = CARTESIAN_POINT ( 'NONE',  ( 121.0783548109119749, 0.2603800115204892296, -16.42320221600525088 ) ) ;
#11580 = ORIENTED_EDGE ( 'NONE', *, *, #21934, .F. ) ;
#11581 = CARTESIAN_POINT ( 'NONE',  ( 74.69189222814998175, -41.76310523276723785, -20.39321520033831447 ) ) ;
#11582 = CARTESIAN_POINT ( 'NONE',  ( 64.66798275244620697, -2.679388005794879568, -8.175474704283455907 ) ) ;
#11583 = CARTESIAN_POINT ( 'NONE',  ( 72.87572422742091760, -11.86958442233774313, -21.89321520033831447 ) ) ;
#11584 = CARTESIAN_POINT ( 'NONE',  ( 116.9373081442452929, -1.833838273342659253, -17.42832698103878286 ) ) ;
#11585 = DIRECTION ( 'NONE',  ( 0.000000000000000000, -0.3818493186865927203, 0.9242245927363029745 ) ) ;
#11586 = CARTESIAN_POINT ( 'NONE',  ( 124.0325569858783439, -2.378957183258601393, -17.95140958770220152 ) ) ;
#11587 = CARTESIAN_POINT ( 'NONE',  ( 123.6310548109119765, -4.153390946401325223, -8.397313243818185668 ) ) ;
#11588 = DIRECTION ( 'NONE',  ( 0.000000000000000000, -0.3818493186865927203, 0.9242245927363029745 ) ) ;
#11589 = CARTESIAN_POINT ( 'NONE',  ( 123.2906948109119867, -1.833838273342659697, -17.42832698103878286 ) ) ;
#11590 = CARTESIAN_POINT ( 'NONE',  ( 125.2231329858062594, -11.67996730509178249, -10.73859541710734788 ) ) ;
#11591 = CARTESIAN_POINT ( 'NONE',  ( 123.8579614775786126, -9.859900752359378018, -12.68260735090039759 ) ) ;
#11592 = CARTESIAN_POINT ( 'NONE',  ( 113.0231681442453322, 0.9020085738987339008, -11.91225656197089222 ) ) ;
#11593 = CARTESIAN_POINT ( 'NONE',  ( 120.9081748109119872, -5.638512984488999180, -18.83840828888717311 ) ) ;
#11594 = CARTESIAN_POINT ( 'NONE',  ( 113.5904348109119866, -7.893985811506177619, -18.51759400769804742 ) ) ;
#11595 = DIRECTION ( 'NONE',  ( 0.9609149988134843001, -0.1028163501681632064, 0.2570431154366505933 ) ) ;
#11596 = CARTESIAN_POINT ( 'NONE',  ( 119.8303681442453126, 0.4262465694468514643, -12.03445270309931736 ) ) ;
#11597 = ORIENTED_EDGE ( 'NONE', *, *, #44692, .T. ) ;
#11598 = CARTESIAN_POINT ( 'NONE',  ( 122.2128881442453263, -1.834011780172310813, -8.268836392978581529 ) ) ;
#11599 = CARTESIAN_POINT ( 'NONE',  ( 113.1217858795247935, -8.402594152722688392, -9.854619843455216355 ) ) ;
#11600 = CARTESIAN_POINT ( 'NONE',  ( 82.45431455551781141, -31.76310523276724140, -22.91043087769159214 ) ) ;
#11601 = CARTESIAN_POINT ( 'NONE',  ( 112.6828081442453282, -2.084020599724406786, -8.691656652584148546 ) ) ;
#11602 = CARTESIAN_POINT ( 'NONE',  ( 138.2010754744741519, -3.429981731480040708, -16.55181326108910866 ) ) ;
#11603 = CARTESIAN_POINT ( 'NONE',  ( 116.1777233795247781, -1.325403438956436419, -9.854619843455211026 ) ) ;
#11604 = EDGE_LOOP ( 'NONE', ( #4833, #12764, #33845, #15935 ) ) ;
#11605 = VECTOR ( 'NONE', #37728, 1000.000000000000000 ) ;
#11606 = CARTESIAN_POINT ( 'NONE',  ( 119.8870948109119752, -0.8288870151387760510, -10.36305467784173118 ) ) ;
#11607 = CARTESIAN_POINT ( 'NONE',  ( 119.8823610609119754, -3.163656168406935087, -18.89861972220014508 ) ) ;
#11608 = CARTESIAN_POINT ( 'NONE',  ( 63.13926143489126730, -14.69785589905574241, -17.13608958866837639 ) ) ;
#11609 = PLANE ( 'NONE',  #36258 ) ;
#11610 = CARTESIAN_POINT ( 'NONE',  ( 108.3989733795248753, -1.325403438956436419, -9.854619843455211026 ) ) ;
#11611 = VERTEX_POINT ( 'NONE', #31220 ) ;
#11612 = CARTESIAN_POINT ( 'NONE',  ( 115.4624148109119943, -5.638512984488999180, -18.83840828888717311 ) ) ;
#11613 = CARTESIAN_POINT ( 'NONE',  ( 88.63266681459825236, -11.26170729784157665, -14.03921856447226446 ) ) ;
#11614 = CARTESIAN_POINT ( 'NONE',  ( 120.5110881442453206, -3.505236298600246325, -18.68346056562440793 ) ) ;
#11615 = CARTESIAN_POINT ( 'NONE',  ( 127.3434826498071288, -2.860650813802300352, -8.201060023076600203 ) ) ;
#11616 =( NAMED_UNIT ( * ) PLANE_ANGLE_UNIT ( ) SI_UNIT ( $, .RADIAN. ) );
#11617 = CARTESIAN_POINT ( 'NONE',  ( 111.3213681442453264, -7.643976991954077427, -18.09477374809248928 ) ) ;
#11618 = DIRECTION ( 'NONE',  ( 1.000000000000000000, 0.000000000000000000, 0.000000000000000000 ) ) ;
#11619 = CARTESIAN_POINT ( 'NONE',  ( 61.77615262425602793, -2.025327440714448812, -8.893215200338310922 ) ) ;
#11620 = ORIENTED_EDGE ( 'NONE', *, *, #31449, .F. ) ;
#11621 = EDGE_CURVE ( 'NONE', #12207, #18915, #4368, .T. ) ;
#11622 = CARTESIAN_POINT ( 'NONE',  ( 116.6638952545248031, -9.868328341294098749, -15.46607636864997204 ) ) ;
#11623 = CARTESIAN_POINT ( 'NONE',  ( 121.0783548109119749, 0.2603800115204892296, -16.42320221600525088 ) ) ;
#11624 = CARTESIAN_POINT ( 'NONE',  ( 68.27538871269578635, -1.300937240615723800, -16.26478957841321460 ) ) ;
#11625 = ORIENTED_EDGE ( 'NONE', *, *, #12309, .F. ) ;
#11626 = CARTESIAN_POINT ( 'NONE',  ( 135.3184548109119874, 0.7167481258041168424, -11.18974888642104659 ) ) ;
#11627 = CARTESIAN_POINT ( 'NONE',  ( 112.5126281442453120, 0.1319031606808879209, -14.10382304977623669 ) ) ;
#11628 = CARTESIAN_POINT ( 'NONE',  ( 110.6909265045248247, -2.791137627527939813, -8.388885654883745602 ) ) ;
#11629 = CARTESIAN_POINT ( 'NONE',  ( 121.8158014775786171, -4.153390946401325223, -8.397313243818185668 ) ) ;
#11630 = VERTEX_POINT ( 'NONE', #654 ) ;
#11631 = CARTESIAN_POINT ( 'NONE',  ( 118.0718414775786300, -9.261995988541697145, -16.69588392320189030 ) ) ;
#11632 = CIRCLE ( 'NONE', #37097, 2.999999999999999556 ) ;
#11633 = CARTESIAN_POINT ( 'NONE',  ( 90.04708369096697140, -25.99489077589524300, -13.39321520033831447 ) ) ;
#11634 = CARTESIAN_POINT ( 'NONE',  ( 120.4543614775786295, -4.089484607189480592, -7.948022111789465605 ) ) ;
#11635 = CARTESIAN_POINT ( 'NONE',  ( 64.61650192636965073, -34.86087584742114132, -0.8932152003383146965 ) ) ;
#11636 = CARTESIAN_POINT ( 'NONE',  ( 125.2761281442453054, -10.63000616557722466, -14.87417383870573495 ) ) ;
#11637 = EDGE_CURVE ( 'NONE', #28070, #26037, #18200, .T. ) ;
#11638 = LINE ( 'NONE', #24872, #6578 ) ;
#11639 = VECTOR ( 'NONE', #7170, 1000.000000000000000 ) ;
#11640 = CARTESIAN_POINT ( 'NONE',  ( 123.2184548109119788, -4.863998795839242995, -13.39321520033831447 ) ) ;
#11641 = B_SPLINE_CURVE_WITH_KNOTS ( 'NONE', 3,
 ( #24858, #6642, #31024, #24412, #44955, #24197, #28285, #6864, #31244, #17571, #234, #13928, #27837, #31465, #3873, #38751, #18908, #21661, #25985, #8429, #1352, #18694, #36230, #43311, #11853, #42418, #35779, #25536, #38981, #28514, #25315, #39209, #32363, #1129, #25086, #8203, #36001, #4772, #25760, #15492, #28959, #14595, #4995, #12079, #7749, #39889, #35549, #22112, #39666, #4321, #29173, #29399, #8651, #22334, #18014, #35319 ),
 .UNSPECIFIED., .F., .F.,
 ( 4, 2, 2, 2, 2, 2, 2, 1, 2, 2, 2, 2, 2, 2, 2, 2, 2, 2, 2, 2, 2, 1, 2, 2, 2, 2, 2, 2, 4 ),
 ( 0.000000000000000000, 0.06249999999997815636, 0.09374999999997378486, 0.1093749999999781009, 0.1249999999999824307, 0.1875000000000227873, 0.2187500000000374145, 0.2343750000000390799, 0.2421875000000399125, 0.2500000000000407452, 0.3125000000000284772, 0.3437500000000180966, 0.3593750000000173195, 0.3750000000000165978, 0.5000000000000366374, 0.5625000000000461853, 0.5937500000000491829, 0.6093750000000490719, 0.6250000000000488498, 0.6875000000000446310, 0.7187500000000426326, 0.7343750000000419664, 0.7421875000000414113, 0.7500000000000407452, 0.8125000000000156541, 0.8437500000000029976, 0.8593750000000026645, 0.8750000000000022204, 1.000000000000000000 ),
 .UNSPECIFIED. ) ;
#11642 = CARTESIAN_POINT ( 'NONE',  ( 125.3895814775786448, -7.893985811506177619, -18.51759400769804742 ) ) ;
#11643 = AXIS2_PLACEMENT_3D ( 'NONE', #22958, #33202, #30028 ) ;
#11644 = CARTESIAN_POINT ( 'NONE',  ( 113.2500748109119968, -6.344957434206662583, -7.627207830600332805 ) ) ;
#11645 = CARTESIAN_POINT ( 'NONE',  ( 123.7637130757767352, -0.9924539043446216624, -17.29976612834909133 ) ) ;
#11646 = CARTESIAN_POINT ( 'NONE',  ( 122.0994348109119443, -10.15424416112533912, -14.75197769757731336 ) ) ;
#11647 = CARTESIAN_POINT ( 'NONE',  ( 112.3991748109119868, -1.833838273342658809, -17.42832698103878286 ) ) ;
#11648 = CARTESIAN_POINT ( 'NONE',  ( 119.2063748109119814, -1.561330072975668504, -17.79121239304076951 ) ) ;
#11649 = EDGE_CURVE ( 'NONE', #33082, #9431, #42239, .T. ) ;
#11650 = ORIENTED_EDGE ( 'NONE', *, *, #1993, .F. ) ;
#11651 = CARTESIAN_POINT ( 'NONE',  ( 114.7905291257774820, 0.2334052082820642360, -12.14321520033831625 ) ) ;
#11652 = EDGE_CURVE ( 'NONE', #10767, #42505, #40808, .T. ) ;
#11653 = FACE_OUTER_BOUND ( 'NONE', #18797, .T. ) ;
#11654 = CARTESIAN_POINT ( 'NONE',  ( 115.8999108795247821, -1.325403438956436419, -16.93181055722141792 ) ) ;
#11655 = CARTESIAN_POINT ( 'NONE',  ( 115.2748327545248657, -6.936859964151250502, -8.388885654883777576 ) ) ;
#11656 = CARTESIAN_POINT ( 'NONE',  ( 126.4852516627930612, -9.823310243116877061, -12.06768105343453179 ) ) ;
#11657 = CARTESIAN_POINT ( 'NONE',  ( 115.6325948109119821, 0.2603800115204892296, -16.42320221600525088 ) ) ;
#11658 = ORIENTED_EDGE ( 'NONE', *, *, #18895, .F. ) ;
#11659 = CARTESIAN_POINT ( 'NONE',  ( 116.1431348109119881, 0.1319031606808879209, -14.10382304977623669 ) ) ;
#11660 = DIRECTION ( 'NONE',  ( 0.9609149988134843001, -0.1028163501681632064, 0.2570431154366505933 ) ) ;
#11661 = DIRECTION ( 'NONE',  ( -0.1352586133457954198, -0.9908103287288503314, 0.000000000000000000 ) ) ;
#11662 = CARTESIAN_POINT ( 'NONE',  ( 120.1993349628857146, -6.095137211460705196, -18.44441274085889049 ) ) ;
#11663 = CARTESIAN_POINT ( 'NONE',  ( 70.19189222814998175, -62.26243369865490251, -38.10776559704283528 ) ) ;
#11664 = CARTESIAN_POINT ( 'NONE',  ( 65.91876108126253087, -14.44801200876193370, -16.81557847985648735 ) ) ;
#11665 = CARTESIAN_POINT ( 'NONE',  ( 116.3133148109119759, -7.893985811506177619, -18.51759400769804742 ) ) ;
#11666 = EDGE_CURVE ( 'NONE', #4044, #13839, #36413, .T. ) ;
#11667 = CARTESIAN_POINT ( 'NONE',  ( 110.6214733795247867, -8.938348069036489818, -17.46756447353520159 ) ) ;
#11668 = CARTESIAN_POINT ( 'NONE',  ( 111.7327233795247849, -1.325403438956436419, -9.854619843455211026 ) ) ;
#11669 = ORIENTED_EDGE ( 'NONE', *, *, #12672, .T. ) ;
#11670 = CARTESIAN_POINT ( 'NONE',  ( 126.5621572004118889, -7.381812952428812302, -8.875070251845482261 ) ) ;
#11671 = CARTESIAN_POINT ( 'NONE',  ( 118.9794681442453026, -0.8288870151387760510, -10.36305467784173118 ) ) ;
#11672 = CARTESIAN_POINT ( 'NONE',  ( 116.5969481442453031, 0.5811942927096154232, -14.16772938898807155 ) ) ;
#11673 = CARTESIAN_POINT ( 'NONE',  ( 112.2289948109119848, -1.834011780172310813, -8.268836392978581529 ) ) ;
#11674 = EDGE_CURVE ( 'NONE', #31995, #42647, #8322, .T. ) ;
#11675 = CARTESIAN_POINT ( 'NONE',  ( 124.3685014775786328, 0.4262465694468514643, -12.03445270309931736 ) ) ;
#11676 = CARTESIAN_POINT ( 'NONE',  ( 122.0994348109119443, -10.15424416112533912, -14.75197769757731336 ) ) ;
#11677 = CARTESIAN_POINT ( 'NONE',  ( 115.4056881442453459, -2.084020599724406786, -8.691656652584148546 ) ) ;
#11678 = EDGE_LOOP ( 'NONE', ( #35436, #36749, #42195, #7786 ) ) ;
#11679 = EDGE_CURVE ( 'NONE', #42441, #39438, #4294, .T. ) ;
#11680 = EDGE_CURVE ( 'NONE', #30574, #28223, #36276, .T. ) ;
#11681 = CARTESIAN_POINT ( 'NONE',  ( 119.7434548109119703, -7.554583864224885481, -18.48844787311982785 ) ) ;
#11682 = AXIS2_PLACEMENT_3D ( 'NONE', #8466, #8012, #21919 ) ;
#11683 = DIRECTION ( 'NONE',  ( -1.000000000000000000, 0.000000000000000000, -0.000000000000000000 ) ) ;
#11684 = CARTESIAN_POINT ( 'NONE',  ( 117.7882081442453170, -3.505236298600246325, -18.68346056562440793 ) ) ;
#11685 = ORIENTED_EDGE ( 'NONE', *, *, #3931, .F. ) ;
#11686 = DIRECTION ( 'NONE',  ( 0.000000000000000000, 0.6004852223388321697, -0.7996358532186279566 ) ) ;
#11687 = CARTESIAN_POINT ( 'NONE',  ( 116.5402214775786405, 0.2603800115204892296, -16.42320221600525088 ) ) ;
#11688 = CARTESIAN_POINT ( 'NONE',  ( 106.8015515045248378, -6.936859964151250502, -18.39754474579286025 ) ) ;
#11689 = ORIENTED_EDGE ( 'NONE', *, *, #24861, .F. ) ;
#11690 = ORIENTED_EDGE ( 'NONE', *, *, #39358, .T. ) ;
#11691 = CARTESIAN_POINT ( 'NONE',  ( 123.4608748109119745, 0.4262465694468514643, -12.03445270309931736 ) ) ;
#11692 = CARTESIAN_POINT ( 'NONE',  ( 118.4122014775786340, -9.859900752359374465, -12.68260735090039404 ) ) ;
#11693 = CARTESIAN_POINT ( 'NONE',  ( 124.5623748110993319, -9.860959602566504500, -13.61026352087490565 ) ) ;
#11694 = CARTESIAN_POINT ( 'NONE',  ( 116.4267681442453153, -6.222761293078227673, -8.102969835052210357 ) ) ;
#11695 = VERTEX_POINT ( 'NONE', #43290 ) ;
#11696 = CARTESIAN_POINT ( 'NONE',  ( 110.5266510812576826, -0.01829820670803256055, -12.14321520033831625 ) ) ;
#11697 = CARTESIAN_POINT ( 'NONE',  ( 62.51159666141266058, -64.93666976841245742, -45.57438496592644128 ) ) ;
#11698 = CARTESIAN_POINT ( 'NONE',  ( 109.9963952545248134, 0.8980012041604421569, -11.00651665394454071 ) ) ;
#11699 = AXIS2_PLACEMENT_3D ( 'NONE', #27661, #34033, #13303 ) ;
#11700 = CARTESIAN_POINT ( 'NONE',  ( 115.5191414775786569, -3.383040157471821630, -19.15922257007629170 ) ) ;
#11701 = CARTESIAN_POINT ( 'NONE',  ( 125.5597614775786326, -7.894159318335828068, -9.358103419637847864 ) ) ;
#11702 = CARTESIAN_POINT ( 'NONE',  ( 120.2274548109119934, -9.859900752359378018, -12.68260735090039759 ) ) ;
#11703 = DIRECTION ( 'NONE',  ( 0.9908103287288505534, -0.1352586133457950590, 0.000000000000000000 ) ) ;
#11704 = VERTEX_POINT ( 'NONE', #25289 ) ;
#11705 = CARTESIAN_POINT ( 'NONE',  ( 119.8303681442453126, 0.4262465694468514643, -12.03445270309931736 ) ) ;
#11706 = EDGE_CURVE ( 'NONE', #33236, #27364, #33476, .T. ) ;
#11707 = DIRECTION ( 'NONE',  ( 0.000000000000000000, 0.000000000000000000, 1.000000000000000000 ) ) ;
#11708 = CONICAL_SURFACE ( 'NONE', #1512, 1.499999999999999334, 1.249045772398253540 ) ;
#11709 = CARTESIAN_POINT ( 'NONE',  ( 116.9417077545247992, -2.791137627527939813, -18.39754474579286025 ) ) ;
#11710 = CARTESIAN_POINT ( 'NONE',  ( 116.1082702545247827, -10.62599879583958717, -15.77991374673208469 ) ) ;
#11711 = CARTESIAN_POINT ( 'NONE',  ( 119.7169148109119874, -9.988377603198976828, -10.36322818467138340 ) ) ;
#11712 = ORIENTED_EDGE ( 'NONE', *, *, #31701, .F. ) ;
#11713 = CIRCLE ( 'NONE', #26293, 4.500000000000003553 ) ;
#11714 = CARTESIAN_POINT ( 'NONE',  ( 116.7671281442453335, -1.834011780172310813, -8.268836392978581529 ) ) ;
#11715 = CARTESIAN_POINT ( 'NONE',  ( 115.3367294832010543, -2.324775150319240868, -18.02356106541842351 ) ) ;
#11716 = CARTESIAN_POINT ( 'NONE',  ( 109.3713171295247832, -10.62599879583958540, -13.39321520033831447 ) ) ;
#11717 = CARTESIAN_POINT ( 'NONE',  ( 115.5758681442453053, -1.561330072975668060, -17.79121239304076951 ) ) ;
#11718 = CARTESIAN_POINT ( 'NONE',  ( 118.6958348109119754, -6.344957434206665248, -7.627207830600338134 ) ) ;
#11719 = CARTESIAN_POINT ( 'NONE',  ( 126.3444272079794786, -9.918751065189484351, -13.10290698151034228 ) ) ;
#11720 = CARTESIAN_POINT ( 'NONE',  ( 116.6689336878302043, -11.83255234646479082, -6.347766163431310282 ) ) ;
#11721 = CARTESIAN_POINT ( 'NONE',  ( 106.8015515045248378, -6.936859964151250502, -18.39754474579286025 ) ) ;
#11722 = VERTEX_POINT ( 'NONE', #8632 ) ;
#11723 = CARTESIAN_POINT ( 'NONE',  ( 116.1777233795247781, -8.938348069036489818, -17.46756447353520159 ) ) ;
#11724 = CARTESIAN_POINT ( 'NONE',  ( 109.2294641300314595, -10.43693616051014139, -13.09401194842305038 ) ) ;
#11725 = CARTESIAN_POINT ( 'NONE',  ( 121.8158014775786171, -4.153390946401325223, -8.397313243818185668 ) ) ;
#11726 = CARTESIAN_POINT ( 'NONE',  ( 111.3854577545248645, -2.791137627527939813, -18.39754474579286025 ) ) ;
#11727 = CARTESIAN_POINT ( 'NONE',  ( 106.3153796295248412, -4.863998795839590272, -19.15521520033831493 ) ) ;
#11728 = CARTESIAN_POINT ( 'NONE',  ( 115.7460481442453357, -10.15424416112533912, -14.75197769757731336 ) ) ;
#11729 = DIRECTION ( 'NONE',  ( 0.9908103287288504424, -0.1352586133457950313, 0.000000000000000000 ) ) ;
#11730 = CARTESIAN_POINT ( 'NONE',  ( 124.7655881442452852, 0.5811942927096110934, -14.16772938898807510 ) ) ;
#11731 = B_SPLINE_CURVE_WITH_KNOTS ( 'NONE', 3,
 ( #17097, #17318, #44689, #10694 ),
 .UNSPECIFIED., .F., .F.,
 ( 4, 4 ),
 ( 0.0003857850822298949651, 0.001092701553673899872 ),
 .UNSPECIFIED. ) ;
#11732 = CARTESIAN_POINT ( 'NONE',  ( 118.9227414775786400, -10.63000616557722466, -14.87417383870573495 ) ) ;
#11733 = ORIENTED_EDGE ( 'NONE', *, *, #3745, .T. ) ;
#11734 = EDGE_CURVE ( 'NONE', #22330, #24453, #30576, .T. ) ;
#11735 = CARTESIAN_POINT ( 'NONE',  ( 118.1852948109119836, -4.153390946401325223, -8.397313243818185668 ) ) ;
#11736 = CARTESIAN_POINT ( 'NONE',  ( 113.0798948109119948, -0.4660016031367893996, -10.09054647747474043 ) ) ;
#11737 = VECTOR ( 'NONE', #29599, 1000.000000000000000 ) ;
#11738 = CARTESIAN_POINT ( 'NONE',  ( 120.1707281442453166, 0.2603800115204892296, -16.42320221600525088 ) ) ;
#11739 = CARTESIAN_POINT ( 'NONE',  ( 119.8870948109119752, -0.8288870151387760510, -10.36305467784173118 ) ) ;
#11740 = ORIENTED_EDGE ( 'NONE', *, *, #19812, .T. ) ;
#11741 = EDGE_CURVE ( 'NONE', #10810, #35134, #8182, .T. ) ;
#11742 = CARTESIAN_POINT ( 'NONE',  ( 124.9924948109119924, -5.574606645277164318, -18.38911715685844683 ) ) ;
#11743 = PRODUCT_RELATED_PRODUCT_CATEGORY ( 'part', '', ( #14299 ) ) ;
#11744 = AXIS2_PLACEMENT_3D ( 'NONE', #29721, #1453, #19011 ) ;
#11745 = CARTESIAN_POINT ( 'NONE',  ( 121.1350814775786233, 0.5811942927096110934, -14.16772938898807510 ) ) ;
#11746 = CARTESIAN_POINT ( 'NONE',  ( 125.1589444732324807, -6.145249445731414184, -6.105551253155266700 ) ) ;
#11747 = AXIS2_PLACEMENT_3D ( 'NONE', #34529, #24297, #31121 ) ;
#11748 = DIRECTION ( 'NONE',  ( -1.000000000000000000, 0.000000000000000000, 0.000000000000000000 ) ) ;
#11749 = FACE_OUTER_BOUND ( 'NONE', #40486, .T. ) ;
#11750 = CARTESIAN_POINT ( 'NONE',  ( 114.0246765045248196, -2.791137627527939813, -8.388885654883777576 ) ) ;
#11751 = CARTESIAN_POINT ( 'NONE',  ( 73.47343079648352671, -1.934511955536642791, -12.14321520033831625 ) ) ;
#11752 = CARTESIAN_POINT ( 'NONE',  ( 116.7104014775786425, -8.899110576539710493, -16.42337572283490132 ) ) ;
#11753 = CARTESIAN_POINT ( 'NONE',  ( 124.7655881442452852, 0.5811942927096110934, -14.16772938898807510 ) ) ;
#11754 = CARTESIAN_POINT ( 'NONE',  ( 64.98755411081816646, -13.32594127658043170, -15.07288939246319970 ) ) ;
#11755 = CARTESIAN_POINT ( 'NONE',  ( 117.8239502440515452, -2.467220198592778413, -17.83387418641524391 ) ) ;
#11756 = CARTESIAN_POINT ( 'NONE',  ( 109.1629577545248395, -2.791137627527939813, -18.39754474579286025 ) ) ;
#11757 = CARTESIAN_POINT ( 'NONE',  ( 115.3489614775786407, -9.261995988541700697, -16.69588392320188319 ) ) ;
#11758 = DIRECTION ( 'NONE',  ( 0.000000000000000000, -0.3818493186865929978, 0.9242245927363029745 ) ) ;
#11759 = CARTESIAN_POINT ( 'NONE',  ( -1.637506834317598026, -6.775152287193681566, -17.89321520033831447 ) ) ;
#11761 = CARTESIAN_POINT ( 'NONE',  ( 120.9081748109119872, -5.638512984488999180, -18.83840828888717311 ) ) ;
#11760 = CARTESIAN_POINT ( 'NONE',  ( 59.75121349346654398, -13.58877957849836093, -7.404803486908547505 ) ) ;
#11762 = CARTESIAN_POINT ( 'NONE',  ( 122.6099748109119929, -0.8288870151387760510, -10.36305467784173118 ) ) ;
#11763 = ORIENTED_EDGE ( 'NONE', *, *, #16387, .T. ) ;
#11764 = DIRECTION ( 'NONE',  ( 0.9609149988134837450, -0.1028163501681639419, 0.2570431154366518145 ) ) ;
#11765 = CARTESIAN_POINT ( 'NONE',  ( 125.5597614775786326, -1.561330072975669392, -17.79121239304076951 ) ) ;
#11766 = B_SPLINE_CURVE_WITH_KNOTS ( 'NONE', 3,
 ( #4866, #40207, #36317, #26073, #32889, #1664, #1442, #5087, #15139, #8740, #36095, #11949, #32674, #15365, #29269, #12400, #29713, #43184, #5536, #26300, #2110, #25846, #16038, #39977, #33118, #15588, #11720, #1225, #19453, #29946, #19003, #29491, #22648, #12171, #39536 ),
 .UNSPECIFIED., .F., .F.,
 ( 4, 2, 2, 1, 1, 2, 2, 2, 2, 1, 1, 2, 2, 2, 2, 1, 1, 1, 2, 2, 4 ),
 ( 0.000000000000000000, 0.1249999999999536482, 0.1874999999999301670, 0.2187499999999181211, 0.2343749999999113487, 0.2421874999999079625, 0.2499999999999046041, 0.3749999999998828160, 0.4374999999998722688, 0.4687499999998676059, 0.4843749999998684386, 0.4921874999998683831, 0.4999999999998683275, 0.6249999999999567013, 0.6875000000000006661, 0.7187500000000220934, 0.7343750000000325295, 0.7421875000000374145, 0.7460937500000398570, 0.7500000000000422995, 1.000000000000000000 ),
 .UNSPECIFIED. ) ;
#11767 = CARTESIAN_POINT ( 'NONE',  ( 110.8992858795247827, -8.402594152722688392, -9.854619843455216355 ) ) ;
#11768 = CARTESIAN_POINT ( 'NONE',  ( 118.2987481442453088, -7.894159318335828068, -9.358103419637847864 ) ) ;
#11769 = EDGE_CURVE ( 'NONE', #40139, #30207, #4367, .T. ) ;
#11770 = CARTESIAN_POINT ( 'NONE',  ( 120.0572748109119772, -6.222761293078241884, -8.102969835052219238 ) ) ;
#11771 = CARTESIAN_POINT ( 'NONE',  ( 114.9518748109119883, -7.643976991954077427, -18.09477374809248928 ) ) ;
#11772 = CARTESIAN_POINT ( 'NONE',  ( 73.07463722459043254, -61.07442264524582498, -36.73805742556071152 ) ) ;
#11773 = CARTESIAN_POINT ( 'NONE',  ( 107.5655358795247736, -0.7896495226426338832, -17.46756447353520159 ) ) ;
#11774 = CARTESIAN_POINT ( 'NONE',  ( 123.6310548109119765, -4.153390946401325223, -8.397313243818185668 ) ) ;
#11775 = AXIS2_PLACEMENT_3D ( 'NONE', #20245, #9986, #45083 ) ;
#11776 = CARTESIAN_POINT ( 'NONE',  ( 124.9357681442453014, -7.643976991954077427, -18.09477374809248928 ) ) ;
#11777 = CARTESIAN_POINT ( 'NONE',  ( 108.7294421295247844, -9.051693226400931991, -21.39321520033831447 ) ) ;
#11778 = DIRECTION ( 'NONE',  ( 1.000000000000000000, 0.000000000000000000, 0.000000000000000000 ) ) ;
#11779 = CARTESIAN_POINT ( 'NONE',  ( 120.3685329359119862, -5.367793381288652910, -18.78638297431638904 ) ) ;
#11780 = CARTESIAN_POINT ( 'NONE',  ( 113.7468640045248236, -10.62599879583958717, -11.00651665394454604 ) ) ;
#11781 = CARTESIAN_POINT ( 'NONE',  ( -13.15471766443228141, -4.070564271056700711, -19.15902936687194469 ) ) ;
#11782 = CARTESIAN_POINT ( 'NONE',  ( 83.87387534288872359, -31.73118616881930620, -23.27653720400033066 ) ) ;
#11783 = CARTESIAN_POINT ( 'NONE',  ( 120.6812681442452941, -10.30919188438810075, -12.61870101168855918 ) ) ;
#11784 = CARTESIAN_POINT ( 'NONE',  ( 119.7169148109119874, -9.988377603198976828, -10.36322818467138340 ) ) ;
#11785 = CARTESIAN_POINT ( 'NONE',  ( 106.6626452545248611, 0.8980012041604421569, -11.00651665394454071 ) ) ;
#11786 = FACE_OUTER_BOUND ( 'NONE', #36950, .T. ) ;
#11787 = DIRECTION ( 'NONE',  ( -1.000000000000000000, 0.000000000000000000, 0.000000000000000000 ) ) ;
#11788 = VERTEX_POINT ( 'NONE', #32111 ) ;
#11789 = DIRECTION ( 'NONE',  ( -0.9908103287288504424, 0.1352586133457951423, 0.000000000000000000 ) ) ;
#11790 = CARTESIAN_POINT ( 'NONE',  ( 115.9162281442453235, -4.089484607189486809, -7.948022111789456723 ) ) ;
#11791 = EDGE_CURVE ( 'NONE', #35800, #29125, #21845, .T. ) ;
#11792 = CARTESIAN_POINT ( 'NONE',  ( 124.5386814775786206, -4.153390946401325223, -8.397313243818185668 ) ) ;
#11793 = DIRECTION ( 'NONE',  ( 0.000000000000000000, 0.000000000000000000, 1.000000000000000000 ) ) ;
#11794 = CARTESIAN_POINT ( 'NONE',  ( 114.4413348109119823, -0.8288870151387760510, -10.36305467784173118 ) ) ;
#11795 = CARTESIAN_POINT ( 'NONE',  ( 122.7801548109119665, -3.383040157471821630, -19.15922257007629170 ) ) ;
#11796 = CARTESIAN_POINT ( 'NONE',  ( 112.4272546295247821, -4.863998795839590272, -7.631215200338315796 ) ) ;
#11797 = VECTOR ( 'NONE', #37643, 1000.000000000000000 ) ;
#11798 = CARTESIAN_POINT ( 'NONE',  ( 118.2420214775786320, -6.222761293078241884, -8.102969835052219238 ) ) ;
#11799 = DIRECTION ( 'NONE',  ( -1.000000000000000000, 0.000000000000000000, 0.000000000000000000 ) ) ;
#11800 = CARTESIAN_POINT ( 'NONE',  ( 123.6797710478795835, -5.999872392221376138, -18.26400721298383800 ) ) ;
#11801 = ORIENTED_EDGE ( 'NONE', *, *, #23916, .T. ) ;
#11802 = CARTESIAN_POINT ( 'NONE',  ( 120.9241579359119925, -4.360204210389833968, -8.000047426360245240 ) ) ;
#11803 = CARTESIAN_POINT ( 'NONE',  ( 120.0005481442453146, -5.638512984488999180, -18.83840828888717311 ) ) ;
#11804 = ORIENTED_EDGE ( 'NONE', *, *, #25317, .F. ) ;
#11805 = CARTESIAN_POINT ( 'NONE',  ( 66.31928500851137187, -14.71576354012722021, -10.39321520033831625 ) ) ;
#11806 = AXIS2_PLACEMENT_3D ( 'NONE', #13691, #7497, #24614 ) ;
#11807 = CARTESIAN_POINT ( 'NONE',  ( -13.15712544184149202, -4.069566355151700066, -7.629049492614480954 ) ) ;
#11808 = DIRECTION ( 'NONE',  ( 0.9609149988134837450, -0.1028163501681639419, 0.2570431154366518145 ) ) ;
#11809 = CARTESIAN_POINT ( 'NONE',  ( 119.8303681442453126, 0.4262465694468514643, -12.03445270309931736 ) ) ;
#11810 = CARTESIAN_POINT ( 'NONE',  ( 65.10287265247757205, -0.4742552606671820992, -16.39321520033831447 ) ) ;
#11811 = CARTESIAN_POINT ( 'NONE',  ( 64.21004395737219284, -35.06008033345069919, -5.893215200338315363 ) ) ;
#11812 = CARTESIAN_POINT ( 'NONE',  ( 123.3474214775786209, -0.1624402480850797581, -16.17319339645315424 ) ) ;
#11813 = CARTESIAN_POINT ( 'NONE',  ( 125.7866681442453256, -8.899110576539104756, -16.42337572283570424 ) ) ;
#11814 = CARTESIAN_POINT ( 'NONE',  ( 125.5597614775786326, -7.894159318335828068, -9.358103419637847864 ) ) ;
#11815 = CARTESIAN_POINT ( 'NONE',  ( 125.3417925815060698, -11.53121377071529530, -15.77642740804299493 ) ) ;
#11816 = CARTESIAN_POINT ( 'NONE',  ( 116.1998614775786507, 0.4262465694468514643, -12.03445270309931736 ) ) ;
#11817 = CARTESIAN_POINT ( 'NONE',  ( 122.0994348109119443, -10.15424416112533912, -14.75197769757731336 ) ) ;
#11818 = CARTESIAN_POINT ( 'NONE',  ( 114.4980614775786592, -7.893985811506177619, -18.51759400769804742 ) ) ;
#11819 = CARTESIAN_POINT ( 'NONE',  ( 119.2631014775786298, 0.2603800115204892296, -16.42320221600525088 ) ) ;
#11820 = CARTESIAN_POINT ( 'NONE',  ( 114.7249681442453237, 0.2603800115204892296, -16.42320221600525088 ) ) ;
#11821 = LINE ( 'NONE', #28927, #10352 ) ;
#11822 = CARTESIAN_POINT ( 'NONE',  ( 125.2194014775786286, 0.1319031606808879209, -14.10382304977623669 ) ) ;
#11823 = ORIENTED_EDGE ( 'NONE', *, *, #11485, .T. ) ;
#11825 = CARTESIAN_POINT ( 'NONE',  ( 119.0361948109119652, -7.893985811506177619, -18.51759400769804742 ) ) ;
#11824 = AXIS2_PLACEMENT_3D ( 'NONE', #16268, #29712, #26299 ) ;
#11826 = CARTESIAN_POINT ( 'NONE',  ( 115.7610046295247912, -4.863998795839590272, -7.631215200338315796 ) ) ;
#11827 = CARTESIAN_POINT ( 'NONE',  ( 114.2330358795247776, -8.402594152722688392, -9.854619843455216355 ) ) ;
#11828 = FACE_OUTER_BOUND ( 'NONE', #34630, .T. ) ;
#11829 = FACE_OUTER_BOUND ( 'NONE', #28203, .T. ) ;
#11830 = AXIS2_PLACEMENT_3D ( 'NONE', #30159, #1872, #27195 ) ;
#11831 = DIRECTION ( 'NONE',  ( 1.000000000000000000, 0.000000000000000000, -0.000000000000000000 ) ) ;
#11832 = CARTESIAN_POINT ( 'NONE',  ( 126.0135748109119902, -8.166667518702819706, -8.995218007635861213 ) ) ;
#11833 = ORIENTED_EDGE ( 'NONE', *, *, #26449, .T. ) ;
#11834 = CARTESIAN_POINT ( 'NONE',  ( 122.4397948109119767, -0.1624402480850797581, -16.17319339645315424 ) ) ;
#11835 = CARTESIAN_POINT ( 'NONE',  ( 120.4379860609119675, -6.564341423271550902, -7.887810678476487425 ) ) ;
#11836 = CARTESIAN_POINT ( 'NONE',  ( 121.6186891859119896, -8.844754642576884152, -8.592115655440050404 ) ) ;
#11837 = CARTESIAN_POINT ( 'NONE',  ( 124.1497896737536877, -8.611453504372539314, -17.77011218421760574 ) ) ;
#11838 = CARTESIAN_POINT ( 'NONE',  ( 107.4960827545248350, -6.936859964151250502, -8.388885654883777576 ) ) ;
#11839 = VERTEX_POINT ( 'NONE', #35755 ) ;
#11840 = CIRCLE ( 'NONE', #175, 3.000000000000003997 ) ;
#11841 = CARTESIAN_POINT ( 'NONE',  ( 113.6471614775786492, -5.638512984488999180, -18.83840828888717311 ) ) ;
#11842 = CARTESIAN_POINT ( 'NONE',  ( 126.1837548109119211, -10.63000616557722466, -14.87417383870573495 ) ) ;
#11843 = CARTESIAN_POINT ( 'NONE',  ( 119.3765548109119834, -10.15424416112533912, -14.75197769757731336 ) ) ;
#11844 = EDGE_CURVE ( 'NONE', #2582, #29158, #40974, .T. ) ;
#11845 = CARTESIAN_POINT ( 'NONE',  ( 126.4852516627927912, -3.538464648936350265, -8.433903753060587150 ) ) ;
#11846 =( NAMED_UNIT ( * ) SI_UNIT ( $, .STERADIAN. ) SOLID_ANGLE_UNIT ( ) );
#11847 = DIRECTION ( 'NONE',  ( 0.8636456077245086016, -0.5040994586965593660, 0.000000000000000000 ) ) ;
#11848 = DIRECTION ( 'NONE',  ( 1.000000000000000000, 0.000000000000000000, 0.000000000000000000 ) ) ;
#11849 = CARTESIAN_POINT ( 'NONE',  ( 125.0492214775786266, -3.505236298600246325, -18.68346056562440793 ) ) ;
#11850 = VERTEX_POINT ( 'NONE', #5197 ) ;
#11851 = DIRECTION ( 'NONE',  ( 0.1352586133457954198, 0.9908103287288503314, 0.000000000000000000 ) ) ;
#11852 = CARTESIAN_POINT ( 'NONE',  ( 121.3619881442452879, -4.089484607189486809, -7.948022111789456723 ) ) ;
#11853 = CARTESIAN_POINT ( 'NONE',  ( 137.2865145795265391, -8.514350784173746689, -17.13881612151974210 ) ) ;
#11854 = ORIENTED_EDGE ( 'NONE', *, *, #3829, .T. ) ;
#11855 = CARTESIAN_POINT ( 'NONE',  ( 115.5758681442453053, -1.561330072975668060, -17.79121239304076951 ) ) ;
#11856 = CARTESIAN_POINT ( 'NONE',  ( 111.5482748109120053, -0.1624402480850797581, -16.17319339645315424 ) ) ;
#11857 = AXIS2_PLACEMENT_3D ( 'NONE', #28055, #20545, #3431 ) ;
#11858 = CARTESIAN_POINT ( 'NONE',  ( 70.19189222814998175, -51.48119552555760947, -33.79530790927901052 ) ) ;
#11859 = CARTESIAN_POINT ( 'NONE',  ( 121.7590748109119687, -2.084020599724406786, -8.691656652584148546 ) ) ;
#11860 = ORIENTED_EDGE ( 'NONE', *, *, #25420, .T. ) ;
#11861 = CIRCLE ( 'NONE', #27166, 1.200000000000000178 ) ;
#11862 = CARTESIAN_POINT ( 'NONE',  ( 117.5613014775786525, 0.9020085738987339008, -11.91225656197089222 ) ) ;
#11863 = DIRECTION ( 'NONE',  ( 1.000000000000000000, 0.000000000000000000, 0.000000000000000000 ) ) ;
#11864 = DIRECTION ( 'NONE',  ( 0.000000000000000000, 0.3818493186865929423, -0.9242245927363028635 ) ) ;
#11865 = CARTESIAN_POINT ( 'NONE',  ( 115.2035566399283795, 0.4261359969231631739, -14.64321520033831447 ) ) ;
#11866 = PRESENTATION_LAYER_ASSIGNMENT (  '', '', ( #35147 ) ) ;
#11867 = CARTESIAN_POINT ( 'NONE',  ( 136.7082020370459077, -5.390462347091045103, -7.772095544634614050 ) ) ;
#11868 = CARTESIAN_POINT ( 'NONE',  ( 113.5904348109119866, -2.084020599724406786, -8.691656652584148546 ) ) ;
#11869 = CARTESIAN_POINT ( 'NONE',  ( 94.20708369096698220, -26.70704619373760735, -14.24467064448769982 ) ) ;
#11870 = CIRCLE ( 'NONE', #30815, 6.479565957685756494 ) ;
#11871 = CARTESIAN_POINT ( 'NONE',  ( 124.7803599147174367, -3.802325732078021492, -21.07728963076554862 ) ) ;
#11872 = CARTESIAN_POINT ( 'NONE',  ( 125.6732148109119862, 0.5811942927096110934, -14.16772938898807510 ) ) ;
#11873 = CARTESIAN_POINT ( 'NONE',  ( 113.0231681442453322, 0.9020085738987339008, -11.91225656197089222 ) ) ;
#11874 = CARTESIAN_POINT ( 'NONE',  ( 120.5768923109119868, -0.4387604401700512802, -15.73000352943951619 ) ) ;
#11875 = CARTESIAN_POINT ( 'NONE',  ( 123.9714148109119805, -8.899110576539710493, -16.42337572283490132 ) ) ;
#11876 = CARTESIAN_POINT ( 'NONE',  ( 112.2289948109119848, -7.643976991954077427, -18.09477374809248928 ) ) ;
#11877 = CARTESIAN_POINT ( 'NONE',  ( 119.2631014775786298, 0.2603800115204892296, -16.42320221600525088 ) ) ;
#11878 = ORIENTED_EDGE ( 'NONE', *, *, #2319, .F. ) ;
#11879 = CARTESIAN_POINT ( 'NONE',  ( 95.28169473643895060, -24.52346489965341902, -16.95464091111045590 ) ) ;
#11880 = CARTESIAN_POINT ( 'NONE',  ( 115.8304577545247582, -7.250697342233347165, -7.631215200338321125 ) ) ;
#11881 = CARTESIAN_POINT ( 'NONE',  ( 108.9545983795247821, -8.402594152722688392, -16.93181055722141792 ) ) ;
#11882 = CARTESIAN_POINT ( 'NONE',  ( 109.7880358795247986, -8.402594152722688392, -9.854619843455216355 ) ) ;
#11883 = CARTESIAN_POINT ( 'NONE',  ( 126.5621572004067872, -9.839173191191122214, -11.97876773276561302 ) ) ;
#11884 = CARTESIAN_POINT ( 'NONE',  ( 113.8173414775786512, 0.2603800115204892296, -16.42320221600525088 ) ) ;
#11885 = ORIENTED_EDGE ( 'NONE', *, *, #40181, .F. ) ;
#11886 = CARTESIAN_POINT ( 'NONE',  ( 116.4267681442453153, -6.222761293078241884, -8.102969835052219238 ) ) ;
#11887 = CARTESIAN_POINT ( 'NONE',  ( 107.9822546295247889, -4.863998795839590272, -7.631215200338315796 ) ) ;
#11888 = CYLINDRICAL_SURFACE ( 'NONE', #41643, 15.90000000000000036 ) ;
#11889 = CARTESIAN_POINT ( 'NONE',  ( 111.2647102085435193, -8.897589485953298905, -16.42540022429002633 ) ) ;
#11890 = CARTESIAN_POINT ( 'NONE',  ( 119.7692287164846476, -6.356880537135879194, -18.94008305455118801 ) ) ;
#11891 = CARTESIAN_POINT ( 'NONE',  ( 112.2857214775786474, -4.089484607189486809, -7.948022111789456723 ) ) ;
#11892 = CARTESIAN_POINT ( 'NONE',  ( 120.5678148109119832, -8.166667518702819706, -8.995218007635861213 ) ) ;
#11893 = CARTESIAN_POINT ( 'NONE',  ( 112.2883483795247770, -0.7896495226426338832, -9.318865927141430916 ) ) ;
#11894 = CARTESIAN_POINT ( 'NONE',  ( 111.9410827545248708, -6.936859964151250502, -8.388885654883777576 ) ) ;
#11895 = ORIENTED_EDGE ( 'NONE', *, *, #23080, .F. ) ;
#11896 = CARTESIAN_POINT ( 'NONE',  ( 80.91184012100937650, -3.933054092416038650, -19.39321520033831447 ) ) ;
#11897 = CARTESIAN_POINT ( 'NONE',  ( 118.7525614775786380, -1.833838273342659253, -17.42832698103878286 ) ) ;
#11898 = VECTOR ( 'NONE', #41685, 1000.000000000000000 ) ;
#11899 = CARTESIAN_POINT ( 'NONE',  ( 117.0507614775786465, -10.30919188438810075, -12.61870101168855918 ) ) ;
#11900 = DIRECTION ( 'NONE',  ( 0.9908103287288504424, -0.1352586133457950590, 0.000000000000000000 ) ) ;
#11901 = CARTESIAN_POINT ( 'NONE',  ( 118.1852948109119836, -4.153390946401313677, -8.397313243818183892 ) ) ;
#11902 = CARTESIAN_POINT ( 'NONE',  ( 124.5954081442453116, -6.222761293078241884, -8.102969835052219238 ) ) ;
#11903 = CARTESIAN_POINT ( 'NONE',  ( 116.4267681442453153, -6.222761293078241884, -8.102969835052219238 ) ) ;
#11904 = VERTEX_POINT ( 'NONE', #19116 ) ;
#11905 = EDGE_CURVE ( 'NONE', #16801, #30998, #5977, .T. ) ;
#11906 = CARTESIAN_POINT ( 'NONE',  ( 124.2579079359120016, -4.360204210389833968, -8.000047426360245240 ) ) ;
#11907 = VECTOR ( 'NONE', #1302, 999.9999999999998863 ) ;
#11908 = CARTESIAN_POINT ( 'NONE',  ( 121.5330010407382133, -2.419733177069661512, -17.89711025544711376 ) ) ;
#11909 = CARTESIAN_POINT ( 'NONE',  ( 117.4478481442453131, -9.565557343593413364, -10.61323700422348004 ) ) ;
#11910 = ORIENTED_EDGE ( 'NONE', *, *, #15956, .T. ) ;
#11911 = PLANE ( 'NONE',  #7801 ) ;
#11912 = CARTESIAN_POINT ( 'NONE',  ( 113.6471614775786492, -5.638512984488999180, -18.83840828888717311 ) ) ;
#11913 = ADVANCED_FACE ( 'NONE', ( #16609 ), #13417, .T. ) ;
#11914 = CARTESIAN_POINT ( 'NONE',  ( 108.1211608795247798, -1.325403438956436419, -16.93181055722141792 ) ) ;
#11915 = CARTESIAN_POINT ( 'NONE',  ( 119.1081470589982274, -1.063912429576147511, -17.20460841810472985 ) ) ;
#11916 = ORIENTED_EDGE ( 'NONE', *, *, #16356, .T. ) ;
#11917 = EDGE_LOOP ( 'NONE', ( #4535, #38810, #25970, #4118, #14545, #43036 ) ) ;
#11918 = CARTESIAN_POINT ( 'NONE',  ( 122.8368814775786291, -7.894159318335828068, -9.358103419637847864 ) ) ;
#11919 = CARTESIAN_POINT ( 'NONE',  ( 116.0296814775786345, -1.833838273342658809, -17.42832698103878286 ) ) ;
#11920 =( BOUNDED_CURVE ( )  B_SPLINE_CURVE ( 2, ( #43121, #40553, #18507, #14862, #30060, #5033, #35812, #39701, #12737, #32397, #23222, #5876, #42678, #8240, #4808, #32622, #15083 ),
 .UNSPECIFIED., .F., .F. ) 
 B_SPLINE_CURVE_WITH_KNOTS ( ( 3, 2, 2, 2, 2, 2, 2, 2, 3 ),
 ( 0.7671282416568590001, 0.7734375000000000000, 0.7812500000000000000, 0.7890625000000000000, 0.7968750000000000000, 0.8046875000000000000, 0.8125000000000000000, 0.8203125000000000000, 0.8266217583431409999 ),
 .UNSPECIFIED. ) 
 CURVE ( )  GEOMETRIC_REPRESENTATION_ITEM ( )  RATIONAL_B_SPLINE_CURVE ( ( 0.9763430640195950305, 0.9385262470928690259, 1.000000000000000000, 0.9238795325112869605, 1.000000000000000000, 0.9238795325112869605, 1.000000000000000000, 0.9238795325112869605, 1.000000000000000000, 0.9238795325112869605, 1.000000000000000000, 0.9238795325112869605, 1.000000000000000000, 0.9238795325112869605, 1.000000000000000000, 0.9385262470928680267, 0.9763430640195970289 ) ) 
 REPRESENTATION_ITEM ( '' )  );
#11921 = VERTEX_POINT ( 'NONE', #44203 ) ;
#11922 = CARTESIAN_POINT ( 'NONE',  ( 112.1657300207295549, -8.916287984722918836, -16.39106325734287850 ) ) ;
#11923 = CARTESIAN_POINT ( 'NONE',  ( 61.80744621386338622, -65.84115252037693722, -43.66573742411122083 ) ) ;
#11924 = CARTESIAN_POINT ( 'NONE',  ( 110.5520202545248054, -10.62599879583958717, -15.77991374673208469 ) ) ;
#11925 = AXIS2_PLACEMENT_3D ( 'NONE', #42679, #42902, #10773 ) ;
#11926 = CARTESIAN_POINT ( 'NONE',  ( 117.9583881442453048, -10.30919188438810075, -12.61870101168855918 ) ) ;
#11927 = EDGE_CURVE ( 'NONE', #17, #36181, #30502, .T. ) ;
#11929 = CARTESIAN_POINT ( 'NONE',  ( 117.4478481442453131, -9.565557343593413364, -10.61323700422348004 ) ) ;
#11928 = CARTESIAN_POINT ( 'NONE',  ( 116.0296814775786345, -8.166667518702817929, -8.995218007635861213 ) ) ;
#11930 = CARTESIAN_POINT ( 'NONE',  ( 120.5678148109119832, -1.833838273342659253, -17.42832698103878286 ) ) ;
#11931 = FACE_OUTER_BOUND ( 'NONE', #37187, .T. ) ;
#11932 = EDGE_CURVE ( 'NONE', #39770, #11206, #44453, .T. ) ;
#11933 = EDGE_CURVE ( 'NONE', #39210, #12514, #14555, .T. ) ;
#11934 = VERTEX_POINT ( 'NONE', #6105 ) ;
#11935 = CARTESIAN_POINT ( 'NONE',  ( 118.7525614775786380, -1.833838273342659253, -17.42832698103878286 ) ) ;
#11936 = CARTESIAN_POINT ( 'NONE',  ( 123.9714148109119805, -8.899110576539710493, -16.42337572283490132 ) ) ;
#11937 = CARTESIAN_POINT ( 'NONE',  ( 111.9410827545248708, -2.477300249445798297, -19.15521520033831138 ) ) ;
#11938 = AXIS2_PLACEMENT_3D ( 'NONE', #11982, #32924, #1258 ) ;
#11939 = CARTESIAN_POINT ( 'NONE',  ( 116.5249890045247980, -9.868328341294098749, -11.32035403202665869 ) ) ;
#11940 = CARTESIAN_POINT ( 'NONE',  ( 111.2465515045248168, -2.477300249445798297, -7.631215200338321125 ) ) ;
#11941 = CARTESIAN_POINT ( 'NONE',  ( 119.0361948109119652, -7.893985811506177619, -18.51759400769804742 ) ) ;
#11942 = VERTEX_POINT ( 'NONE', #43970 ) ;
#11943 = CARTESIAN_POINT ( 'NONE',  ( 121.3052614775786111, -1.834011780172310813, -8.268836392978581529 ) ) ;
#11944 = CARTESIAN_POINT ( 'NONE',  ( 62.50008149197554275, -37.25231330516801620, -5.285959774307153580 ) ) ;
#11945 = CARTESIAN_POINT ( 'NONE',  ( 108.1906140045248463, -10.62599879583958717, -11.00651665394454604 ) ) ;
#11946 = CARTESIAN_POINT ( 'NONE',  ( 117.7314814775786260, -4.089484607189486809, -7.948022111789456723 ) ) ;
#11947 = CARTESIAN_POINT ( 'NONE',  ( 119.2631014775786298, 0.2603800115204892296, -16.42320221600525088 ) ) ;
#11948 = CARTESIAN_POINT ( 'NONE',  ( 125.5030348109119558, -6.222761293078241884, -8.102969835052219238 ) ) ;
#11949 = CARTESIAN_POINT ( 'NONE',  ( 117.1139656878117563, -11.30305607403721879, -5.600395450087082949 ) ) ;
#11950 = ORIENTED_EDGE ( 'NONE', *, *, #5000, .T. ) ;
#11951 = LINE ( 'NONE', #32005, #42695 ) ;
#11952 = CARTESIAN_POINT ( 'NONE',  ( 109.2294401191927165, -10.32848583145956844, -14.25478553988458685 ) ) ;
#11953 = CARTESIAN_POINT ( 'NONE',  ( 119.0929214775786278, -4.153390946401325223, -8.397313243818185668 ) ) ;
#11954 = CARTESIAN_POINT ( 'NONE',  ( 113.0523327545247838, -6.936859964151250502, -8.388885654883777576 ) ) ;
#11955 = CARTESIAN_POINT ( 'NONE',  ( 115.8999108795247821, -1.325403438956436419, -16.93181055722141792 ) ) ;
#11956 = CARTESIAN_POINT ( 'NONE',  ( 112.6828081442453282, -2.084020599724406786, -8.691656652584148546 ) ) ;
#11957 = CARTESIAN_POINT ( 'NONE',  ( 61.63318325272354770, -19.46990085680238636, -16.39321520033831447 ) ) ;
#11958 = CARTESIAN_POINT ( 'NONE',  ( 69.81869296892593013, -25.88089094749368613, -5.787280954910575481 ) ) ;
#11959 = CARTESIAN_POINT ( 'NONE',  ( 112.9097148109120070, -9.565557343593413364, -10.61323700422348004 ) ) ;
#11960 = CARTESIAN_POINT ( 'NONE',  ( 120.9649014775786355, -3.383040157471821630, -19.15922257007629170 ) ) ;
#11961 = ORIENTED_EDGE ( 'NONE', *, *, #20393, .F. ) ;
#11962 = EDGE_CURVE ( 'NONE', #32179, #41326, #22753, .T. ) ;
#11963 = CARTESIAN_POINT ( 'NONE',  ( 118.8092881442453290, -0.1624402480850797581, -16.17319339645315424 ) ) ;
#11964 = CARTESIAN_POINT ( 'NONE',  ( 114.1577014775786552, -6.344957434206662583, -7.627207830600332805 ) ) ;
#11965 = CARTESIAN_POINT ( 'NONE',  ( 123.0070614775786169, 0.9020085738987339008, -11.91225656197089222 ) ) ;
#11966 = CARTESIAN_POINT ( 'NONE',  ( 118.9227414775786542, 0.4262465694468514643, -12.03445270309931736 ) ) ;
#11967 = VERTEX_POINT ( 'NONE', #40776 ) ;
#11968 = CARTESIAN_POINT ( 'NONE',  ( 116.2678702882355140, -1.135392229370332462, -17.10942237759954665 ) ) ;
#11969 = EDGE_CURVE ( 'NONE', #19575, #12207, #9799, .T. ) ;
#11970 = EDGE_CURVE ( 'NONE', #38354, #14378, #37334, .T. ) ;
#11971 = CARTESIAN_POINT ( 'NONE',  ( 119.0361948109119652, -7.893985811506177619, -18.51759400769804742 ) ) ;
#11972 = CARTESIAN_POINT ( 'NONE',  ( 123.9584548109119737, -5.853704621469987934, -5.454671103420249523 ) ) ;
#11973 = CARTESIAN_POINT ( 'NONE',  ( 121.9292548109119849, -1.561330072975668948, -17.79121239304076951 ) ) ;
#11974 = CARTESIAN_POINT ( 'NONE',  ( 70.19189222814998175, -52.61716011954800365, -34.24968978710501943 ) ) ;
#11975 = CARTESIAN_POINT ( 'NONE',  ( 118.7708473908105873, -2.443475742715334853, -17.86549347949429389 ) ) ;
#11976 = VECTOR ( 'NONE', #36808, 1000.000000000000000 ) ;
#11977 = CARTESIAN_POINT ( 'NONE',  ( 113.7468640045248236, 0.1403307496149616695, -15.46607636864997204 ) ) ;
#11978 = CARTESIAN_POINT ( 'NONE',  ( 123.4244704359119709, -10.25716656981731489, -12.88942061488890545 ) ) ;
#11979 = CARTESIAN_POINT ( 'NONE',  ( 137.5082292857753430, -9.854187482169276535, -12.96399892178506263 ) ) ;
#11980 = CARTESIAN_POINT ( 'NONE',  ( 115.4624148109119943, -4.153390946401321671, -8.397313243818183892 ) ) ;
#11981 = CARTESIAN_POINT ( 'NONE',  ( 124.9924948109119924, -4.089484607189486809, -7.948022111789456723 ) ) ;
#11982 = CARTESIAN_POINT ( 'NONE',  ( 117.2294421295247844, -4.863998795839590272, -13.39321520033831447 ) ) ;
#11983 = ADVANCED_FACE ( 'NONE', ( #23678 ), #13881, .T. ) ;
#11984 = FACE_OUTER_BOUND ( 'NONE', #19609, .T. ) ;
#11985 = CARTESIAN_POINT ( 'NONE',  ( 112.6356140045247827, 0.1403307496149616695, -15.46607636864997204 ) ) ;
#11986 = CARTESIAN_POINT ( 'NONE',  ( 116.9373081442452929, -1.833838273342659253, -17.42832698103878286 ) ) ;
#11987 = DIRECTION ( 'NONE',  ( 0.000000000000000000, 0.9242245927363005320, 0.3818493186865984379 ) ) ;
#11988 = CARTESIAN_POINT ( 'NONE',  ( -1.996248100948082360, -6.883391001766379524, -18.88506229808600523 ) ) ;
#11990 = CARTESIAN_POINT ( 'NONE',  ( 120.9649014775786355, -3.383040157471821630, -19.15922257007629170 ) ) ;
#11989 = CARTESIAN_POINT ( 'NONE',  ( 61.96962176546384882, -13.30635342911269881, -7.742800864598132549 ) ) ;
#11991 = CARTESIAN_POINT ( 'NONE',  ( 121.8158014775786171, -4.153390946401325223, -8.397313243818185668 ) ) ;
#11992 = EDGE_LOOP ( 'NONE', ( #2881, #1461, #20339, #34702, #31543, #7825, #40094, #12369, #37061, #19538, #15018, #25291, #39262, #8591, #14216, #17624, #13425, #8245, #34653, #16234, #32883, #12028, #23987 ) ) ;
#11993 = LINE ( 'NONE', #16316, #21692 ) ;
#11994 = CARTESIAN_POINT ( 'NONE',  ( 125.1059481442452750, -8.166667518702819706, -8.995218007635861213 ) ) ;
#11995 = CARTESIAN_POINT ( 'NONE',  ( 109.8574890045247940, -9.868328341294098749, -11.32035403202665869 ) ) ;
#11996 = CARTESIAN_POINT ( 'NONE',  ( 122.3263414775786373, -3.505236298600246325, -18.68346056562440793 ) ) ;
#11997 = CARTESIAN_POINT ( 'NONE',  ( 121.8158014775786171, -4.153390946401325223, -8.397313243818185668 ) ) ;
#11998 = CARTESIAN_POINT ( 'NONE',  ( 116.8238548109119819, -5.574606645277164318, -18.38911715685844683 ) ) ;
#11999 = CARTESIAN_POINT ( 'NONE',  ( 124.7472578386058615, 1.330726760588684332, -18.10008909799004329 ) ) ;
#12000 = CARTESIAN_POINT ( 'NONE',  ( 109.9963952545248134, 0.8980012041604421569, -11.00651665394454071 ) ) ;
#12001 = CARTESIAN_POINT ( 'NONE',  ( 123.7445081442452874, -7.894159318335828068, -9.358103419637847864 ) ) ;
#12002 = CARTESIAN_POINT ( 'NONE',  ( 123.2339681442453241, -3.505236298600246325, -18.68346056562440793 ) ) ;
#12003 = CARTESIAN_POINT ( 'NONE',  ( 61.76986277844709861, -39.32091226840162079, -4.893215200338314474 ) ) ;
#12004 = CARTESIAN_POINT ( 'NONE',  ( 112.7962614775786676, -6.222761293078232114, -8.102969835052212133 ) ) ;
#12005 = CARTESIAN_POINT ( 'NONE',  ( 120.6463454359119822, 0.5291689781388270175, -13.89700978578772705 ) ) ;
#12006 = CARTESIAN_POINT ( 'NONE',  ( 114.8581140045248361, -10.62599879583958717, -11.00651665394454604 ) ) ;
#12007 =( BOUNDED_SURFACE ( )  B_SPLINE_SURFACE ( 1, 2, ( 
 ( #990, #28816, #18549, #11709, #15352, #25619, #22189, #1654, #18774, #11939, #32663, #29480, #25835, #1431, #29259, #43170, #39742, #36307, #5075, #18992, #43393, #12160, #5308, #13064, #2557, #20358, #23094, #27425, #9875, #2789, #10103, #23317, #5523, #19443, #9188, #33326, #30161, #2100, #34244, #6213, #37203, #16027, #29935, #27198, #3017, #16939, #2330, #23785, #16486, #9407, #30834, #44757, #26963, #36976, #43849, #16260, #16716, #41346, #9638, #44080, #12618, #5744, #13516, #37674, #36755, #40884, #20134, #30609, #6450, #26519, #44309, #40428, #13290, #30386, #19664, #34020, #33552, #23560, #12844, #26745, #37441, #41116, #40652, #5975, #44527, #19901, #33786, #18042, #43059, #7320, #21241, #17164, #24007, #38330, #10762, #13957, #44981, #703, #24886, #3464, #13739, #485, #35118, #20799, #28090, #14398, #6889, #7550, #38779, #27648, #7106, #34890, #3679, #31270, #31937, #15237, #29146, #17381, #17600, #38115, #35348, #3901, #31052, #31493, #37894, #17819, #264, #41562, #10322, #4123, #24225, #34679, #6673, #14173, #43, #21016, #24659, #41999, #38545, #21465, #27868, #20580, #42221, #31716, #34459, #10537, #3238, #41782, #24439, #28309, #10982, #22308, #9305, #26404, #1546, #26631, #1769, #23213, #36870, #5193, #40544 ),
 ( #22528, #43738, #18881, #8628, #22981, #39863, #2217, #5866, #30273, #40314, #9078, #4971, #11826, #26179, #12508, #15695, #32772, #33672, #12728, #36424, #15467, #33438, #5640, #19111, #15925, #16147, #32995, #37092, #19788, #29373, #40087, #22748, #36649, #29597, #2450, #16370, #25733, #43514, #5422, #25956, #39640, #19561, #43284, #19339, #8404, #30051, #33224, #12055, #12283, #36204, #8848, #1999, #29822, #43964, #44417, #16832, #6556, #27313, #30725, #6787, #2672, #31168, #41452, #3134, #13845, #20248, #12960, #26856, #33902, #40769, #41007, #9527, #20696, #20473, #6099, #38012, #37562, #34574, #17057, #9760, #3358, #13410, #23443, #44873, #6331, #37328, #20019, #44198, #37783, #13183, #27086, #45089, #16604, #30497, #34354, #23672, #17276, #10210, #34134, #2903, #44648, #30949, #13629, #24118, #41231, #9991, #23900, #27540, #5112, #26096, #37242, #26783, #30424, #43885, #9226, #33591, #40691, #19937, #2134, #16525, #16297, #19481, #8766, #23135, #15610, #33362, #19261, #9444, #5561, #30197, #29517, #9000, #29738, #6013, #22897, #37013, #22672, #23357, #5783, #44116, #16064, #12656, #29970, #44343, #13102, #36568, #1913, #1691, #26552, #40465, #19703, #43649, #40233, #12883, #36340, #26326, #19028, #36792, #12425, #39777, #32914 ) ),
 .UNSPECIFIED., .F., .F., .T. ) 
 B_SPLINE_SURFACE_WITH_KNOTS ( ( 2, 2 ),
 ( 3, 2, 2, 2, 2, 2, 2, 2, 2, 2, 2, 2, 2, 2, 2, 2, 2, 2, 2, 2, 2, 2, 2, 2, 2, 2, 2, 2, 2, 2, 2, 2, 2, 2, 2, 2, 2, 2, 2, 2, 2, 2, 2, 2, 2, 2, 2, 2, 2, 2, 2, 2, 2, 2, 2, 2, 2, 2, 2, 2, 2, 2, 2, 2, 2, 2, 2, 2, 2, 2, 2, 2, 2, 2, 2, 2, 2, 2, 2, 2, 3 ),
 ( 0.000000000000000000, 1.000000000000000000 ),
 ( 0.000000000000000000, 0.01250000000000000069, 0.02500000000000000139, 0.03749999999999999861, 0.05000000000000000278, 0.06250000000000000000, 0.07499999999999999722, 0.08749999999999999445, 0.1000000000000000056, 0.1125000000000000028, 0.1250000000000000000, 0.1375000000000000111, 0.1499999999999999944, 0.1625000000000000056, 0.1749999999999999889, 0.1875000000000000000, 0.2000000000000000111, 0.2124999999999999944, 0.2250000000000000056, 0.2374999999999999889, 0.2500000000000000000, 0.2625000000000000111, 0.2750000000000000222, 0.2874999999999999778, 0.2999999999999999889, 0.3125000000000000000, 0.3250000000000000111, 0.3375000000000000222, 0.3499999999999999778, 0.3624999999999999889, 0.3750000000000000000, 0.3875000000000000111, 0.4000000000000000222, 0.4124999999999999778, 0.4249999999999999889, 0.4375000000000000000, 0.4500000000000000111, 0.4625000000000000222, 0.4749999999999999778, 0.4874999999999999889, 0.5000000000000000000, 0.5124999999999999556, 0.5250000000000000222, 0.5374999999999999778, 0.5500000000000000444, 0.5625000000000000000, 0.5749999999999999556, 0.5875000000000000222, 0.5999999999999999778, 0.6125000000000000444, 0.6250000000000000000, 0.6374999999999999556, 0.6500000000000000222, 0.6624999999999999778, 0.6750000000000000444, 0.6875000000000000000, 0.6999999999999999556, 0.7125000000000000222, 0.7249999999999999778, 0.7375000000000000444, 0.7500000000000000000, 0.7624999999999999556, 0.7750000000000000222, 0.7874999999999999778, 0.8000000000000000444, 0.8125000000000000000, 0.8249999999999999556, 0.8375000000000000222, 0.8499999999999999778, 0.8625000000000000444, 0.8750000000000000000, 0.8874999999999999556, 0.9000000000000000222, 0.9124999999999999778, 0.9250000000000000444, 0.9375000000000000000, 0.9499999999999999556, 0.9625000000000000222, 0.9749999999999999778, 0.9875000000000000444, 1.000000000000000000 ),
 .UNSPECIFIED. ) 
 GEOMETRIC_REPRESENTATION_ITEM ( )  RATIONAL_B_SPLINE_SURFACE ( (
 ( 1.000000000000000000, 0.9238795325112869605, 1.000000000000000000, 0.9238795325112869605, 1.000000000000000000, 0.9238795325112869605, 1.000000000000000000, 0.9238795325112869605, 1.000000000000000000, 0.9238795325112869605, 1.000000000000000000, 0.9238795325112869605, 1.000000000000000000, 0.9238795325112869605, 1.000000000000000000, 0.9238795325112869605, 1.000000000000000000, 0.9238795325112869605, 1.000000000000000000, 0.9238795325112869605, 1.000000000000000000, 0.9238795325112869605, 1.000000000000000000, 0.9238795325112869605, 1.000000000000000000, 0.9238795325112869605, 1.000000000000000000, 0.9238795325112869605, 1.000000000000000000, 0.9238795325112869605, 1.000000000000000000, 0.9238795325112869605, 1.000000000000000000, 0.9238795325112869605, 1.000000000000000000, 0.9238795325112869605, 1.000000000000000000, 0.9238795325112869605, 1.000000000000000000, 0.9238795325112869605, 1.000000000000000000, 0.9238795325112869605, 1.000000000000000000, 0.9238795325112869605, 1.000000000000000000, 0.9238795325112869605, 1.000000000000000000, 0.9238795325112869605, 1.000000000000000000, 0.9238795325112869605, 1.000000000000000000, 0.9238795325112869605, 1.000000000000000000, 0.9238795325112869605, 1.000000000000000000, 0.9238795325112869605, 1.000000000000000000, 0.9238795325112869605, 1.000000000000000000, 0.9238795325112869605, 1.000000000000000000, 0.9238795325112869605, 1.000000000000000000, 0.9238795325112869605, 1.000000000000000000, 0.9238795325112869605, 1.000000000000000000, 0.9238795325112869605, 1.000000000000000000, 0.9238795325112869605, 1.000000000000000000, 0.9238795325112869605, 1.000000000000000000, 0.9238795325112869605, 1.000000000000000000, 0.9238795325112869605, 1.000000000000000000, 0.9238795325112869605, 1.000000000000000000, 0.9238795325112869605, 1.000000000000000000, 0.9238795325112869605, 1.000000000000000000, 0.9238795325112869605, 1.000000000000000000, 0.9238795325112869605, 1.000000000000000000, 0.9238795325112869605, 1.000000000000000000, 0.9238795325112869605, 1.000000000000000000, 0.9238795325112869605, 1.000000000000000000, 0.9238795325112869605, 1.000000000000000000, 0.9238795325112869605, 1.000000000000000000, 0.9238795325112869605, 1.000000000000000000, 0.9238795325112869605, 1.000000000000000000, 0.9238795325112869605, 1.000000000000000000, 0.9238795325112869605, 1.000000000000000000, 0.9238795325112869605, 1.000000000000000000, 0.9238795325112869605, 1.000000000000000000, 0.9238795325112869605, 1.000000000000000000, 0.9238795325112869605, 1.000000000000000000, 0.9238795325112869605, 1.000000000000000000, 0.9238795325112869605, 1.000000000000000000, 0.9238795325112869605, 1.000000000000000000, 0.9238795325112869605, 1.000000000000000000, 0.9238795325112869605, 1.000000000000000000, 0.9238795325112869605, 1.000000000000000000, 0.9238795325112869605, 1.000000000000000000, 0.9238795325112869605, 1.000000000000000000, 0.9238795325112869605, 1.000000000000000000, 0.9238795325112869605, 1.000000000000000000, 0.9238795325112869605, 1.000000000000000000, 0.9238795325112869605, 1.000000000000000000, 0.9238795325112869605, 1.000000000000000000, 0.9238795325112869605, 1.000000000000000000, 0.9238795325112869605, 1.000000000000000000, 0.9238795325112869605, 1.000000000000000000, 0.9238795325112869605, 1.000000000000000000, 0.9238795325112869605, 1.000000000000000000, 0.9238795325112869605, 1.000000000000000000, 0.9238795325112869605, 1.000000000000000000, 0.9238795325112869605, 1.000000000000000000, 0.9238795325112869605, 1.000000000000000000, 0.9238795325112869605, 1.000000000000000000, 0.9238795325112869605, 1.000000000000000000),
 ( 1.000000000000000000, 0.9238795325112869605, 1.000000000000000000, 0.9238795325112869605, 1.000000000000000000, 0.9238795325112869605, 1.000000000000000000, 0.9238795325112869605, 1.000000000000000000, 0.9238795325112869605, 1.000000000000000000, 0.9238795325112869605, 1.000000000000000000, 0.9238795325112869605, 1.000000000000000000, 0.9238795325112869605, 1.000000000000000000, 0.9238795325112869605, 1.000000000000000000, 0.9238795325112869605, 1.000000000000000000, 0.9238795325112869605, 1.000000000000000000, 0.9238795325112869605, 1.000000000000000000, 0.9238795325112869605, 1.000000000000000000, 0.9238795325112869605, 1.000000000000000000, 0.9238795325112869605, 1.000000000000000000, 0.9238795325112869605, 1.000000000000000000, 0.9238795325112869605, 1.000000000000000000, 0.9238795325112869605, 1.000000000000000000, 0.9238795325112869605, 1.000000000000000000, 0.9238795325112869605, 1.000000000000000000, 0.9238795325112869605, 1.000000000000000000, 0.9238795325112869605, 1.000000000000000000, 0.9238795325112869605, 1.000000000000000000, 0.9238795325112869605, 1.000000000000000000, 0.9238795325112869605, 1.000000000000000000, 0.9238795325112869605, 1.000000000000000000, 0.9238795325112869605, 1.000000000000000000, 0.9238795325112869605, 1.000000000000000000, 0.9238795325112869605, 1.000000000000000000, 0.9238795325112869605, 1.000000000000000000, 0.9238795325112869605, 1.000000000000000000, 0.9238795325112869605, 1.000000000000000000, 0.9238795325112869605, 1.000000000000000000, 0.9238795325112869605, 1.000000000000000000, 0.9238795325112869605, 1.000000000000000000, 0.9238795325112869605, 1.000000000000000000, 0.9238795325112869605, 1.000000000000000000, 0.9238795325112869605, 1.000000000000000000, 0.9238795325112869605, 1.000000000000000000, 0.9238795325112869605, 1.000000000000000000, 0.9238795325112869605, 1.000000000000000000, 0.9238795325112869605, 1.000000000000000000, 0.9238795325112869605, 1.000000000000000000, 0.9238795325112869605, 1.000000000000000000, 0.9238795325112869605, 1.000000000000000000, 0.9238795325112869605, 1.000000000000000000, 0.9238795325112869605, 1.000000000000000000, 0.9238795325112869605, 1.000000000000000000, 0.9238795325112869605, 1.000000000000000000, 0.9238795325112869605, 1.000000000000000000, 0.9238795325112869605, 1.000000000000000000, 0.9238795325112869605, 1.000000000000000000, 0.9238795325112869605, 1.000000000000000000, 0.9238795325112869605, 1.000000000000000000, 0.9238795325112869605, 1.000000000000000000, 0.9238795325112869605, 1.000000000000000000, 0.9238795325112869605, 1.000000000000000000, 0.9238795325112869605, 1.000000000000000000, 0.9238795325112869605, 1.000000000000000000, 0.9238795325112869605, 1.000000000000000000, 0.9238795325112869605, 1.000000000000000000, 0.9238795325112869605, 1.000000000000000000, 0.9238795325112869605, 1.000000000000000000, 0.9238795325112869605, 1.000000000000000000, 0.9238795325112869605, 1.000000000000000000, 0.9238795325112869605, 1.000000000000000000, 0.9238795325112869605, 1.000000000000000000, 0.9238795325112869605, 1.000000000000000000, 0.9238795325112869605, 1.000000000000000000, 0.9238795325112869605, 1.000000000000000000, 0.9238795325112869605, 1.000000000000000000, 0.9238795325112869605, 1.000000000000000000, 0.9238795325112869605, 1.000000000000000000, 0.9238795325112869605, 1.000000000000000000, 0.9238795325112869605, 1.000000000000000000, 0.9238795325112869605, 1.000000000000000000, 0.9238795325112869605, 1.000000000000000000, 0.9238795325112869605, 1.000000000000000000, 0.9238795325112869605, 1.000000000000000000, 0.9238795325112869605, 1.000000000000000000) ) ) 
 REPRESENTATION_ITEM ( '' )  SURFACE ( )  );
#12008 = CARTESIAN_POINT ( 'NONE',  ( -13.35197469415439464, -5.063788272970252358, -18.19321519141019294 ) ) ;
#12009 = CARTESIAN_POINT ( 'NONE',  ( 83.51226282631382958, -32.71650970335249298, -21.69069357203322213 ) ) ;
#12010 = CARTESIAN_POINT ( 'NONE',  ( 122.0994348109119443, 0.9020085738987339008, -11.91225656197089222 ) ) ;
#12011 = CARTESIAN_POINT ( 'NONE',  ( 117.5045748109119756, 0.5811942927096110934, -14.16772938898807510 ) ) ;
#12012 = CARTESIAN_POINT ( 'NONE',  ( 107.9128015045248219, -2.477300249445798297, -7.631215200338321125 ) ) ;
#12013 = CARTESIAN_POINT ( 'NONE',  ( 115.7460481442453357, 0.9020085738987339008, -11.91225656197089222 ) ) ;
#12014 = DIRECTION ( 'NONE',  ( -1.000000000000000000, 1.091021054073464066E-15, 0.000000000000000000 ) ) ;
#12015 = ORIENTED_EDGE ( 'NONE', *, *, #5258, .T. ) ;
#12016 = CARTESIAN_POINT ( 'NONE',  ( 112.4235952706805790, 0.3193521225029610777, -14.64321520033830026 ) ) ;
#12017 = VECTOR ( 'NONE', #44005, 1000.000000000000227 ) ;
#12018 = CARTESIAN_POINT ( 'NONE',  ( 118.8092881442453290, -9.988377603198976828, -10.36322818467138340 ) ) ;
#12019 = CARTESIAN_POINT ( 'NONE',  ( 112.3424481442453384, -6.344957434206662583, -7.627207830600332805 ) ) ;
#12020 = SHAPE_DEFINITION_REPRESENTATION ( #7751, #10805 ) ;
#12021 = CARTESIAN_POINT ( 'NONE',  ( 113.3068014775786594, -1.833838273342658809, -17.42832698103878286 ) ) ;
#12022 = CARTESIAN_POINT ( 'NONE',  ( 111.7184548109119788, -0.8288870151387760510, -10.36305467784173118 ) ) ;
#12023 = CIRCLE ( 'NONE', #21488, 0.5000000000000004441 ) ;
#12024 = CARTESIAN_POINT ( 'NONE',  ( 109.4407702545248355, -10.62599879583958717, -15.77991374673208469 ) ) ;
#12025 = CARTESIAN_POINT ( 'NONE',  ( 121.7590748109119687, -2.084020599724406786, -8.691656652584148546 ) ) ;
#12026 = CARTESIAN_POINT ( 'NONE',  ( 110.7603796295247918, -4.863998795839590272, -19.15521520033831493 ) ) ;
#12027 = FACE_OUTER_BOUND ( 'NONE', #4193, .T. ) ;
#12028 = ORIENTED_EDGE ( 'NONE', *, *, #38977, .F. ) ;
#12029 = EDGE_CURVE ( 'NONE', #23066, #735, #4397, .T. ) ;
#12030 = DIRECTION ( 'NONE',  ( 1.000000000000000000, 0.000000000000000000, -0.000000000000000000 ) ) ;
#12031 = CARTESIAN_POINT ( 'NONE',  ( 123.0637881442452937, -0.4660016031367893996, -10.09054647747474043 ) ) ;
#12032 = ORIENTED_EDGE ( 'NONE', *, *, #24000, .F. ) ;
#12033 = FACE_OUTER_BOUND ( 'NONE', #4346, .T. ) ;
#12034 = CARTESIAN_POINT ( 'NONE',  ( 65.52359245923510400, -2.352842260041322575, -8.554674841066066904 ) ) ;
#12035 = CARTESIAN_POINT ( 'NONE',  ( 77.77634386988368931, 3.254514819260763581, -14.64321520033831447 ) ) ;
#12036 = CARTESIAN_POINT ( 'NONE',  ( 119.6034614775786196, -3.505236298600246325, -18.68346056562440793 ) ) ;
#12037 = CARTESIAN_POINT ( 'NONE',  ( 111.9645664091100912, -0.9924539043446216624, -17.29976612834909133 ) ) ;
#12038 = CARTESIAN_POINT ( 'NONE',  ( 64.18133890301322708, -35.39523410098156120, -5.871648730333205890 ) ) ;
#12039 = CARTESIAN_POINT ( 'NONE',  ( 124.7655881442452852, -9.859900752359378018, -12.68260735090039759 ) ) ;
#12040 = CARTESIAN_POINT ( 'NONE',  ( 94.20708369096698220, -25.99489077589524300, -13.39321520033831447 ) ) ;
#12041 = CARTESIAN_POINT ( 'NONE',  ( 123.6310548109119765, -4.153390946401325223, -8.397313243818185668 ) ) ;
#12042 = AXIS2_PLACEMENT_3D ( 'NONE', #7041, #7702, #17748 ) ;
#12043 = CARTESIAN_POINT ( 'NONE',  ( 90.33554924625337890, -25.23119213852205789, -15.24166438581092109 ) ) ;
#12044 = B_SPLINE_CURVE_WITH_KNOTS ( 'NONE', 3,
 ( #44207, #11890, #1167, #4358 ),
 .UNSPECIFIED., .F., .F.,
 ( 4, 4 ),
 ( 4.131326245856534688E-18, 6.689972255565380249E-05 ),
 .UNSPECIFIED. ) ;
#12045 = CARTESIAN_POINT ( 'NONE',  ( 118.1852948109119836, -4.153390946401325223, -8.397313243818185668 ) ) ;
#12046 = CARTESIAN_POINT ( 'NONE',  ( 124.1983214775786166, -1.833838273342659697, -17.42832698103878286 ) ) ;
#12047 = CARTESIAN_POINT ( 'NONE',  ( 119.8303681442453126, -10.63000616557722466, -14.87417383870573495 ) ) ;
#12048 = EDGE_CURVE ( 'NONE', #35857, #23574, #5853, .T. ) ;
#12049 = CARTESIAN_POINT ( 'NONE',  ( 117.2209414775786485, -7.893985811506177619, -18.51759400769804742 ) ) ;
#12050 = CARTESIAN_POINT ( 'NONE',  ( 113.1217858795247935, -8.402594152722688392, -9.854619843455216355 ) ) ;
#12051 = AXIS2_PLACEMENT_3D ( 'NONE', #42474, #1188, #15100 ) ;
#12052 = CARTESIAN_POINT ( 'NONE',  ( 125.7299414775786346, -10.15424416112533912, -14.75197769757731336 ) ) ;
#12053 = ORIENTED_EDGE ( 'NONE', *, *, #28168, .T. ) ;
#12054 = CARTESIAN_POINT ( 'NONE',  ( 120.3976348109119812, -1.834011780172310813, -8.268836392978581529 ) ) ;
#12055 = CARTESIAN_POINT ( 'NONE',  ( 113.3301452545248083, 0.8980012041604421569, -11.00651665394454071 ) ) ;
#12056 = CARTESIAN_POINT ( 'NONE',  ( 110.6214733795247867, -1.325403438956436419, -9.854619843455211026 ) ) ;
#12057 = CARTESIAN_POINT ( 'NONE',  ( 85.82015659721905365, -24.14644159042263993, -12.62951656296512937 ) ) ;
#12058 = CARTESIAN_POINT ( 'NONE',  ( 113.6471614775786492, -4.153390946401321671, -8.397313243818183892 ) ) ;
#12059 = CARTESIAN_POINT ( 'NONE',  ( 70.19189222814998175, -57.25954915413987578, -36.10662921840084749 ) ) ;
#12060 = B_SPLINE_CURVE_WITH_KNOTS ( 'NONE', 3,
 ( #27496, #14249, #31342, #14029 ),
 .UNSPECIFIED., .F., .F.,
 ( 4, 4 ),
 ( 0.000000000000000000, 1.000000000000000000 ),
 .UNSPECIFIED. ) ;
#12061 = CARTESIAN_POINT ( 'NONE',  ( 116.8028015045247940, -6.936859964151250502, -18.39754474579286025 ) ) ;
#12062 = ORIENTED_EDGE ( 'NONE', *, *, #41297, .F. ) ;
#12063 = CARTESIAN_POINT ( 'NONE',  ( 111.8319081442453182, -5.638512984488999180, -18.83840828888717311 ) ) ;
#12064 = CARTESIAN_POINT ( 'NONE',  ( -13.55933139336933557, -4.790867379097090151, -17.98576441024524897 ) ) ;
#12065 = CARTESIAN_POINT ( 'NONE',  ( 120.0212673109119805, 0.2312338769422704887, -16.08380026872395874 ) ) ;
#12066 = DIRECTION ( 'NONE',  ( 0.9908103287288504424, -0.1352586133457952255, -0.000000000000000000 ) ) ;
#12067 = CARTESIAN_POINT ( 'NONE',  ( 106.1764733795248219, -1.325403438956436419, -9.854619843455211026 ) ) ;
#12068 = ORIENTED_EDGE ( 'NONE', *, *, #11791, .T. ) ;
#12069 = CARTESIAN_POINT ( 'NONE',  ( 116.5969481442453031, 0.5811942927096154232, -14.16772938898807155 ) ) ;
#12070 = DIRECTION ( 'NONE',  ( 0.9387755102040816757, -0.3445294493088600918, 0.000000000000000000 ) ) ;
#12071 = CARTESIAN_POINT ( 'NONE',  ( 121.5888948109119809, 0.1319031606808879209, -14.10382304977623669 ) ) ;
#12072 = CARTESIAN_POINT ( 'NONE',  ( 113.8740681442453138, -9.859900752359374465, -12.68260735090039404 ) ) ;
#12073 = DIRECTION ( 'NONE',  ( 1.000000000000000000, 0.000000000000000000, -0.000000000000000000 ) ) ;
#12074 = CARTESIAN_POINT ( 'NONE',  ( 71.77086717554882966, -26.54201219542348511, -4.893215200338314474 ) ) ;
#12075 = CARTESIAN_POINT ( 'NONE',  ( 113.5904348109119866, -7.893985811506177619, -18.51759400769804742 ) ) ;
#12076 = CIRCLE ( 'NONE', #37546, 6.500000000000000888 ) ;
#12077 = CARTESIAN_POINT ( 'NONE',  ( 71.37572422742091760, -11.86958442233774313, -21.89321520033831447 ) ) ;
#12078 = CARTESIAN_POINT ( 'NONE',  ( 122.6667014775786413, -7.893985811506177619, -18.51759400769804742 ) ) ;
#12079 = CARTESIAN_POINT ( 'NONE',  ( 136.8340972670098097, -9.953648946029552746, -15.66212078552328713 ) ) ;
#12080 = ORIENTED_EDGE ( 'NONE', *, *, #7456, .T. ) ;
#12081 = CARTESIAN_POINT ( 'NONE',  ( 113.1366214775786432, -1.834011780172310813, -8.268836392978581529 ) ) ;
#12082 = CARTESIAN_POINT ( 'NONE',  ( 124.1983214775786166, -8.166667518702819706, -8.995218007635861213 ) ) ;
#12083 = AXIS2_PLACEMENT_3D ( 'NONE', #20400, #13554, #41385 ) ;
#12084 = DIRECTION ( 'NONE',  ( 0.7871354856660198740, 0.4483307682966886643, 0.4235767337848242442 ) ) ;
#12085 = CARTESIAN_POINT ( 'NONE',  ( 123.5176014775786228, -0.8288870151387760510, -10.36305467784173118 ) ) ;
#12086 = ORIENTED_EDGE ( 'NONE', *, *, #33114, .F. ) ;
#12087 = CARTESIAN_POINT ( 'NONE',  ( 119.2063748109119814, -1.561330072975668504, -17.79121239304076951 ) ) ;
#12088 = VECTOR ( 'NONE', #43603, 1000.000000000000114 ) ;
#12089 = DIRECTION ( 'NONE',  ( -0.000000000000000000, -0.9284778069183721172, -0.3713878862591650232 ) ) ;
#12090 = CARTESIAN_POINT ( 'NONE',  ( 76.63408154409412987, 1.697290617957241565, -15.89321520033831447 ) ) ;
#12091 = CARTESIAN_POINT ( 'NONE',  ( 109.9649712410415816, 0.7607806665038616689, -12.14321520033831625 ) ) ;
#12092 = CARTESIAN_POINT ( 'NONE',  ( 136.2267163768036937, -5.541130735199761403, -7.574948583682552083 ) ) ;
#12093 = CARTESIAN_POINT ( 'NONE',  ( 113.4202548109119846, 0.1319031606808879209, -14.10382304977623669 ) ) ;
#12094 = CARTESIAN_POINT ( 'NONE',  ( 124.9868051361299166, -1.575707845324203493, -20.23615509330177531 ) ) ;
#12095 = EDGE_CURVE ( 'NONE', #22775, #5648, #16152, .T. ) ;
#12096 = CARTESIAN_POINT ( 'NONE',  ( 125.3553822467254122, -2.689292442315842191, -20.09621397316101366 ) ) ;
#12097 = CIRCLE ( 'NONE', #25929, 1.499999999999996225 ) ;
#12098 = CARTESIAN_POINT ( 'NONE',  ( 113.5337081442453240, -0.8288870151387760510, -10.36305467784173118 ) ) ;
#12099 = CARTESIAN_POINT ( 'NONE',  ( 126.6375681442452930, -10.15424416112533912, -14.75197769757731336 ) ) ;
#12100 = CARTESIAN_POINT ( 'NONE',  ( 116.6348121297881733, -9.548805560831048922, -15.25421616637334488 ) ) ;
#12101 = CARTESIAN_POINT ( 'NONE',  ( 121.9859814775786333, -9.565557343593413364, -10.61323700422348004 ) ) ;
#12102 = DIRECTION ( 'NONE',  ( 0.000000000000000000, -0.3818493186865927203, 0.9242245927363029745 ) ) ;
#12103 = CARTESIAN_POINT ( 'NONE',  ( 118.6958348109119754, -6.344957434206665248, -7.627207830600338134 ) ) ;
#12104 = CARTESIAN_POINT ( 'NONE',  ( 121.6456214775786293, -10.63000616557722466, -14.87417383870573495 ) ) ;
#12105 = EDGE_LOOP ( 'NONE', ( #18265, #25083, #40561, #43336 ) ) ;
#12106 = CARTESIAN_POINT ( 'NONE',  ( 114.9716510812576757, -0.01829820670803256055, -12.14321520033831625 ) ) ;
#12107 = CARTESIAN_POINT ( 'NONE',  ( 110.8992858795247827, -0.7896495226426338832, -17.46756447353520159 ) ) ;
#12108 = AXIS2_PLACEMENT_3D ( 'NONE', #11198, #5912, #26454 ) ;
#12109 = CARTESIAN_POINT ( 'NONE',  ( 109.5796765045248122, -2.791137627527939813, -8.388885654883777576 ) ) ;
#12110 = CARTESIAN_POINT ( 'NONE',  ( 108.5378796295247810, -4.863998795839590272, -8.388885654883775800 ) ) ;
#12111 = CARTESIAN_POINT ( 'NONE',  ( 125.6164881442453094, -9.565557343593953377, -10.61323700422440197 ) ) ;
#12112 = CARTESIAN_POINT ( 'NONE',  ( 116.1998614775786507, -10.63000616557722466, -14.87417383870573495 ) ) ;
#12113 = VERTEX_POINT ( 'NONE', #2223 ) ;
#12114 = CARTESIAN_POINT ( 'NONE',  ( 105.9681140045248355, -10.62599879583958717, -11.00651665394454604 ) ) ;
#12115 = DIRECTION ( 'NONE',  ( -0.9609149988134837450, 0.1028163501681639419, -0.2570431154366518145 ) ) ;
#12116 = CARTESIAN_POINT ( 'NONE',  ( 115.3489614775786407, -0.8288870151387760510, -10.36305467784173118 ) ) ;
#12118 = CIRCLE ( 'NONE', #12839, 5.132259260909266985 ) ;
#12117 = CARTESIAN_POINT ( 'NONE',  ( 112.9097148109120070, 0.2603800115204892296, -16.42320221600525088 ) ) ;
#12119 = CARTESIAN_POINT ( 'NONE',  ( 120.1707281442453166, 0.2603800115204892296, -16.42320221600525088 ) ) ;
#12120 = CARTESIAN_POINT ( 'NONE',  ( 111.6632702545248605, -10.62599879583958717, -15.77991374673208469 ) ) ;
#12121 = CARTESIAN_POINT ( 'NONE',  ( 117.2294421295247844, 1.035107641088057973, -21.72657133228191739 ) ) ;
#12122 = ORIENTED_EDGE ( 'NONE', *, *, #40151, .F. ) ;
#12123 = DIRECTION ( 'NONE',  ( 0.000000000000000000, 0.000000000000000000, 1.000000000000000000 ) ) ;
#12124 = CARTESIAN_POINT ( 'NONE',  ( 117.6747548109119919, -7.643976991954077427, -18.09477374809248928 ) ) ;
#12125 = CARTESIAN_POINT ( 'NONE',  ( 117.6747548109119919, -1.834011780172310813, -8.268836392978581529 ) ) ;
#12126 = CARTESIAN_POINT ( 'NONE',  ( 116.5969481442453031, 0.5811942927096154232, -14.16772938898807155 ) ) ;
#12127 = CARTESIAN_POINT ( 'NONE',  ( 61.27778620743471549, -25.99489077589588604, -13.39321520033831447 ) ) ;
#12128 = CARTESIAN_POINT ( 'NONE',  ( 123.9146881442452894, -10.15424416112533912, -14.75197769757731336 ) ) ;
#12129 = CARTESIAN_POINT ( 'NONE',  ( 115.1220548109119761, -1.833838273342658809, -17.42832698103878286 ) ) ;
#12130 = VERTEX_POINT ( 'NONE', #2003 ) ;
#12131 = CARTESIAN_POINT ( 'NONE',  ( 124.4662673109119737, -9.289237151508434209, -11.05642687123711276 ) ) ;
#12132 = CIRCLE ( 'NONE', #31071, 1.500000000000000888 ) ;
#12133 = CARTESIAN_POINT ( 'NONE',  ( 113.1366214775786432, -1.834011780172310813, -8.268836392978581529 ) ) ;
#12134 = CARTESIAN_POINT ( 'NONE',  ( 117.9016614775786280, -0.1624402480850797581, -16.17319339645315424 ) ) ;
#12135 = ORIENTED_EDGE ( 'NONE', *, *, #41766, .T. ) ;
#12136 = CARTESIAN_POINT ( 'NONE',  ( 120.5768923109119868, -0.4387604401700512802, -15.73000352943951619 ) ) ;
#12137 = CARTESIAN_POINT ( 'NONE',  ( 115.0086014775786509, -4.089484607189486809, -7.948022111789456723 ) ) ;
#12138 = CARTESIAN_POINT ( 'NONE',  ( 107.3571765045248299, -2.791137627527939813, -8.388885654883777576 ) ) ;
#12139 = CARTESIAN_POINT ( 'NONE',  ( 118.8459235400977718, -1.223627541775709426, -16.99192386690442547 ) ) ;
#12140 = AXIS2_PLACEMENT_3D ( 'NONE', #6146, #31210, #6381 ) ;
#12141 = ORIENTED_EDGE ( 'NONE', *, *, #15267, .T. ) ;
#12142 = EDGE_LOOP ( 'NONE', ( #3094, #5776, #699, #18358 ) ) ;
#12143 = CARTESIAN_POINT ( 'NONE',  ( 122.3830681442452857, -1.833838273342659697, -17.42832698103878286 ) ) ;
#12144 = CARTESIAN_POINT ( 'NONE',  ( 119.8303681442453126, 0.4262465694468514643, -12.03445270309931736 ) ) ;
#12145 = DIRECTION ( 'NONE',  ( 0.000000000000000000, 0.000000000000000000, 1.000000000000000000 ) ) ;
#12146 = AXIS2_PLACEMENT_3D ( 'NONE', #29408, #40350, #19594 ) ;
#12147 = ORIENTED_EDGE ( 'NONE', *, *, #25053, .F. ) ;
#12148 = FACE_BOUND ( 'NONE', #5991, .T. ) ;
#12149 = LINE ( 'NONE', #39511, #12088 ) ;
#12150 = CARTESIAN_POINT ( 'NONE',  ( 107.4266296295248821, -4.863998795839590272, -19.15521520033831493 ) ) ;
#12151 = CARTESIAN_POINT ( 'NONE',  ( 114.8384214775786489, 0.9020085738987339008, -11.91225656197089222 ) ) ;
#12153 = CARTESIAN_POINT ( 'NONE',  ( 117.3911214775786505, -7.894159318335828068, -9.358103419637847864 ) ) ;
#12152 = CARTESIAN_POINT ( 'NONE',  ( 114.9518748109119883, -1.834011780172310813, -8.268836392978581529 ) ) ;
#12154 = CARTESIAN_POINT ( 'NONE',  ( 119.9438214775786378, -2.084020599724406786, -8.691656652584148546 ) ) ;
#12155 = DIRECTION ( 'NONE',  ( -1.000000000000000000, 0.000000000000000000, 0.000000000000000000 ) ) ;
#12156 = ORIENTED_EDGE ( 'NONE', *, *, #36779, .F. ) ;
#12157 = CARTESIAN_POINT ( 'NONE',  ( 118.3554748109119998, -9.565557343593413364, -10.61323700422348004 ) ) ;
#12158 = CARTESIAN_POINT ( 'NONE',  ( 124.9924948109119924, -5.574606645277164318, -18.38911715685844683 ) ) ;
#12159 = CARTESIAN_POINT ( 'NONE',  ( 113.1912390045248031, 0.8980012041604421569, -15.77991374673208469 ) ) ;
#12160 = CARTESIAN_POINT ( 'NONE',  ( 115.6915515045247531, -6.936859964151250502, -18.39754474579286025 ) ) ;
#12161 = CARTESIAN_POINT ( 'NONE',  ( 111.6632702545248605, -10.62599879583958717, -15.77991374673208469 ) ) ;
#12162 = CIRCLE ( 'NONE', #5606, 5.999999999999997335 ) ;
#12163 = CARTESIAN_POINT ( 'NONE',  ( 120.1707281442453166, 0.2603800115204892296, -16.42320221600525088 ) ) ;
#12164 = VERTEX_POINT ( 'NONE', #15929 ) ;
#12165 = CARTESIAN_POINT ( 'NONE',  ( 120.0005481442453146, -5.638512984488999180, -18.83840828888717311 ) ) ;
#12166 = CARTESIAN_POINT ( 'NONE',  ( 75.95778847736481509, -3.256761025687722189, -18.79321520033831661 ) ) ;
#12167 = CARTESIAN_POINT ( 'NONE',  ( 71.02242295334774269, -54.12449018237889220, -37.95742420651561133 ) ) ;
#12168 = CARTESIAN_POINT ( 'NONE',  ( 117.9583881442453048, -10.30919188438810075, -12.61870101168855918 ) ) ;
#12169 = CARTESIAN_POINT ( 'NONE',  ( 116.8238548109119819, -4.089484607189486809, -7.948022111789456723 ) ) ;
#12170 = CARTESIAN_POINT ( 'NONE',  ( 111.4241771286805260, -2.495269033102075262, -17.79652296963211455 ) ) ;
#12171 = CARTESIAN_POINT ( 'NONE',  ( 116.4298796982476318, -11.97487242489886761, -6.682657204922437089 ) ) ;
#12172 = VECTOR ( 'NONE', #19681, 1000.000000000000227 ) ;
#12173 = ORIENTED_EDGE ( 'NONE', *, *, #9730, .F. ) ;
#12174 = DIRECTION ( 'NONE',  ( 0.000000000000000000, 0.6004852223388321697, -0.7996358532186279566 ) ) ;
#12175 = CARTESIAN_POINT ( 'NONE',  ( 109.2294431053738464, -10.03736769325571032, -11.07138121511321316 ) ) ;
#12176 = CARTESIAN_POINT ( 'NONE',  ( 120.6245414775786458, -0.1624402480850797581, -16.17319339645315424 ) ) ;
#12177 = CARTESIAN_POINT ( 'NONE',  ( 110.2047546295247855, -4.863998795839590272, -18.39754474579285315 ) ) ;
#12178 = CARTESIAN_POINT ( 'NONE',  ( 105.4819421295248247, 0.8980012041604618078, -13.39321520033831447 ) ) ;
#12179 = CARTESIAN_POINT ( 'NONE',  ( 118.2987481442453088, -7.894159318335828068, -9.358103419637847864 ) ) ;
#12180 = DIRECTION ( 'NONE',  ( 1.000000000000000000, 0.000000000000000000, 0.000000000000000000 ) ) ;
#12181 = CARTESIAN_POINT ( 'NONE',  ( 70.09935913692072518, -25.95240877518153511, -5.724109476187205559 ) ) ;
#12182 = CARTESIAN_POINT ( 'NONE',  ( 112.7395348109119766, -4.153390946401321671, -8.397313243818183892 ) ) ;
#12183 = CARTESIAN_POINT ( 'NONE',  ( 121.0216281442452981, -1.561330072975668948, -17.79121239304076951 ) ) ;
#12184 = VERTEX_POINT ( 'NONE', #9084 ) ;
#12185 = AXIS2_PLACEMENT_3D ( 'NONE', #8161, #5403, #1309 ) ;
#12186 = CARTESIAN_POINT ( 'NONE',  ( 120.2274548109119934, -9.859900752359378018, -12.68260735090039759 ) ) ;
#12187 = CARTESIAN_POINT ( 'NONE',  ( 114.7249681442453237, 0.2603800115204892296, -16.42320221600525088 ) ) ;
#12188 = CARTESIAN_POINT ( 'NONE',  ( 122.0994348109119443, 0.9020085738987339008, -11.91225656197089222 ) ) ;
#12189 = CARTESIAN_POINT ( 'NONE',  ( 119.9438214775786378, -2.084020599724406786, -8.691656652584148546 ) ) ;
#12190 = ORIENTED_EDGE ( 'NONE', *, *, #17038, .F. ) ;
#12191 = CARTESIAN_POINT ( 'NONE',  ( 116.3852670589982381, -1.063912429576147067, -17.20460841810472985 ) ) ;
#12192 =( BOUNDED_CURVE ( )  B_SPLINE_CURVE ( 2, ( #493, #11218, #10991, #42452, #24893, #31944, #42675, #35355, #4131, #18051, #5030, #11445, #8684, #4580, #29885, #25790, #32395 ),
 .UNSPECIFIED., .F., .T. ) 
 B_SPLINE_CURVE_WITH_KNOTS ( ( 3, 2, 2, 2, 2, 2, 2, 2, 3 ),
 ( 0.5171282416568590001, 0.5234375000000000000, 0.5312500000000000000, 0.5390625000000000000, 0.5468750000000000000, 0.5546875000000000000, 0.5625000000000000000, 0.5703125000000000000, 0.5766217583431409999 ),
 .UNSPECIFIED. ) 
 CURVE ( )  GEOMETRIC_REPRESENTATION_ITEM ( )  RATIONAL_B_SPLINE_CURVE ( ( 0.9763430640195970289, 0.9385262470928680267, 1.000000000000000000, 0.9238795325112869605, 1.000000000000000000, 0.9238795325112869605, 1.000000000000000000, 0.9238795325112869605, 1.000000000000000000, 0.9238795325112869605, 1.000000000000000000, 0.9238795325112869605, 1.000000000000000000, 0.9238795325112869605, 1.000000000000000000, 0.9385262470928680267, 0.9763430640195970289 ) ) 
 REPRESENTATION_ITEM ( '' )  );
#12193 = EDGE_CURVE ( 'NONE', #43318, #38775, #21881, .T. ) ;
#12194 = CARTESIAN_POINT ( 'NONE',  ( 119.3765548109119834, 0.9020085738987339008, -11.91225656197089222 ) ) ;
#12195 = CARTESIAN_POINT ( 'NONE',  ( 70.19189222814998175, -63.93370346063255738, -42.00736267657491396 ) ) ;
#12196 = EDGE_CURVE ( 'NONE', #22388, #25605, #26636, .T. ) ;
#12197 = CARTESIAN_POINT ( 'NONE',  ( 121.1918081442452859, 0.9020085738987339008, -11.91225656197089222 ) ) ;
#12198 = CARTESIAN_POINT ( 'NONE',  ( 117.3719165460472027, -2.191907684172563986, -18.20049396185734025 ) ) ;
#12199 = DIRECTION ( 'NONE',  ( 0.9908103287288504424, -0.1352586133457952255, -0.000000000000000000 ) ) ;
#12200 = CARTESIAN_POINT ( 'NONE',  ( 118.8493976481213821, -2.395992375830759524, -17.92872468182853396 ) ) ;
#12201 = CARTESIAN_POINT ( 'NONE',  ( 111.0381921295247878, -9.868328341294093420, -13.39321520033831447 ) ) ;
#12202 = DIRECTION ( 'NONE',  ( 3.183628217498455203E-14, 1.000000000000000000, 0.000000000000000000 ) ) ;
#12203 = CARTESIAN_POINT ( 'NONE',  ( 135.3184548109119874, -10.36826876090623450, -11.00511718064541178 ) ) ;
#12204 = CARTESIAN_POINT ( 'NONE',  ( 118.4122014775786340, -9.859900752359374465, -12.68260735090039404 ) ) ;
#12205 = CARTESIAN_POINT ( 'NONE',  ( 124.7088614775786226, 0.2603800115204892296, -16.42320221600525088 ) ) ;
#12206 = FACE_OUTER_BOUND ( 'NONE', #2551, .T. ) ;
#12207 = VERTEX_POINT ( 'NONE', #5872 ) ;
#12208 = CARTESIAN_POINT ( 'NONE',  ( 85.70478001548416103, -26.75858941326842810, -11.54476601486570964 ) ) ;
#12209 = CARTESIAN_POINT ( 'NONE',  ( 110.3436608795247764, -1.325403438956436419, -16.93181055722141792 ) ) ;
#12210 = VECTOR ( 'NONE', #32488, 999.9999999999998863 ) ;
#12211 = CARTESIAN_POINT ( 'NONE',  ( 117.4478481442453131, -9.565557343593413364, -10.61323700422348004 ) ) ;
#12212 = CARTESIAN_POINT ( 'NONE',  ( 113.5214761498677376, -2.324775150319240868, -18.02356106541842351 ) ) ;
#12213 = ADVANCED_FACE ( 'NONE', ( #19794 ), #20441, .T. ) ;
#12214 = DIRECTION ( 'NONE',  ( -0.9908103287288505534, 0.1352586133457944206, 0.000000000000000000 ) ) ;
#12215 = DIRECTION ( 'NONE',  ( 1.000000000000000000, 0.000000000000000000, 0.000000000000000000 ) ) ;
#12217 = CARTESIAN_POINT ( 'NONE',  ( 124.3685014775786328, -10.63000616557722466, -14.87417383870573495 ) ) ;
#12216 = CARTESIAN_POINT ( 'NONE',  ( 64.60379348622299744, -13.80859085231287864, -8.919028783932633431 ) ) ;
#12218 = CARTESIAN_POINT ( 'NONE',  ( 123.6310548109119765, -4.153390946401325223, -8.397313243818185668 ) ) ;
#12219 = ORIENTED_EDGE ( 'NONE', *, *, #1152, .T. ) ;
#12220 = DIRECTION ( 'NONE',  ( 0.000000000000000000, 0.000000000000000000, 1.000000000000000000 ) ) ;
#12221 = CARTESIAN_POINT ( 'NONE',  ( 111.0381921295247878, -9.868328341294093420, -13.39321520033831447 ) ) ;
#12222 = CARTESIAN_POINT ( 'NONE',  ( 124.5386814775786206, -4.153390946401325223, -8.397313243818185668 ) ) ;
#12223 = ADVANCED_FACE ( 'NONE', ( #27766 ), #8763, .T. ) ;
#12224 = CARTESIAN_POINT ( 'NONE',  ( 121.6456214775786293, 0.4262465694468514643, -12.03445270309931736 ) ) ;
#12225 = CARTESIAN_POINT ( 'NONE',  ( 121.3619881442452879, -5.574606645277164318, -18.38911715685844683 ) ) ;
#12226 = EDGE_CURVE ( 'NONE', #259, #6454, #28215, .T. ) ;
#12227 = CARTESIAN_POINT ( 'NONE',  ( 120.9234003923315441, -1.063912429576147511, -17.20460841810472985 ) ) ;
#12228 = CARTESIAN_POINT ( 'NONE',  ( 107.0793640045248196, -10.62599879583958717, -11.00651665394454604 ) ) ;
#12229 = DIRECTION ( 'NONE',  ( 1.000000000000000000, 0.000000000000000000, 0.000000000000000000 ) ) ;
#12230 = DIRECTION ( 'NONE',  ( 0.000000000000000000, 0.3818493186865927203, -0.9242245927363029745 ) ) ;
#12231 = LINE ( 'NONE', #5145, #6644 ) ;
#12232 = AXIS2_PLACEMENT_3D ( 'NONE', #37935, #13330, #3053 ) ;
#12233 = CARTESIAN_POINT ( 'NONE',  ( 110.8298327545248299, -2.477300249445798297, -19.15521520033831138 ) ) ;
#12234 = CARTESIAN_POINT ( 'NONE',  ( 86.34560043013698305, -9.320000780048239619, -16.89321520033831447 ) ) ;
#12235 = CARTESIAN_POINT ( 'NONE',  ( 117.2294421295247844, 1.035107641088057973, -21.72657133228191739 ) ) ;
#12236 = CARTESIAN_POINT ( 'NONE',  ( 121.9859814775786333, 0.2603800115204892296, -16.42320221600525088 ) ) ;
#12237 = CARTESIAN_POINT ( 'NONE',  ( 119.2063748109119814, -1.561330072975668504, -17.79121239304076951 ) ) ;
#12238 = CARTESIAN_POINT ( 'NONE',  ( 107.0099108795247815, -8.938348069036489818, -9.318865927141430916 ) ) ;
#12239 = CARTESIAN_POINT ( 'NONE',  ( 115.6893214775786447, 0.5811942927096154232, -14.16772938898807155 ) ) ;
#12240 = CARTESIAN_POINT ( 'NONE',  ( 78.69189222814998175, -69.76310523276724496, -16.89321520033831447 ) ) ;
#12241 = VERTEX_POINT ( 'NONE', #20921 ) ;
#12242 = UNCERTAINTY_MEASURE_WITH_UNIT (LENGTH_MEASURE( 1.000000000000000082E-05 ), #15675, 'distance_accuracy_value', 'NONE');
#12243 = CARTESIAN_POINT ( 'NONE',  ( 70.19189222814998175, -53.54563792646638376, -34.62107767336419073 ) ) ;
#12244 = EDGE_CURVE ( 'NONE', #24220, #36515, #31350, .T. ) ;
#12245 = CARTESIAN_POINT ( 'NONE',  ( 123.4041481442452834, -10.30919188438810075, -12.61870101168855918 ) ) ;
#12246 = CARTESIAN_POINT ( 'NONE',  ( 118.7525614775786380, -8.166667518702819706, -8.995218007635861213 ) ) ;
#12247 = CARTESIAN_POINT ( 'NONE',  ( 125.4463081442452932, -4.153390946401325223, -8.397313243818185668 ) ) ;
#12248 = APPLICATION_PROTOCOL_DEFINITION ( 'draft international standard', 'automotive_design', 1998, #23025 ) ;
#12249 = ADVANCED_FACE ( 'NONE', ( #31616 ), #39211, .F. ) ;
#12250 = CARTESIAN_POINT ( 'NONE',  ( 114.2144281442453178, -1.833838273342658809, -17.42832698103878286 ) ) ;
#12251 = CARTESIAN_POINT ( 'NONE',  ( 111.6050014775786536, 0.1319031606808879209, -14.10382304977623669 ) ) ;
#12252 = EDGE_CURVE ( 'NONE', #10287, #13764, #30847, .T. ) ;
#12253 = EDGE_CURVE ( 'NONE', #1633, #27848, #6563, .T. ) ;
#12254 = CARTESIAN_POINT ( 'NONE',  ( 110.4825671295247815, -10.62599879583958540, -13.39321520033831447 ) ) ;
#12255 = CARTESIAN_POINT ( 'NONE',  ( 120.6245414775786458, -0.1624402480850797581, -16.17319339645315424 ) ) ;
#12256 = CARTESIAN_POINT ( 'NONE',  ( 110.6214733795247867, -8.938348069036441856, -17.46756447353520869 ) ) ;
#12257 = CYLINDRICAL_SURFACE ( 'NONE', #32259, 3.000000000000001776 ) ;
#12258 = EDGE_LOOP ( 'NONE', ( #41641, #8462, #12937, #3144 ) ) ;
#12259 = CARTESIAN_POINT ( 'NONE',  ( 123.9584548109119737, -4.863998795839242995, -13.39321520033831447 ) ) ;
#12260 = CARTESIAN_POINT ( 'NONE',  ( 123.0070614775786169, 0.9020085738987339008, -11.91225656197089222 ) ) ;
#12261 = CARTESIAN_POINT ( 'NONE',  ( 122.3736205389825216, -6.126425863531494542, -18.50366489541501380 ) ) ;
#12262 = CARTESIAN_POINT ( 'NONE',  ( 124.8633137343409771, 2.042755831848476866, -9.994361272893446113 ) ) ;
#12263 =( NAMED_UNIT ( * ) PLANE_ANGLE_UNIT ( ) SI_UNIT ( $, .RADIAN. ) );
#12264 = CIRCLE ( 'NONE', #24028, 2.445500000000004448 ) ;
#12265 = CARTESIAN_POINT ( 'NONE',  ( 118.1285681442453068, -2.084020599724406786, -8.691656652584148546 ) ) ;
#12266 = CARTESIAN_POINT ( 'NONE',  ( 112.2289948109119848, -1.834011780172310591, -8.268836392978581529 ) ) ;
#12267 = CARTESIAN_POINT ( 'NONE',  ( 79.79010115959992788, 5.106172230548759572, -4.893215200338314474 ) ) ;
#12268 = CARTESIAN_POINT ( 'NONE',  ( 123.2906948109119867, -1.833838273342659697, -17.42832698103878286 ) ) ;
#12269 = CARTESIAN_POINT ( 'NONE',  ( 121.4797829359119987, -4.283928203966219428, -7.183505701512921782 ) ) ;
#12270 = CARTESIAN_POINT ( 'NONE',  ( 86.75477599865929790, -25.99489077589524300, -13.39321520033831625 ) ) ;
#12271 = CARTESIAN_POINT ( 'NONE',  ( 124.9558295300363966, -11.72760118899441117, -16.72555640187829340 ) ) ;
#12272 = CARTESIAN_POINT ( 'NONE',  ( 123.1772414775786189, -4.089484607189486809, -7.948022111789456723 ) ) ;
#12273 =( BOUNDED_CURVE ( )  B_SPLINE_CURVE ( 2, ( #22788, #15732, #22563, #29184, #29410, #26216, #18921, #40125, #29634, #1364, #8215, #2259, #5678 ),
 .UNSPECIFIED., .F., .T. ) 
 B_SPLINE_CURVE_WITH_KNOTS ( ( 3, 2, 2, 2, 2, 2, 3 ),
 ( 0.01712824165687044931, 0.02343750000000000000, 0.03125000000000000000, 0.03906250000000000000, 0.04687500000000000000, 0.05468750000000000000, 0.06249487795845730387 ),
 .UNSPECIFIED. ) 
 CURVE ( )  GEOMETRIC_REPRESENTATION_ITEM ( )  RATIONAL_B_SPLINE_CURVE ( ( 0.9763430640194580290, 0.9385262470929809364, 1.000000000000000000, 0.9238795325112869605, 1.000000000000000000, 0.9238795325112869605, 1.000000000000000000, 0.9238795325112869605, 1.000000000000000000, 0.9238795325112869605, 1.000000000000000000, 0.9239294387124680208, 0.9999002530367769870 ) ) 
 REPRESENTATION_ITEM ( '' )  );
#12274 = CARTESIAN_POINT ( 'NONE',  ( 118.1285681442453068, -2.084020599724406786, -8.691656652584148546 ) ) ;
#12275 = CARTESIAN_POINT ( 'NONE',  ( 122.8936081442453059, -9.565557343593413364, -10.61323700422348004 ) ) ;
#12276 = ORIENTED_EDGE ( 'NONE', *, *, #3829, .F. ) ;
#12277 = CARTESIAN_POINT ( 'NONE',  ( 121.5888948109119809, -10.30919188438810075, -12.61870101168855918 ) ) ;
#12278 = CARTESIAN_POINT ( 'NONE',  ( 116.8238548109119819, -4.089484607189486809, -7.948022111789456723 ) ) ;
#12279 = CARTESIAN_POINT ( 'NONE',  ( 113.6774108795247997, -1.325403438956436419, -16.93181055722141792 ) ) ;
#12280 = DIRECTION ( 'NONE',  ( -1.000000000000000000, 0.000000000000000000, 0.000000000000000000 ) ) ;
#12281 = CARTESIAN_POINT ( 'NONE',  ( 125.9001214775786224, -5.574606645277164318, -18.38911715685844683 ) ) ;
#12282 = CARTESIAN_POINT ( 'NONE',  ( 120.9649014775786355, -3.383040157471821630, -19.15922257007629170 ) ) ;
#12283 = CARTESIAN_POINT ( 'NONE',  ( 113.2606921295247702, 0.8980012041604618078, -13.39321520033831447 ) ) ;
#12284 = CARTESIAN_POINT ( 'NONE',  ( 107.9128015045248219, -6.936859964151250502, -18.39754474579286025 ) ) ;
#12285 = CARTESIAN_POINT ( 'NONE',  ( 88.07785292173620917, -25.38011337280982715, -14.88121679464376257 ) ) ;
#12286 = CARTESIAN_POINT ( 'NONE',  ( 113.4769814775786330, 0.4262465694468514643, -12.03445270309931736 ) ) ;
#12287 = CARTESIAN_POINT ( 'NONE',  ( 115.4137390045248566, -9.868328341294098749, -11.32035403202665869 ) ) ;
#12288 = ORIENTED_EDGE ( 'NONE', *, *, #1363, .T. ) ;
#12289 = CARTESIAN_POINT ( 'NONE',  ( 125.3895814775786448, -2.084020599724406786, -8.691656652584148546 ) ) ;
#12290 = CARTESIAN_POINT ( 'NONE',  ( 122.6604860609119640, -6.564341423271550902, -7.887810678476487425 ) ) ;
#12291 = CARTESIAN_POINT ( 'NONE',  ( 122.0354079359119908, -5.444069387712269226, -19.60292469916370450 ) ) ;
#12292 = CARTESIAN_POINT ( 'NONE',  ( 123.8772847346423163, -8.435056900666539903, -17.43606523319152757 ) ) ;
#12293 = CARTESIAN_POINT ( 'NONE',  ( 108.0517077545248696, -2.791137627527939813, -18.39754474579286025 ) ) ;
#12294 = EDGE_CURVE ( 'NONE', #24584, #10084, #14593, .T. ) ;
#12295 = VERTEX_POINT ( 'NONE', #23331 ) ;
#12296 = CARTESIAN_POINT ( 'NONE',  ( 119.3198281442452924, 0.5811942927096110934, -14.16772938898807510 ) ) ;
#12297 = LINE ( 'NONE', #19128, #17466 ) ;
#12298 = CARTESIAN_POINT ( 'NONE',  ( 123.3474214775786209, -0.1624402480850797581, -16.17319339645315424 ) ) ;
#12299 = CARTESIAN_POINT ( 'NONE',  ( 114.9518748109119883, -7.643976991954077427, -18.09477374809248928 ) ) ;
#12300 = CARTESIAN_POINT ( 'NONE',  ( 116.1657942554890752, -2.372251574601226043, -17.96033910819752322 ) ) ;
#12301 = DIRECTION ( 'NONE',  ( -0.000000000000000000, -0.3818493186865928313, 0.9242245927363027524 ) ) ;
#12302 = CARTESIAN_POINT ( 'NONE',  ( 113.3068014775786594, -8.166667518702817929, -8.995218007635859436 ) ) ;
#12303 = EDGE_CURVE ( 'NONE', #21214, #39653, #19914, .T. ) ;
#12304 = CARTESIAN_POINT ( 'NONE',  ( 112.7050671295247923, 0.1403307496149613920, -13.39321520033831447 ) ) ;
#12305 = ADVANCED_FACE ( 'NONE', ( #13530 ), #17176, .T. ) ;
#12306 = CARTESIAN_POINT ( 'NONE',  ( 124.4819548109119722, -7.893985811506177619, -18.51759400769804742 ) ) ;
#12307 = DIRECTION ( 'NONE',  ( -0.000000000000000000, -0.9284778069183718952, -0.3713878862591649677 ) ) ;
#12308 = EDGE_LOOP ( 'NONE', ( #30166, #18888, #31604, #10931 ) ) ;
#12309 = EDGE_CURVE ( 'NONE', #5970, #12356, #30400, .T. ) ;
#12310 = CARTESIAN_POINT ( 'NONE',  ( 113.1933481442453058, -4.089484607189486809, -7.948022111789456723 ) ) ;
#12311 = CARTESIAN_POINT ( 'NONE',  ( 113.5904348109119866, -2.084020599724406786, -8.691656652584148546 ) ) ;
#12312 = CARTESIAN_POINT ( 'NONE',  ( 120.2542535264548889, -8.247323210606168686, -17.08054893949881148 ) ) ;
#12313 = CARTESIAN_POINT ( 'NONE',  ( 113.7038881442453402, -3.383040157471821630, -19.15922257007629170 ) ) ;
#12314 = ORIENTED_EDGE ( 'NONE', *, *, #935, .T. ) ;
#12315 = CARTESIAN_POINT ( 'NONE',  ( 116.3133148109119759, -7.893985811506177619, -18.51759400769804742 ) ) ;
#12316 = CARTESIAN_POINT ( 'NONE',  ( 90.20794100481921873, -11.57440209418094668, -18.64321520033831803 ) ) ;
#12317 = DIRECTION ( 'NONE',  ( 0.000000000000000000, -0.9242245927363028635, -0.3818493186865930533 ) ) ;
#12318 = CARTESIAN_POINT ( 'NONE',  ( 123.6089988258993202, -4.390761125357079742, -15.27237650495351495 ) ) ;
#12319 = CARTESIAN_POINT ( 'NONE',  ( 113.1366214775786432, -7.643976991954077427, -18.09477374809248928 ) ) ;
#12320 = PLANE ( 'NONE',  #5875 ) ;
#12321 = CARTESIAN_POINT ( 'NONE',  ( 124.9764995119678730, -3.726932892905140182, -20.90982082926597840 ) ) ;
#12322 = CARTESIAN_POINT ( 'NONE',  ( 111.3213681442453264, -7.643976991954077427, -18.09477374809248928 ) ) ;
#12323 = CARTESIAN_POINT ( 'NONE',  ( 125.5597614775786326, -7.894159318335828068, -9.358103419637847864 ) ) ;
#12324 = CARTESIAN_POINT ( 'NONE',  ( 120.0907204359119760, 1.345710702986147034, -13.97328579221134426 ) ) ;
#12325 = AXIS2_PLACEMENT_3D ( 'NONE', #13573, #24066, #21071 ) ;
#12326 = CARTESIAN_POINT ( 'NONE',  ( 113.4769814775786330, -10.63000616557722466, -14.87417383870573495 ) ) ;
#12327 = CARTESIAN_POINT ( 'NONE',  ( 112.4559014775786778, -0.1624402480850797581, -16.17319339645315424 ) ) ;
#12328 = CARTESIAN_POINT ( 'NONE',  ( 122.9503348109119827, 0.5811942927096110934, -14.16772938898807510 ) ) ;
#12329 = CARTESIAN_POINT ( 'NONE',  ( 122.7801548109119665, -3.383040157471821630, -19.15922257007629170 ) ) ;
#12330 = ORIENTED_EDGE ( 'NONE', *, *, #2358, .T. ) ;
#12331 = CARTESIAN_POINT ( 'NONE',  ( 127.3669547543382379, -8.461095036548107018, -17.65169866057126313 ) ) ;
#12332 = CARTESIAN_POINT ( 'NONE',  ( 110.1353015045248469, -2.477300249445798297, -7.631215200338321125 ) ) ;
#12333 = CARTESIAN_POINT ( 'NONE',  ( 111.4549108795247747, -1.325403438956436419, -16.93181055722141792 ) ) ;
#12334 = CARTESIAN_POINT ( 'NONE',  ( 107.3571765045248299, -2.791137627527939813, -8.388885654883777576 ) ) ;
#12335 = CARTESIAN_POINT ( 'NONE',  ( 71.02242295334774269, -50.41057895470540728, -36.47187266147894746 ) ) ;
#12336 = CARTESIAN_POINT ( 'NONE',  ( 115.6893214775786447, 0.5811942927096154232, -14.16772938898807155 ) ) ;
#12337 = EDGE_LOOP ( 'NONE', ( #27396, #29829, #4098, #38717, #35825, #35250, #41670, #27463, #17682, #9145, #16580 ) ) ;
#12338 = CARTESIAN_POINT ( 'NONE',  ( 124.3522778485100702, -9.656977264654683424, -19.75004840186534949 ) ) ;
#12339 = CARTESIAN_POINT ( 'NONE',  ( 124.2579079359119731, -4.360204210389825086, -8.000047426360248792 ) ) ;
#12340 = DIRECTION ( 'NONE',  ( 0.000000000000000000, 0.000000000000000000, 1.000000000000000000 ) ) ;
#12341 = B_SPLINE_CURVE_WITH_KNOTS ( 'NONE', 3,
 ( #10382, #34524, #10162, #3301 ),
 .UNSPECIFIED., .F., .F.,
 ( 4, 4 ),
 ( 0.000000000000000000, 1.000000000000000000 ),
 .UNSPECIFIED. ) ;
#12342 = CARTESIAN_POINT ( 'NONE',  ( 112.6828081442453282, -2.084020599724406786, -8.691656652584148546 ) ) ;
#12343 = EDGE_CURVE ( 'NONE', #21853, #40407, #15340, .T. ) ;
#12344 = CARTESIAN_POINT ( 'NONE',  ( 120.9081748109119872, -5.638512984488999180, -18.83840828888717311 ) ) ;
#12345 = CARTESIAN_POINT ( 'NONE',  ( 110.8298327545248299, -2.477300249445798297, -19.15521520033831138 ) ) ;
#12346 = LINE ( 'NONE', #36936, #32981 ) ;
#12347 = VERTEX_POINT ( 'NONE', #20370 ) ;
#12348 = CARTESIAN_POINT ( 'NONE',  ( 110.8068531537514758, 0.4930828106259610433, -14.64321520033834645 ) ) ;
#12349 = CARTESIAN_POINT ( 'NONE',  ( 120.5110881442453206, -3.505236298600246325, -18.68346056562440793 ) ) ;
#12350 = CARTESIAN_POINT ( 'NONE',  ( 118.5256548109119876, -0.4660016031367893996, -10.09054647747474043 ) ) ;
#12351 = CARTESIAN_POINT ( 'NONE',  ( 114.8384214775786489, -10.15424416112533912, -14.75197769757731336 ) ) ;
#12352 = CARTESIAN_POINT ( 'NONE',  ( 113.9875214775786532, -0.4660016031367893996, -10.09054647747474043 ) ) ;
#12353 = DIRECTION ( 'NONE',  ( 0.000000000000000000, 0.9242245927363034186, 0.3818493186865916655 ) ) ;
#12354 = CARTESIAN_POINT ( 'NONE',  ( 123.8579614775786126, -9.859900752359378018, -12.68260735090039759 ) ) ;
#12355 = CARTESIAN_POINT ( 'NONE',  ( 120.1140014775786398, -7.894159318335828068, -9.358103419637847864 ) ) ;
#12356 = VERTEX_POINT ( 'NONE', #6227 ) ;
#12357 = CARTESIAN_POINT ( 'NONE',  ( 123.7717360609119623, -6.564341423271550902, -7.887810678476487425 ) ) ;
#12358 = ADVANCED_FACE ( 'NONE', ( #26978 ), #40898, .T. ) ;
#12359 = VECTOR ( 'NONE', #38787, 1000.000000000000000 ) ;
#12360 = CARTESIAN_POINT ( 'NONE',  ( 112.5693548109119888, -10.63000616557722466, -14.87417383870573495 ) ) ;
#12361 = CARTESIAN_POINT ( 'NONE',  ( 121.8725281442453223, -6.222761293078241884, -8.102969835052219238 ) ) ;
#12362 = EDGE_LOOP ( 'NONE', ( #4780, #40621, #13263, #39241, #7111, #12809 ) ) ;
#12363 = CONICAL_SURFACE ( 'NONE', #18179, 2.999999999999999556, 0.9599310885968830309 ) ;
#12364 = CARTESIAN_POINT ( 'NONE',  ( 122.0354079359119908, -4.360204210389833968, -8.000047426360245240 ) ) ;
#12365 = CARTESIAN_POINT ( 'NONE',  ( 113.7606148109119886, -1.561330072975668060, -17.79121239304076596 ) ) ;
#12366 = CARTESIAN_POINT ( 'NONE',  ( 110.2047546295247855, -4.863998795839590272, -7.631215200338315796 ) ) ;
#12367 = CARTESIAN_POINT ( 'NONE',  ( 116.7104014775786425, -8.899110576539710493, -16.42337572283490132 ) ) ;
#12368 = ORIENTED_EDGE ( 'NONE', *, *, #15250, .T. ) ;
#12369 = ORIENTED_EDGE ( 'NONE', *, *, #1596, .F. ) ;
#12370 = CARTESIAN_POINT ( 'NONE',  ( 122.8936081442453059, -9.565557343593413364, -10.61323700422348004 ) ) ;
#12371 = CARTESIAN_POINT ( 'NONE',  ( 120.0005481442453146, -4.153390946401325223, -8.397313243818185668 ) ) ;
#12372 = VECTOR ( 'NONE', #25165, 1000.000000000000000 ) ;
#12373 = CARTESIAN_POINT ( 'NONE',  ( 66.31928500851137187, -14.71576354012722021, -16.39321520033831447 ) ) ;
#12374 = CARTESIAN_POINT ( 'NONE',  ( 62.33173950417162246, -36.13435100893377694, -5.771259754798731656 ) ) ;
#12375 = AXIS2_PLACEMENT_3D ( 'NONE', #42185, #21649, #10727 ) ;
#12376 = DIRECTION ( 'NONE',  ( 0.9609149988134837450, -0.1028163501681639419, 0.2570431154366518145 ) ) ;
#12377 = DIRECTION ( 'NONE',  ( -0.000000000000000000, -0.9284778069183718952, -0.3713878862591649677 ) ) ;
#12378 = CARTESIAN_POINT ( 'NONE',  ( 119.3765548109119834, 0.9020085738987339008, -11.91225656197089222 ) ) ;
#12379 = CARTESIAN_POINT ( 'NONE',  ( 107.2182702545248105, -10.62599879583958717, -15.77991374673208469 ) ) ;
#12380 = EDGE_CURVE ( 'NONE', #41822, #18421, #10246, .T. ) ;
#12381 = CARTESIAN_POINT ( 'NONE',  ( 114.7816948109119863, 0.5811942927096154232, -14.16772938898807155 ) ) ;
#12383 = CARTESIAN_POINT ( 'NONE',  ( 117.7314814775786260, -5.574606645277164318, -18.38911715685844683 ) ) ;
#12382 = CARTESIAN_POINT ( 'NONE',  ( 116.0864081442453113, -9.988377603198976828, -10.36322818467138340 ) ) ;
#12384 = CARTESIAN_POINT ( 'NONE',  ( 120.6245414775786458, -0.1624402480850797581, -16.17319339645315424 ) ) ;
#12385 = CARTESIAN_POINT ( 'NONE',  ( 113.3068014775786594, -8.166667518702817929, -8.995218007635859436 ) ) ;
#12386 = ORIENTED_EDGE ( 'NONE', *, *, #40719, .T. ) ;
#12387 = CARTESIAN_POINT ( 'NONE',  ( 119.1496481442453046, -6.222761293078241884, -8.102969835052219238 ) ) ;
#12388 = DIRECTION ( 'NONE',  ( 0.000000000000000000, 0.6004852223388321697, -0.7996358532186279566 ) ) ;
#12389 = CARTESIAN_POINT ( 'NONE',  ( 113.7468640045248236, -10.62599879583958717, -11.00651665394454604 ) ) ;
#12390 = CARTESIAN_POINT ( 'NONE',  ( 89.40092984481313465, -25.99489077589524300, -13.39321520033831625 ) ) ;
#12391 = CARTESIAN_POINT ( 'NONE',  ( 113.3995983795247895, -0.7896495226426338832, -9.318865927141430916 ) ) ;
#12392 = CARTESIAN_POINT ( 'NONE',  ( 118.3554748109119998, 0.2603800115204892296, -16.42320221600525088 ) ) ;
#12393 = VERTEX_POINT ( 'NONE', #34257 ) ;
#12394 = CARTESIAN_POINT ( 'NONE',  ( 120.6245414775786458, -9.988377603198976828, -10.36322818467138340 ) ) ;
#12395 = CARTESIAN_POINT ( 'NONE',  ( 62.81996251504057227, -37.57851814417504954, -5.091777875131382913 ) ) ;
#12396 = CARTESIAN_POINT ( 'NONE',  ( 108.7462390045248242, 0.8980012041604421569, -15.77991374673208469 ) ) ;
#12397 = CARTESIAN_POINT ( 'NONE',  ( 118.5823814775786360, -1.834011780172310813, -8.268836392978581529 ) ) ;
#12398 = CARTESIAN_POINT ( 'NONE',  ( 117.2776681442452968, -5.638512984488999180, -18.83840828888717311 ) ) ;
#12399 = CARTESIAN_POINT ( 'NONE',  ( 64.53406607755297841, -2.730567333127841501, -18.66298557222672727 ) ) ;
#12400 = CARTESIAN_POINT ( 'NONE',  ( 116.9757267558744047, -11.53487629098437317, -5.866158325263667095 ) ) ;
#12401 = ORIENTED_EDGE ( 'NONE', *, *, #527, .T. ) ;
#12402 = CARTESIAN_POINT ( 'NONE',  ( 75.95778847736481509, -3.256761025687722189, -18.64321520033831803 ) ) ;
#12403 = CARTESIAN_POINT ( 'NONE',  ( 109.2294499582155396, -8.941328865127285752, -16.92711395088718263 ) ) ;
#12404 = CARTESIAN_POINT ( 'NONE',  ( 121.4187148109119789, -3.505236298600246325, -18.68346056562440793 ) ) ;
#12405 = CARTESIAN_POINT ( 'NONE',  ( 110.5520202545248054, 0.1403307496149616695, -11.32035403202665336 ) ) ;
#12406 = CARTESIAN_POINT ( 'NONE',  ( 110.2742077545248094, -2.791137627527939813, -18.39754474579286025 ) ) ;
#12407 = AXIS2_PLACEMENT_3D ( 'NONE', #39456, #8219, #4787 ) ;
#12408 = CARTESIAN_POINT ( 'NONE',  ( 119.2631014775786298, -9.565557343593413364, -10.61323700422348004 ) ) ;
#12409 = FACE_OUTER_BOUND ( 'NONE', #24854, .T. ) ;
#12410 = CARTESIAN_POINT ( 'NONE',  ( 68.94757123365556595, -25.85038639872388799, -5.893215200338315363 ) ) ;
#12411 = CARTESIAN_POINT ( 'NONE',  ( 125.7866681442452688, -0.4660016031367893996, -10.09054647747474043 ) ) ;
#12412 = CARTESIAN_POINT ( 'NONE',  ( 124.9357681442453014, -1.834011780172310813, -8.268836392978581529 ) ) ;
#12413 = ORIENTED_EDGE ( 'NONE', *, *, #15719, .T. ) ;
#12414 = CARTESIAN_POINT ( 'NONE',  ( 118.8660148109119774, 0.1319031606808879209, -14.10382304977623669 ) ) ;
#12415 = CARTESIAN_POINT ( 'NONE',  ( 114.7816948109119863, 0.5811942927096154232, -14.16772938898807155 ) ) ;
#12416 = CARTESIAN_POINT ( 'NONE',  ( 121.4187148109119789, -6.344957434206665248, -7.627207830600338134 ) ) ;
#12417 = ADVANCED_FACE ( 'NONE', ( #10116 ), #38130, .F. ) ;
#12418 = CARTESIAN_POINT ( 'NONE',  ( 121.8158014775786171, -4.153390946401325223, -8.397313243818185668 ) ) ;
#12419 = EDGE_LOOP ( 'NONE', ( #40291, #15776, #19345, #13720, #7130, #30883 ) ) ;
#12420 = CARTESIAN_POINT ( 'NONE',  ( 124.0848681442452772, -5.574606645277164318, -18.38911715685844683 ) ) ;
#12421 = CARTESIAN_POINT ( 'NONE',  ( 123.5176014775786228, -9.261995988541697145, -16.69588392320189030 ) ) ;
#12422 = AXIS2_PLACEMENT_3D ( 'NONE', #45095, #13852, #17718 ) ;
#12423 = CARTESIAN_POINT ( 'NONE',  ( 124.4646854081441631, -8.458298358070186040, -6.340390706684574162 ) ) ;
#12424 = CARTESIAN_POINT ( 'NONE',  ( 124.7088614775786226, 0.2603800115204892296, -16.42320221600525088 ) ) ;
#12425 = CARTESIAN_POINT ( 'NONE',  ( 105.6208483795248299, -0.7896495226426338832, -9.318865927141430916 ) ) ;
#12426 = CARTESIAN_POINT ( 'NONE',  ( 94.20708369096698220, -26.42437990495228917, -14.12788525418686270 ) ) ;
#12427 = FACE_OUTER_BOUND ( 'NONE', #8808, .T. ) ;
#12428 = CARTESIAN_POINT ( 'NONE',  ( 110.8298327545248299, -6.936859964151250502, -8.388885654883777576 ) ) ;
#12429 = AXIS2_PLACEMENT_3D ( 'NONE', #12690, #18841, #22042 ) ;
#12430 = CARTESIAN_POINT ( 'NONE',  ( 122.7299391859119737, -1.406689858478933353, -17.56299727309130887 ) ) ;
#12431 = AXIS2_PLACEMENT_3D ( 'NONE', #1723, #8579, #39367 ) ;
#12432 = CARTESIAN_POINT ( 'NONE',  ( 137.0134976903310644, -9.992782420886062056, -11.53748965989417385 ) ) ;
#12433 = CARTESIAN_POINT ( 'NONE',  ( 120.5110881442453206, -3.505236298600246325, -18.68346056562440793 ) ) ;
#12434 = CARTESIAN_POINT ( 'NONE',  ( 123.6877814775786533, -3.383040157471821630, -19.15922257007629170 ) ) ;
#12435 = CARTESIAN_POINT ( 'NONE',  ( 61.69189222814998175, -49.76310523276723785, -4.893215200338314474 ) ) ;
#12436 = ORIENTED_EDGE ( 'NONE', *, *, #24741, .T. ) ;
#12437 = CARTESIAN_POINT ( 'NONE',  ( 116.0086969107182142, -2.467220198592777525, -17.83387418641524391 ) ) ;
#12438 = CARTESIAN_POINT ( 'NONE',  ( 107.8433483795247838, -8.402594152722688392, -16.93181055722141792 ) ) ;
#12439 = CARTESIAN_POINT ( 'NONE',  ( 116.3700414775786527, -4.153390946401321671, -8.397313243818183892 ) ) ;
#12440 = DIRECTION ( 'NONE',  ( 1.000000000000000000, 0.000000000000000000, -0.000000000000000000 ) ) ;
#12441 = CARTESIAN_POINT ( 'NONE',  ( 135.3184548109119874, 1.087851763053662602, -12.63461456455805276 ) ) ;
#12442 = CARTESIAN_POINT ( 'NONE',  ( 122.7177766009169204, -8.403782945130243931, -17.37684090985457885 ) ) ;
#12444 = CARTESIAN_POINT ( 'NONE',  ( 122.7801548109119665, -3.383040157471821630, -19.15922257007629170 ) ) ;
#12443 = CARTESIAN_POINT ( 'NONE',  ( 113.9552388068194801, 0.1168444861213632779, -12.14321520033831625 ) ) ;
#12445 = CARTESIAN_POINT ( 'NONE',  ( 121.9292548109119849, -7.894159318335828068, -9.358103419637847864 ) ) ;
#12446 = ORIENTED_EDGE ( 'NONE', *, *, #1366, .F. ) ;
#12447 = CARTESIAN_POINT ( 'NONE',  ( 110.2961459279789835, 0.1843591316377651834, -14.64321520033833934 ) ) ;
#12448 = CARTESIAN_POINT ( 'NONE',  ( 72.54180985774836188, -52.30061520688905574, -33.39389990939168484 ) ) ;
#12449 = CARTESIAN_POINT ( 'NONE',  ( 109.0240515045248202, -6.936859964151250502, -18.39754474579286025 ) ) ;
#12450 = CARTESIAN_POINT ( 'NONE',  ( 121.8725281442453223, -6.222761293078241884, -8.102969835052219238 ) ) ;
#12451 = CARTESIAN_POINT ( 'NONE',  ( 121.7023481442452777, -0.8288870151387760510, -10.36305467784173118 ) ) ;
#12452 = CARTESIAN_POINT ( 'NONE',  ( 124.4646854081411362, 2.664654824213256834, -15.83876163224986655 ) ) ;
#12453 = CARTESIAN_POINT ( 'NONE',  ( 110.4131140045248287, -10.62599879583958717, -11.00651665394454604 ) ) ;
#12454 = CARTESIAN_POINT ( 'NONE',  ( 116.5509091406318873, 0.3208234527006367798, -15.99825685930877839 ) ) ;
#12455 = DIRECTION ( 'NONE',  ( -0.3127730236694426513, 0.9498278979187093629, 0.000000000000000000 ) ) ;
#12456 = AXIS2_PLACEMENT_3D ( 'NONE', #18335, #15984, #15140 ) ;
#12457 = LINE ( 'NONE', #15645, #24096 ) ;
#12458 = CARTESIAN_POINT ( 'NONE',  ( 112.7745202545247878, -10.62599879583958717, -15.77991374673208469 ) ) ;
#12459 = CARTESIAN_POINT ( 'NONE',  ( -13.00223655648873589, -4.133127502629707628, -19.24873805723332865 ) ) ;
#12460 = CARTESIAN_POINT ( 'NONE',  ( 115.8999108795247821, -8.938348069036489818, -9.318865927141430916 ) ) ;
#12461 = CARTESIAN_POINT ( 'NONE',  ( 121.8158014775786171, -5.638512984488999180, -18.83840828888717311 ) ) ;
#12462 = CARTESIAN_POINT ( 'NONE',  ( 121.2485348109119769, -0.4660016031367893996, -10.09054647747474043 ) ) ;
#12463 = CARTESIAN_POINT ( 'NONE',  ( 121.9470836909669913, -24.14644159042263993, -12.62951656296512937 ) ) ;
#12464 =( BOUNDED_SURFACE ( )  B_SPLINE_SURFACE ( 1, 2, ( 
 ( #9508, #37310, #40988, #9287, #26838, #16815, #12710, #20230, #26610, #30707, #12941, #16352, #6077, #19999, #33883, #30479, #44400, #13164, #6311, #44630, #13394, #27297, #38874, #34982, #359, #3768, #32033, #3552, #11077, #7195, #10633, #45068, #31365, #14720, #17692, #583, #7644, #42094, #17467, #24980, #802, #31589, #25210, #38641, #27743, #39108, #38427, #4221, #28407, #14270, #6986, #41657, #14492, #38208, #13828, #3992, #17914, #137, #10416, #21105, #24538, #14050, #20898, #24323, #21557, #10857, #31812, #28633, #42540, #3339, #20678, #21334, #28188, #35446, #34772, #24753, #7413, #27966, #35219, #11301, #42316, #34555, #41873, #18137, #17258, #31147, #22851, #19429, #15165, #4450, #13051, #1028, #36961, #11530, #18371, #29070, #33314, #26950, #12830, #19887, #14945, #9173, #35902, #26729, #25436, #37188, #7877, #8950, #23081, #36742, #28855, #35675, #40639, #33774, #40184, #5510, #42768, #32260, #9394, #2544, #2089, #16015, #18589, #16246, #30149, #29921, #4667, #21785, #26505, #39338, #5962, #44064, #23305, #16471, #42982, #12378, #43836, #8105, #1254, #5733, #30374, #40414, #22006, #19652, #32479, #44295, #26276, #12604, #33538, #2316, #30821, #13504, #6435, #9624, #34229, #41765, #13943, #10090, #20567, #23994, #7093, #23770, #31258, #27410, #44744, #20120, #20346, #34878, #37882, #20786, #27855, #17151, #37662, #31, #21003, #6656, #250, #13726, #2775, #14158, #41332, #24425, #3453, #34445, #27182, #16700, #34666, #13276, #34006, #24210, #38103, #3003, #30595, #3225, #31039, #16926, #41103, #44512, #10526, #44969, #6877, #3666, #17586, #23546, #40871, #41549, #27635, #38316, #9861, #10309, #17369, #31479, #37429, #6199, #21896, #28077, #7308, #28748, #32149, #3887, #42432, #38996, #35334, #24647, #32597, #21226, #11423, #31700, #38533, #4104, #7765, #1368, #32376, #39455, #35104, #42652, #10969, #1142, #470, #11636, #41984, #28527, #25330, #11196, #17807, #24871, #10750, #25549, #14384, #25100, #28296, #21673, #689, #7987, #8218, #18706, #35561 ),
 ( #42207, #39222, #919, #38763, #4334, #18255, #18027, #7533, #21451, #31924, #35790, #14608, #14838, #4560, #18486, #15059, #28974, #22124, #42878, #36018, #4786, #19598, #32814, #44009, #15278, #15734, #29864, #29636, #8444, #43098, #33482, #26671, #1808, #12319, #25998, #23019, #36908, #43551, #12093, #29186, #33263, #11868, #12771, #5680, #2261, #16188, #22565, #36469, #22790, #22348, #8663, #43780, #30093, #2035, #25773, #12544, #39902, #40584, #36242, #9343, #23252, #1582, #5235, #33033, #19150, #39679, #26218, #37134, #5910, #40128, #8892, #36684, #19831, #43326, #33718, #5455, #19374, #5008, #15961, #18925, #26451, #40354, #15504, #9117, #29412, #38051, #27798, #30766, #7044, #20515, #9571, #20956, #20288, #31208, #10252, #44690, #33950, #23487, #41496, #20065, #40815, #30991, #44916, #13225, #26895, #34172, #6380, #41712, #16875, #27581, #34614, #23943, #30537, #6829, #10476, #13451, #2489, #34394, #37373, #16418, #2946, #45131, #24160, #27356, #2718, #6144, #20734, #16644, #44459, #13673, #3401, #27125, #41049, #41275, #10035, #9806, #23716, #37606, #17319, #37822, #13890, #24377, #38264, #30313, #44239, #3176, #6600, #12999, #17098, #31875, #640, #24598, #21396, #25498, #28697, #34828, #14108, #35509, #38939, #10695, #4051, #14553, #42156, #31426, #39402, #28024, #18199, #38482, #192, #10916, #28472, #8167, #39170, #1091, #41932, #4281, #17751, #7934, #7256, #18436, #3611, #35276, #32095, #17974, #21171, #17528, #21844, #15007, #42378, #11141, #417, #42602, #11367, #25044, #31647, #35048, #7707, #3831, #32326, #25273, #35739, #4512, #24816, #38708, #21620, #14333, #28247, #865, #28920, #14783, #7476, #42828, #11589, #5627, #43046, #19548, #43725, #39628, #12041, #39851, #32761, #35965, #15456, #22966, #40301, #36410, #1757, #5178, #33426, #4957, #12493, #8616, #25945, #1316, #1534, #22514, #29362, #22296, #29134, #26392, #43502, #5409, #16132, #43951, #4735, #22074, #22735, #19096, #9065, #25722, #32982, #15682, #11814, #29585, #12715, #15912, #18654 ) ),
 .UNSPECIFIED., .F., .F., .T. ) 
 B_SPLINE_SURFACE_WITH_KNOTS ( ( 2, 2 ),
 ( 3, 2, 2, 2, 2, 2, 2, 2, 2, 2, 2, 2, 2, 2, 2, 2, 2, 2, 2, 2, 2, 2, 2, 2, 2, 2, 2, 2, 2, 2, 2, 2, 2, 2, 2, 2, 2, 2, 2, 2, 2, 2, 2, 2, 2, 2, 2, 2, 2, 2, 2, 2, 2, 2, 2, 2, 2, 2, 2, 2, 2, 2, 2, 2, 2, 2, 2, 2, 2, 2, 2, 2, 2, 2, 2, 2, 2, 2, 2, 2, 2, 2, 2, 2, 2, 2, 2, 2, 2, 2, 2, 2, 2, 2, 2, 2, 2, 2, 2, 2, 2, 2, 2, 2, 2, 2, 2, 2, 2, 2, 2, 2, 2, 2, 2, 2, 2, 2, 2, 2, 2, 2, 2, 2, 2, 2, 2, 2, 3 ),
 ( 0.000000000000000000, 1.000000000000000000 ),
 ( 0.000000000000000000, 0.007812500000000000000, 0.01562500000000000000, 0.02343750000000000000, 0.03125000000000000000, 0.03906250000000000000, 0.04687500000000000000, 0.05468750000000000000, 0.06250000000000000000, 0.07031250000000000000, 0.07812500000000000000, 0.08593750000000000000, 0.09375000000000000000, 0.1015625000000000000, 0.1093750000000000000, 0.1171875000000000000, 0.1250000000000000000, 0.1328125000000000000, 0.1406250000000000000, 0.1484375000000000000, 0.1562500000000000000, 0.1640625000000000000, 0.1718750000000000000, 0.1796875000000000000, 0.1875000000000000000, 0.1953125000000000000, 0.2031250000000000000, 0.2109375000000000000, 0.2187500000000000000, 0.2265625000000000000, 0.2343750000000000000, 0.2421875000000000000, 0.2500000000000000000, 0.2578125000000000000, 0.2656250000000000000, 0.2734375000000000000, 0.2812500000000000000, 0.2890625000000000000, 0.2968750000000000000, 0.3046875000000000000, 0.3125000000000000000, 0.3203125000000000000, 0.3281250000000000000, 0.3359375000000000000, 0.3437500000000000000, 0.3515625000000000000, 0.3593750000000000000, 0.3671875000000000000, 0.3750000000000000000, 0.3828125000000000000, 0.3906250000000000000, 0.3984375000000000000, 0.4062500000000000000, 0.4140625000000000000, 0.4218750000000000000, 0.4296875000000000000, 0.4375000000000000000, 0.4453125000000000000, 0.4531250000000000000, 0.4609375000000000000, 0.4687500000000000000, 0.4765625000000000000, 0.4843750000000000000, 0.4921875000000000000, 0.5000000000000000000, 0.5078125000000000000, 0.5156250000000000000, 0.5234375000000000000, 0.5312500000000000000, 0.5390625000000000000, 0.5468750000000000000, 0.5546875000000000000, 0.5625000000000000000, 0.5703125000000000000, 0.5781250000000000000, 0.5859375000000000000, 0.5937500000000000000, 0.6015625000000000000, 0.6093750000000000000, 0.6171875000000000000, 0.6250000000000000000, 0.6328125000000000000, 0.6406250000000000000, 0.6484375000000000000, 0.6562500000000000000, 0.6640625000000000000, 0.6718750000000000000, 0.6796875000000000000, 0.6875000000000000000, 0.6953125000000000000, 0.7031250000000000000, 0.7109375000000000000, 0.7187500000000000000, 0.7265625000000000000, 0.7343750000000000000, 0.7421875000000000000, 0.7500000000000000000, 0.7578125000000000000, 0.7656250000000000000, 0.7734375000000000000, 0.7812500000000000000, 0.7890625000000000000, 0.7968750000000000000, 0.8046875000000000000, 0.8125000000000000000, 0.8203125000000000000, 0.8281250000000000000, 0.8359375000000000000, 0.8437500000000000000, 0.8515625000000000000, 0.8593750000000000000, 0.8671875000000000000, 0.8750000000000000000, 0.8828125000000000000, 0.8906250000000000000, 0.8984375000000000000, 0.9062500000000000000, 0.9140625000000000000, 0.9218750000000000000, 0.9296875000000000000, 0.9375000000000000000, 0.9453125000000000000, 0.9531250000000000000, 0.9609375000000000000, 0.9687500000000000000, 0.9765625000000000000, 0.9843750000000000000, 0.9921875000000000000, 1.000000000000000000 ),
 .UNSPECIFIED. ) 
 GEOMETRIC_REPRESENTATION_ITEM ( )  RATIONAL_B_SPLINE_SURFACE ( (
 ( 1.000000000000000000, 0.9238795325112869605, 1.000000000000000000, 0.9238795325112869605, 1.000000000000000000, 0.9238795325112869605, 1.000000000000000000, 0.9238795325112869605, 1.000000000000000000, 0.9238795325112869605, 1.000000000000000000, 0.9238795325112869605, 1.000000000000000000, 0.9238795325112869605, 1.000000000000000000, 0.9238795325112869605, 1.000000000000000000, 0.9238795325112869605, 1.000000000000000000, 0.9238795325112869605, 1.000000000000000000, 0.9238795325112869605, 1.000000000000000000, 0.9238795325112869605, 1.000000000000000000, 0.9238795325112869605, 1.000000000000000000, 0.9238795325112869605, 1.000000000000000000, 0.9238795325112869605, 1.000000000000000000, 0.9238795325112869605, 1.000000000000000000, 0.9238795325112869605, 1.000000000000000000, 0.9238795325112869605, 1.000000000000000000, 0.9238795325112869605, 1.000000000000000000, 0.9238795325112869605, 1.000000000000000000, 0.9238795325112869605, 1.000000000000000000, 0.9238795325112869605, 1.000000000000000000, 0.9238795325112869605, 1.000000000000000000, 0.9238795325112869605, 1.000000000000000000, 0.9238795325112869605, 1.000000000000000000, 0.9238795325112869605, 1.000000000000000000, 0.9238795325112869605, 1.000000000000000000, 0.9238795325112869605, 1.000000000000000000, 0.9238795325112869605, 1.000000000000000000, 0.9238795325112869605, 1.000000000000000000, 0.9238795325112869605, 1.000000000000000000, 0.9238795325112869605, 1.000000000000000000, 0.9238795325112869605, 1.000000000000000000, 0.9238795325112869605, 1.000000000000000000, 0.9238795325112869605, 1.000000000000000000, 0.9238795325112869605, 1.000000000000000000, 0.9238795325112869605, 1.000000000000000000, 0.9238795325112869605, 1.000000000000000000, 0.9238795325112869605, 1.000000000000000000, 0.9238795325112869605, 1.000000000000000000, 0.9238795325112869605, 1.000000000000000000, 0.9238795325112869605, 1.000000000000000000, 0.9238795325112869605, 1.000000000000000000, 0.9238795325112869605, 1.000000000000000000, 0.9238795325112869605, 1.000000000000000000, 0.9238795325112869605, 1.000000000000000000, 0.9238795325112869605, 1.000000000000000000, 0.9238795325112869605, 1.000000000000000000, 0.9238795325112869605, 1.000000000000000000, 0.9238795325112869605, 1.000000000000000000, 0.9238795325112869605, 1.000000000000000000, 0.9238795325112869605, 1.000000000000000000, 0.9238795325112869605, 1.000000000000000000, 0.9238795325112869605, 1.000000000000000000, 0.9238795325112869605, 1.000000000000000000, 0.9238795325112869605, 1.000000000000000000, 0.9238795325112869605, 1.000000000000000000, 0.9238795325112869605, 1.000000000000000000, 0.9238795325112869605, 1.000000000000000000, 0.9238795325112869605, 1.000000000000000000, 0.9238795325112869605, 1.000000000000000000, 0.9238795325112869605, 1.000000000000000000, 0.9238795325112869605, 1.000000000000000000, 0.9238795325112869605, 1.000000000000000000, 0.9238795325112869605, 1.000000000000000000, 0.9238795325112869605, 1.000000000000000000, 0.9238795325112869605, 1.000000000000000000, 0.9238795325112869605, 1.000000000000000000, 0.9238795325112869605, 1.000000000000000000, 0.9238795325112869605, 1.000000000000000000, 0.9238795325112869605, 1.000000000000000000, 0.9238795325112869605, 1.000000000000000000, 0.9238795325112869605, 1.000000000000000000, 0.9238795325112869605, 1.000000000000000000, 0.9238795325112869605, 1.000000000000000000, 0.9238795325112869605, 1.000000000000000000, 0.9238795325112869605, 1.000000000000000000, 0.9238795325112869605, 1.000000000000000000, 0.9238795325112869605, 1.000000000000000000, 0.9238795325112869605, 1.000000000000000000, 0.9238795325112869605, 1.000000000000000000, 0.9238795325112869605, 1.000000000000000000, 0.9238795325112869605, 1.000000000000000000, 0.9238795325112869605, 1.000000000000000000, 0.9238795325112869605, 1.000000000000000000, 0.9238795325112869605, 1.000000000000000000, 0.9238795325112869605, 1.000000000000000000, 0.9238795325112869605, 1.000000000000000000, 0.9238795325112869605, 1.000000000000000000, 0.9238795325112869605, 1.000000000000000000, 0.9238795325112869605, 1.000000000000000000, 0.9238795325112869605, 1.000000000000000000, 0.9238795325112869605, 1.000000000000000000, 0.9238795325112869605, 1.000000000000000000, 0.9238795325112869605, 1.000000000000000000, 0.9238795325112869605, 1.000000000000000000, 0.9238795325112869605, 1.000000000000000000, 0.9238795325112869605, 1.000000000000000000, 0.9238795325112869605, 1.000000000000000000, 0.9238795325112869605, 1.000000000000000000, 0.9238795325112869605, 1.000000000000000000, 0.9238795325112869605, 1.000000000000000000, 0.9238795325112869605, 1.000000000000000000, 0.9238795325112869605, 1.000000000000000000, 0.9238795325112869605, 1.000000000000000000, 0.9238795325112869605, 1.000000000000000000, 0.9238795325112869605, 1.000000000000000000, 0.9238795325112869605, 1.000000000000000000, 0.9238795325112869605, 1.000000000000000000, 0.9238795325112869605, 1.000000000000000000, 0.9238795325112869605, 1.000000000000000000, 0.9238795325112869605, 1.000000000000000000, 0.9238795325112869605, 1.000000000000000000, 0.9238795325112869605, 1.000000000000000000, 0.9238795325112869605, 1.000000000000000000, 0.9238795325112869605, 1.000000000000000000, 0.9238795325112869605, 1.000000000000000000, 0.9238795325112869605, 1.000000000000000000, 0.9238795325112869605, 1.000000000000000000, 0.9238795325112869605, 1.000000000000000000, 0.9238795325112869605, 1.000000000000000000, 0.9238795325112869605, 1.000000000000000000, 0.9238795325112869605, 1.000000000000000000, 0.9238795325112869605, 1.000000000000000000, 0.9238795325112869605, 1.000000000000000000, 0.9238795325112869605, 1.000000000000000000, 0.9238795325112869605, 1.000000000000000000, 0.9238795325112869605, 1.000000000000000000),
 ( 1.000000000000000000, 0.9238795325112869605, 1.000000000000000000, 0.9238795325112869605, 1.000000000000000000, 0.9238795325112869605, 1.000000000000000000, 0.9238795325112869605, 1.000000000000000000, 0.9238795325112869605, 1.000000000000000000, 0.9238795325112869605, 1.000000000000000000, 0.9238795325112869605, 1.000000000000000000, 0.9238795325112869605, 1.000000000000000000, 0.9238795325112869605, 1.000000000000000000, 0.9238795325112869605, 1.000000000000000000, 0.9238795325112869605, 1.000000000000000000, 0.9238795325112869605, 1.000000000000000000, 0.9238795325112869605, 1.000000000000000000, 0.9238795325112869605, 1.000000000000000000, 0.9238795325112869605, 1.000000000000000000, 0.9238795325112869605, 1.000000000000000000, 0.9238795325112869605, 1.000000000000000000, 0.9238795325112869605, 1.000000000000000000, 0.9238795325112869605, 1.000000000000000000, 0.9238795325112869605, 1.000000000000000000, 0.9238795325112869605, 1.000000000000000000, 0.9238795325112869605, 1.000000000000000000, 0.9238795325112869605, 1.000000000000000000, 0.9238795325112869605, 1.000000000000000000, 0.9238795325112869605, 1.000000000000000000, 0.9238795325112869605, 1.000000000000000000, 0.9238795325112869605, 1.000000000000000000, 0.9238795325112869605, 1.000000000000000000, 0.9238795325112869605, 1.000000000000000000, 0.9238795325112869605, 1.000000000000000000, 0.9238795325112869605, 1.000000000000000000, 0.9238795325112869605, 1.000000000000000000, 0.9238795325112869605, 1.000000000000000000, 0.9238795325112869605, 1.000000000000000000, 0.9238795325112869605, 1.000000000000000000, 0.9238795325112869605, 1.000000000000000000, 0.9238795325112869605, 1.000000000000000000, 0.9238795325112869605, 1.000000000000000000, 0.9238795325112869605, 1.000000000000000000, 0.9238795325112869605, 1.000000000000000000, 0.9238795325112869605, 1.000000000000000000, 0.9238795325112869605, 1.000000000000000000, 0.9238795325112869605, 1.000000000000000000, 0.9238795325112869605, 1.000000000000000000, 0.9238795325112869605, 1.000000000000000000, 0.9238795325112869605, 1.000000000000000000, 0.9238795325112869605, 1.000000000000000000, 0.9238795325112869605, 1.000000000000000000, 0.9238795325112869605, 1.000000000000000000, 0.9238795325112869605, 1.000000000000000000, 0.9238795325112869605, 1.000000000000000000, 0.9238795325112869605, 1.000000000000000000, 0.9238795325112869605, 1.000000000000000000, 0.9238795325112869605, 1.000000000000000000, 0.9238795325112869605, 1.000000000000000000, 0.9238795325112869605, 1.000000000000000000, 0.9238795325112869605, 1.000000000000000000, 0.9238795325112869605, 1.000000000000000000, 0.9238795325112869605, 1.000000000000000000, 0.9238795325112869605, 1.000000000000000000, 0.9238795325112869605, 1.000000000000000000, 0.9238795325112869605, 1.000000000000000000, 0.9238795325112869605, 1.000000000000000000, 0.9238795325112869605, 1.000000000000000000, 0.9238795325112869605, 1.000000000000000000, 0.9238795325112869605, 1.000000000000000000, 0.9238795325112869605, 1.000000000000000000, 0.9238795325112869605, 1.000000000000000000, 0.9238795325112869605, 1.000000000000000000, 0.9238795325112869605, 1.000000000000000000, 0.9238795325112869605, 1.000000000000000000, 0.9238795325112869605, 1.000000000000000000, 0.9238795325112869605, 1.000000000000000000, 0.9238795325112869605, 1.000000000000000000, 0.9238795325112869605, 1.000000000000000000, 0.9238795325112869605, 1.000000000000000000, 0.9238795325112869605, 1.000000000000000000, 0.9238795325112869605, 1.000000000000000000, 0.9238795325112869605, 1.000000000000000000, 0.9238795325112869605, 1.000000000000000000, 0.9238795325112869605, 1.000000000000000000, 0.9238795325112869605, 1.000000000000000000, 0.9238795325112869605, 1.000000000000000000, 0.9238795325112869605, 1.000000000000000000, 0.9238795325112869605, 1.000000000000000000, 0.9238795325112869605, 1.000000000000000000, 0.9238795325112869605, 1.000000000000000000, 0.9238795325112869605, 1.000000000000000000, 0.9238795325112869605, 1.000000000000000000, 0.9238795325112869605, 1.000000000000000000, 0.9238795325112869605, 1.000000000000000000, 0.9238795325112869605, 1.000000000000000000, 0.9238795325112869605, 1.000000000000000000, 0.9238795325112869605, 1.000000000000000000, 0.9238795325112869605, 1.000000000000000000, 0.9238795325112869605, 1.000000000000000000, 0.9238795325112869605, 1.000000000000000000, 0.9238795325112869605, 1.000000000000000000, 0.9238795325112869605, 1.000000000000000000, 0.9238795325112869605, 1.000000000000000000, 0.9238795325112869605, 1.000000000000000000, 0.9238795325112869605, 1.000000000000000000, 0.9238795325112869605, 1.000000000000000000, 0.9238795325112869605, 1.000000000000000000, 0.9238795325112869605, 1.000000000000000000, 0.9238795325112869605, 1.000000000000000000, 0.9238795325112869605, 1.000000000000000000, 0.9238795325112869605, 1.000000000000000000, 0.9238795325112869605, 1.000000000000000000, 0.9238795325112869605, 1.000000000000000000, 0.9238795325112869605, 1.000000000000000000, 0.9238795325112869605, 1.000000000000000000, 0.9238795325112869605, 1.000000000000000000, 0.9238795325112869605, 1.000000000000000000, 0.9238795325112869605, 1.000000000000000000, 0.9238795325112869605, 1.000000000000000000, 0.9238795325112869605, 1.000000000000000000, 0.9238795325112869605, 1.000000000000000000, 0.9238795325112869605, 1.000000000000000000, 0.9238795325112869605, 1.000000000000000000, 0.9238795325112869605, 1.000000000000000000, 0.9238795325112869605, 1.000000000000000000, 0.9238795325112869605, 1.000000000000000000, 0.9238795325112869605, 1.000000000000000000, 0.9238795325112869605, 1.000000000000000000, 0.9238795325112869605, 1.000000000000000000, 0.9238795325112869605, 1.000000000000000000, 0.9238795325112869605, 1.000000000000000000) ) ) 
 REPRESENTATION_ITEM ( '' )  SURFACE ( )  );
#12465 = CARTESIAN_POINT ( 'NONE',  ( 115.5758681442453053, -1.561330072975668060, -17.79121239304076951 ) ) ;
#12466 = CYLINDRICAL_SURFACE ( 'NONE', #5370, 1.999999999999998890 ) ;
#12467 = ORIENTED_EDGE ( 'NONE', *, *, #16395, .T. ) ;
#12468 = DIRECTION ( 'NONE',  ( 1.000000000000000000, 0.000000000000000000, 0.000000000000000000 ) ) ;
#12469 = CARTESIAN_POINT ( 'NONE',  ( 120.9649014775786355, -3.383040157471821630, -19.15922257007629170 ) ) ;
#12470 = CARTESIAN_POINT ( 'NONE',  ( 118.6391081442452986, -4.089484607189486809, -7.948022111789456723 ) ) ;
#12471 = CARTESIAN_POINT ( 'NONE',  ( 125.6164881442453094, -9.565557343593413364, -10.61323700422348004 ) ) ;
#12472 = CARTESIAN_POINT ( 'NONE',  ( 125.9568481442452850, -6.344957434206665248, -7.627207830600338134 ) ) ;
#12473 = AXIS2_PLACEMENT_3D ( 'NONE', #32946, #11778, #40033 ) ;
#12474 = CARTESIAN_POINT ( 'NONE',  ( 115.4056881442453459, -2.084020599724406786, -8.691656652584148546 ) ) ;
#12475 = CARTESIAN_POINT ( 'NONE',  ( 125.2761281442453054, -10.63000616557722466, -14.87417383870573495 ) ) ;
#12476 = EDGE_CURVE ( 'NONE', #18672, #39054, #22599, .T. ) ;
#12477 = CARTESIAN_POINT ( 'NONE',  ( 108.6767858795247861, -0.7896495226426338832, -17.46756447353520159 ) ) ;
#12478 = CARTESIAN_POINT ( 'NONE',  ( 119.3198281442452924, -9.859900752359374465, -12.68260735090039404 ) ) ;
#12479 = FACE_BOUND ( 'NONE', #901, .T. ) ;
#12480 = LINE ( 'NONE', #2193, #26453 ) ;
#12481 = ORIENTED_EDGE ( 'NONE', *, *, #6978, .F. ) ;
#12482 = LINE ( 'NONE', #36624, #14022 ) ;
#12483 = ADVANCED_FACE ( 'NONE', ( #28321 ), #3131, .T. ) ;
#12484 = CARTESIAN_POINT ( 'NONE',  ( 121.7590748109119687, -7.893985811506177619, -18.51759400769804742 ) ) ;
#12485 = CARTESIAN_POINT ( 'NONE',  ( 124.1685108350118725, 2.242028142391200518, -9.741928829300908532 ) ) ;
#12486 = CIRCLE ( 'NONE', #37231, 0.8718221387495408425 ) ;
#12487 = CYLINDRICAL_SURFACE ( 'NONE', #14321, 1.499999999999996225 ) ;
#12488 = CARTESIAN_POINT ( 'NONE',  ( 118.2420214775786320, -6.222761293078241884, -8.102969835052219238 ) ) ;
#12489 = CARTESIAN_POINT ( 'NONE',  ( 73.07463722459043254, -56.43203361065396706, -34.88111799426488346 ) ) ;
#12490 = CARTESIAN_POINT ( 'NONE',  ( 114.2855644685027698, 0.6938714319018670640, -14.64321520033829493 ) ) ;
#12491 = CARTESIAN_POINT ( 'NONE',  ( 124.7088614775786226, -9.565557343593413364, -10.61323700422348004 ) ) ;
#12492 = CARTESIAN_POINT ( 'NONE',  ( 123.5680096192402146, -1.111561923218658210, -17.14115599315433158 ) ) ;
#12493 = CARTESIAN_POINT ( 'NONE',  ( 124.3117748109119844, 0.1319031606808879209, -14.10382304977623669 ) ) ;
#12494 = CIRCLE ( 'NONE', #38701, 2.999999999999999556 ) ;
#12495 = CARTESIAN_POINT ( 'NONE',  ( 125.2832423080317881, -11.53285783966026834, -16.11696395382945113 ) ) ;
#12496 = CARTESIAN_POINT ( 'NONE',  ( 125.3328548109119964, -9.261995988541697145, -16.69588392320189030 ) ) ;
#12497 = CARTESIAN_POINT ( 'NONE',  ( 119.1496481442453046, -6.222761293078241884, -8.102969835052219238 ) ) ;
#12498 = CARTESIAN_POINT ( 'NONE',  ( 124.9357681442453014, -7.643976991954077427, -18.09477374809248928 ) ) ;
#12499 = EDGE_CURVE ( 'NONE', #19531, #39489, #40072, .T. ) ;
#12500 = VERTEX_POINT ( 'NONE', #40559 ) ;
#12501 = CARTESIAN_POINT ( 'NONE',  ( 124.7655881442452852, 0.5811942927096110934, -14.16772938898807510 ) ) ;
#12502 = CARTESIAN_POINT ( 'NONE',  ( 115.0653281442453277, -6.344957434206662583, -7.627207830600332805 ) ) ;
#12503 = CARTESIAN_POINT ( 'NONE',  ( 117.0111608795247946, -1.325403438956436419, -16.93181055722141792 ) ) ;
#12504 = CARTESIAN_POINT ( 'NONE',  ( 112.7395348109119766, -4.153390946401321671, -8.397313243818183892 ) ) ;
#12505 = EDGE_CURVE ( 'NONE', #27848, #22341, #20136, .T. ) ;
#12506 = CARTESIAN_POINT ( 'NONE',  ( 125.4463081442452932, -4.153390946401325223, -8.397313243818185668 ) ) ;
#12507 = CARTESIAN_POINT ( 'NONE',  ( 125.6732148109119862, 0.5811942927096110934, -14.16772938898807510 ) ) ;
#12508 = CARTESIAN_POINT ( 'NONE',  ( 115.6220983795247861, -0.7896495226426338832, -9.318865927141430916 ) ) ;
#12509 = CARTESIAN_POINT ( 'NONE',  ( 111.2465515045248168, -6.936859964151250502, -18.39754474579286025 ) ) ;
#12510 = LINE ( 'NONE', #19341, #29203 ) ;
#12511 = CARTESIAN_POINT ( 'NONE',  ( 112.9664414775786412, -9.859900752359374465, -12.68260735090039404 ) ) ;
#12512 = DIRECTION ( 'NONE',  ( 0.000000000000000000, -0.3818493186865927203, 0.9242245927363029745 ) ) ;
#12513 = CARTESIAN_POINT ( 'NONE',  ( 111.7327233795247849, -1.325403438956436419, -9.854619843455211026 ) ) ;
#12514 = VERTEX_POINT ( 'NONE', #5655 ) ;
#12515 = CARTESIAN_POINT ( 'NONE',  ( 123.8012348109119642, -9.565557343593413364, -10.61323700422348004 ) ) ;
#12516 = CARTESIAN_POINT ( 'NONE',  ( 120.1601735609119856, -9.645473719204776586, -14.86997237629376656 ) ) ;
#12517 = CARTESIAN_POINT ( 'NONE',  ( 121.0630641859119976, -0.8832429491016019485, -18.19431474523657855 ) ) ;
#12518 = VERTEX_POINT ( 'NONE', #37578 ) ;
#12519 = CARTESIAN_POINT ( 'NONE',  ( 59.62174278132244609, -14.86814543204979344, -8.593215200338315540 ) ) ;
#12520 = CARTESIAN_POINT ( 'NONE',  ( 116.5028905619397079, -11.93022180958501544, -21.11349849701261050 ) ) ;
#12521 = ORIENTED_EDGE ( 'NONE', *, *, #30606, .F. ) ;
#12522 = CARTESIAN_POINT ( 'NONE',  ( 117.3911214775786505, -1.561330072975668504, -17.79121239304076951 ) ) ;
#12523 = AXIS2_PLACEMENT_3D ( 'NONE', #12077, #7518, #35547 ) ;
#12524 = CARTESIAN_POINT ( 'NONE',  ( 124.5386814775786206, -4.153390946401325223, -8.397313243818185668 ) ) ;
#12525 = CARTESIAN_POINT ( 'NONE',  ( 113.7606148109119886, -7.894159318335828068, -9.358103419637847864 ) ) ;
#12526 = DIRECTION ( 'NONE',  ( -0.6937550123170076466, 0.2674776663120608799, -0.6686999932026935767 ) ) ;
#12527 = CARTESIAN_POINT ( 'NONE',  ( 114.8838660002551109, -2.334846009198400907, -18.01015021110789149 ) ) ;
#12528 = CARTESIAN_POINT ( 'NONE',  ( 114.7249681442453237, 0.2603800115204892296, -16.42320221600525088 ) ) ;
#12529 = CARTESIAN_POINT ( 'NONE',  ( 114.0941296295247867, -4.863998795839590272, -8.388885654883775800 ) ) ;
#12530 = CIRCLE ( 'NONE', #38735, 5.999999999999997335 ) ;
#12531 = CARTESIAN_POINT ( 'NONE',  ( 125.2761281442453054, -10.63000616557722466, -14.87417383870573495 ) ) ;
#12532 = LINE ( 'NONE', #5220, #31573 ) ;
#12533 = ORIENTED_EDGE ( 'NONE', *, *, #27184, .F. ) ;
#12534 = CARTESIAN_POINT ( 'NONE',  ( 113.0798948109119948, -0.4660016031367893996, -10.09054647747474043 ) ) ;
#12535 = CARTESIAN_POINT ( 'NONE',  ( 115.1220548109119761, -1.833838273342658809, -17.42832698103878286 ) ) ;
#12536 = DIRECTION ( 'NONE',  ( 0.000000000000000000, -0.9242245927363029745, -0.3818493186865927758 ) ) ;
#12537 = CARTESIAN_POINT ( 'NONE',  ( 125.5597614775786326, -7.894159318335828068, -9.358103419637847864 ) ) ;
#12538 = ORIENTED_EDGE ( 'NONE', *, *, #295, .F. ) ;
#12539 = CARTESIAN_POINT ( 'NONE',  ( 120.0005481442453146, -5.638512984488999180, -18.83840828888717311 ) ) ;
#12540 = PLANE ( 'NONE',  #21578 ) ;
#12541 = CARTESIAN_POINT ( 'NONE',  ( 115.5950730757767531, -0.9924539043446216624, -17.29976612834909133 ) ) ;
#12542 = CARTESIAN_POINT ( 'NONE',  ( -13.78505786849281911, -3.796669023460694792, -17.89321520033831447 ) ) ;
#12543 = CARTESIAN_POINT ( 'NONE',  ( 112.6138494832010650, -2.324775150319229766, -18.02356106541842706 ) ) ;
#12544 = CARTESIAN_POINT ( 'NONE',  ( 114.3846081442453197, 0.4262465694468514643, -12.03445270309931736 ) ) ;
#12545 = DIRECTION ( 'NONE',  ( 0.5040994586965589219, 0.8636456077245089347, 0.000000000000000000 ) ) ;
#12546 = VECTOR ( 'NONE', #23783, 1000.000000000000114 ) ;
#12547 = CARTESIAN_POINT ( 'NONE',  ( 125.3005380000369371, -2.213024231627517491, -20.05538928696255851 ) ) ;
#12548 = CARTESIAN_POINT ( 'NONE',  ( 111.6050014775786536, 0.1319031606808879209, -14.10382304977623669 ) ) ;
#12549 = CARTESIAN_POINT ( 'NONE',  ( 113.6471614775786492, -5.638512984488999180, -18.83840828888717311 ) ) ;
#12550 = CARTESIAN_POINT ( 'NONE',  ( 122.3132204359119868, -10.25716656981731489, -12.88942061488890545 ) ) ;
#12551 = CARTESIAN_POINT ( 'NONE',  ( 113.2500748109119968, -6.344957434206662583, -7.627207830600332805 ) ) ;
#12552 = CARTESIAN_POINT ( 'NONE',  ( 114.1009748109119784, -5.574606645277164318, -18.38911715685844683 ) ) ;
#12553 = CARTESIAN_POINT ( 'NONE',  ( 124.6521348109119884, -1.561330072975668948, -17.79121239304076951 ) ) ;
#12554 = EDGE_CURVE ( 'NONE', #33002, #42672, #23459, .T. ) ;
#12555 = CARTESIAN_POINT ( 'NONE',  ( 123.5176014775786228, -9.261995988541697145, -16.69588392320189030 ) ) ;
#12556 = ORIENTED_EDGE ( 'NONE', *, *, #39550, .F. ) ;
#12557 = CARTESIAN_POINT ( 'NONE',  ( 94.99177781699742695, -25.99489077589524300, -13.39321520033831447 ) ) ;
#12558 = CARTESIAN_POINT ( 'NONE',  ( 111.8021765045248372, -7.250697342233347165, -19.15521520033831138 ) ) ;
#12559 = CARTESIAN_POINT ( 'NONE',  ( 108.7462390045248242, -9.868328341294098749, -11.32035403202665869 ) ) ;
#12560 = AXIS2_PLACEMENT_3D ( 'NONE', #15726, #6134, #33024 ) ;
#12561 = CARTESIAN_POINT ( 'NONE',  ( 109.2324108795247923, -1.325403438956436419, -16.93181055722141792 ) ) ;
#12562 = DIRECTION ( 'NONE',  ( 0.000000000000000000, 0.3818493186865928868, -0.9242245927363027524 ) ) ;
#12563 = CARTESIAN_POINT ( 'NONE',  ( 120.2274548109119934, 0.5811942927096110934, -14.16772938898807510 ) ) ;
#12564 = ORIENTED_EDGE ( 'NONE', *, *, #7187, .F. ) ;
#12565 = CARTESIAN_POINT ( 'NONE',  ( 117.2294421295247844, -10.76310523276723785, -4.893215200338314474 ) ) ;
#12566 = DIRECTION ( 'NONE',  ( 1.000000000000000000, 0.000000000000000000, -0.000000000000000000 ) ) ;
#12567 = CARTESIAN_POINT ( 'NONE',  ( 75.14134903615895666, -42.50702760616825771, -10.39321520033831625 ) ) ;
#12568 = EDGE_CURVE ( 'NONE', #42269, #20890, #1615, .T. ) ;
#12569 = CARTESIAN_POINT ( 'NONE',  ( 114.8951481442453115, -8.899110576539710493, -16.42337572283490132 ) ) ;
#12570 = CARTESIAN_POINT ( 'NONE',  ( 107.4266296295248821, -4.863998795839590272, -8.388885654883775800 ) ) ;
#12571 = PRESENTATION_LAYER_ASSIGNMENT (  '', '', ( #32202 ) ) ;
#12572 = CARTESIAN_POINT ( 'NONE',  ( 121.3619881442452879, -4.089484607189486809, -7.948022111789456723 ) ) ;
#12573 = CARTESIAN_POINT ( 'NONE',  ( 109.3018640045248304, -10.62599879583958717, -11.00651665394454604 ) ) ;
#12574 = CARTESIAN_POINT ( 'NONE',  ( 63.69189222814998175, -64.02637234200076932, -46.77412892735921446 ) ) ;
#12575 = EDGE_LOOP ( 'NONE', ( #15745, #8416, #40910, #10951, #7777 ) ) ;
#12576 = CARTESIAN_POINT ( 'NONE',  ( 121.4544569107182070, -2.467220198592778413, -17.83387418641524391 ) ) ;
#12577 = CARTESIAN_POINT ( 'NONE',  ( 121.3052614775786111, -7.643976991954077427, -18.09477374809248928 ) ) ;
#12578 = CARTESIAN_POINT ( 'NONE',  ( 118.0151148109119816, -10.63000616557722466, -14.87417383870573495 ) ) ;
#12579 = FACE_OUTER_BOUND ( 'NONE', #14901, .T. ) ;
#12580 = CARTESIAN_POINT ( 'NONE',  ( 114.7249681442453237, 0.2603800115204892296, -16.42320221600525088 ) ) ;
#12581 = CARTESIAN_POINT ( 'NONE',  ( 143.3676850761856940, -50.16718729050181480, -4.893215200338314474 ) ) ;
#12582 = CARTESIAN_POINT ( 'NONE',  ( 124.4819548109119722, -2.084020599724406786, -8.691656652584148546 ) ) ;
#12583 = CARTESIAN_POINT ( 'NONE',  ( 118.5256548109119876, -8.899110576539710493, -16.42337572283490132 ) ) ;
#12584 = VERTEX_POINT ( 'NONE', #11030 ) ;
#12585 = B_SPLINE_CURVE_WITH_KNOTS ( 'NONE', 3,
 ( #1933, #36807, #5576, #8337, #15859, #8563, #15404, #33378, #42777, #32932 ),
 .UNSPECIFIED., .F., .F.,
 ( 4, 3, 3, 4 ),
 ( 0.000000000000000000, 0.0001671877548681289800, 0.0003343755096277714980, 0.0006463528481650629171 ),
 .UNSPECIFIED. ) ;
#12586 = CARTESIAN_POINT ( 'NONE',  ( 123.4244704359119709, 1.345710702986147034, -13.97328579221134426 ) ) ;
#12587 = VECTOR ( 'NONE', #28371, 1000.000000000000114 ) ;
#12588 = CARTESIAN_POINT ( 'NONE',  ( 113.9875214775786532, -0.4660016031367893996, -10.09054647747474043 ) ) ;
#12589 = CARTESIAN_POINT ( 'NONE',  ( 120.7379948109119709, 0.4262465694468514643, -12.03445270309931736 ) ) ;
#12590 = VERTEX_POINT ( 'NONE', #31763 ) ;
#12591 = CARTESIAN_POINT ( 'NONE',  ( 123.7022829359119811, -5.367793381288652910, -18.78638297431638904 ) ) ;
#12592 = CARTESIAN_POINT ( 'NONE',  ( 118.6391081442452986, -4.089484607189486809, -7.948022111789456723 ) ) ;
#12593 = PRODUCT_DEFINITION_FORMATION_WITH_SPECIFIED_SOURCE ( 'ANY', '', #3366, .NOT_KNOWN. ) ;
#12594 = CARTESIAN_POINT ( 'NONE',  ( 111.5243640045248412, -10.62599879583958717, -11.00651665394454604 ) ) ;
#12595 = CARTESIAN_POINT ( 'NONE',  ( 114.5547881442453217, -4.153390946401321671, -8.397313243818183892 ) ) ;
#12596 = EDGE_LOOP ( 'NONE', ( #44834, #5726 ) ) ;
#12597 = CIRCLE ( 'NONE', #38063, 2.000000000000000444 ) ;
#12598 = ORIENTED_EDGE ( 'NONE', *, *, #8387, .F. ) ;
#12599 = CARTESIAN_POINT ( 'NONE',  ( 125.4463081442452932, -4.153390946401325223, -8.397313243818185668 ) ) ;
#12600 = CARTESIAN_POINT ( 'NONE',  ( 119.6034614775786196, -3.505236298600246325, -18.68346056562440793 ) ) ;
#12601 = FILL_AREA_STYLE ('',( #26273 ) ) ;
#12602 = EDGE_CURVE ( 'NONE', #20584, #26785, #8051, .T. ) ;
#12603 = CARTESIAN_POINT ( 'NONE',  ( 62.55594166779781773, -34.86283735444163767, -5.893215200338315363 ) ) ;
#12604 = CARTESIAN_POINT ( 'NONE',  ( 120.0572748109119772, -3.383040157471821630, -19.15922257007629170 ) ) ;
#12605 = CARTESIAN_POINT ( 'NONE',  ( 106.4542858795248179, -0.7896495226426338832, -17.46756447353520159 ) ) ;
#12606 = CARTESIAN_POINT ( 'NONE',  ( 117.6180281442453150, -0.4660016031367893996, -10.09054647747474043 ) ) ;
#12608 = CARTESIAN_POINT ( 'NONE',  ( 114.6682414775786469, -7.894159318335828068, -9.358103419637847864 ) ) ;
#12607 = CARTESIAN_POINT ( 'NONE',  ( 114.2711548109119803, -9.988377603198976828, -10.36322818467138340 ) ) ;
#12609 = CARTESIAN_POINT ( 'NONE',  ( 125.4463081442452932, -4.153390946401325223, -8.397313243818185668 ) ) ;
#12610 = CARTESIAN_POINT ( 'NONE',  ( 113.5337081442453240, -9.261995988541697145, -16.69588392320189030 ) ) ;
#12611 = ORIENTED_EDGE ( 'NONE', *, *, #14992, .F. ) ;
#12612 = CARTESIAN_POINT ( 'NONE',  ( 122.2696148109119889, -5.574606645277164318, -18.38911715685844683 ) ) ;
#12613 = FACE_OUTER_BOUND ( 'NONE', #7976, .T. ) ;
#12614 = AXIS2_PLACEMENT_3D ( 'NONE', #23741, #34637, #3197 ) ;
#12615 = CARTESIAN_POINT ( 'NONE',  ( 113.8588425628257284, -2.263366209404213958, -18.10533625161307114 ) ) ;
#12616 = CARTESIAN_POINT ( 'NONE',  ( 112.3578015045248861, -2.477300249445798297, -7.631215200338321125 ) ) ;
#12617 = VECTOR ( 'NONE', #4865, 1000.000000000000114 ) ;
#12618 = CARTESIAN_POINT ( 'NONE',  ( 112.9828796295247884, -4.863998795839590272, -8.388885654883775800 ) ) ;
#12619 = CARTESIAN_POINT ( 'NONE',  ( 110.8992858795247827, -0.7896495226426338832, -17.46756447353520159 ) ) ;
#12620 = ADVANCED_FACE ( 'NONE', ( #4620 ), #458, .T. ) ;
#12621 = B_SPLINE_CURVE_WITH_KNOTS ( 'NONE', 3,
 ( #21227, #7535, #15279, #24648, #38764, #35106, #3888, #17808, #35562, #690 ),
 .UNSPECIFIED., .F., .F.,
 ( 4, 3, 3, 4 ),
 ( 0.000000000000000000, 0.0002476486808869835118, 0.0004952973797228650337, 0.0009539399846111519445 ),
 .UNSPECIFIED. ) ;
#12622 = EDGE_CURVE ( 'NONE', #18302, #12590, #37083, .T. ) ;
#12623 = CARTESIAN_POINT ( 'NONE',  ( 119.5467348109119712, -4.089484607189486809, -7.948022111789456723 ) ) ;
#12624 = ORIENTED_EDGE ( 'NONE', *, *, #12622, .F. ) ;
#12625 = CARTESIAN_POINT ( 'NONE',  ( 121.7590748109119687, -7.893985811506177619, -18.51759400769804742 ) ) ;
#12626 = FACE_OUTER_BOUND ( 'NONE', #17290, .T. ) ;
#12627 = CARTESIAN_POINT ( 'NONE',  ( 106.7320983795247855, -0.7896495226426338832, -9.318865927141430916 ) ) ;
#12628 = CARTESIAN_POINT ( 'NONE',  ( 120.1140014775786398, -1.561330072975668504, -17.79121239304076951 ) ) ;
#12629 = CARTESIAN_POINT ( 'NONE',  ( 119.6601881442453106, -8.166667518702819706, -8.995218007635861213 ) ) ;
#12630 = CARTESIAN_POINT ( 'NONE',  ( 64.64508731025817667, -2.688136943189093575, -18.61997050879359250 ) ) ;
#12631 = CARTESIAN_POINT ( 'NONE',  ( 120.7503284624957729, -6.270977643812245539, -18.77740645536395547 ) ) ;
#12632 = ORIENTED_EDGE ( 'NONE', *, *, #5077, .F. ) ;
#12633 = AXIS2_PLACEMENT_3D ( 'NONE', #8375, #25259, #32080 ) ;
#12634 = CARTESIAN_POINT ( 'NONE',  ( -1.910975223132118872, -6.857719673119084369, -7.986702415358247542 ) ) ;
#12635 = LINE ( 'NONE', #26982, #37653 ) ;
#12636 = CARTESIAN_POINT ( 'NONE',  ( 124.4819548109119722, -2.084020599724406786, -8.691656652584148546 ) ) ;
#12637 = B_SPLINE_CURVE_WITH_KNOTS ( 'NONE', 3,
 ( #116, #28165, #17894, #3749, #35424, #35196, #32012, #38855, #7623, #8084, #34961, #42075, #28381, #3972, #4200, #14925, #27943, #775, #21763, #41853, #563, #7395, #1009, #4429, #31791, #42746, #18345, #42294, #11511, #32238 ),
 .UNSPECIFIED., .F., .F.,
 ( 4, 2, 2, 1, 1, 1, 2, 2, 2, 1, 1, 1, 2, 2, 1, 1, 2, 2, 4 ),
 ( 0.000000000000000000, 0.2499999999997726818, 0.3749999999996590505, 0.4374999999996024291, 0.4687499999995737299, 0.4843749999995729527, 0.4921874999995729527, 0.4999999999995730082, 0.6249999999998475664, 0.6874999999999731326, 0.7187500000000250910, 0.7343750000000514033, 0.7421875000000531797, 0.7500000000000549560, 0.8125000000000354161, 0.8437500000000255351, 0.8593750000000209832, 0.8750000000000164313, 1.000000000000000000 ),
 .UNSPECIFIED. ) ;
#12638 = CARTESIAN_POINT ( 'NONE',  ( 114.1635827545248389, -6.936859964151250502, -8.388885654883777576 ) ) ;
#12639 = CARTESIAN_POINT ( 'NONE',  ( 109.3018640045248304, 0.1403307496149616695, -15.46607636864997204 ) ) ;
#12640 = CARTESIAN_POINT ( 'NONE',  ( 117.9016614775786280, -0.1624402480850797581, -16.17319339645315424 ) ) ;
#12641 = DIRECTION ( 'NONE',  ( -0.7400066460894876297, 0.6725995567522979890, 0.000000000000000000 ) ) ;
#12642 = CARTESIAN_POINT ( 'NONE',  ( 69.25460375973102600, -25.92061903028353953, -5.871778085103695588 ) ) ;
#12643 = CARTESIAN_POINT ( 'NONE',  ( 111.6050014775786536, 0.1319031606808879209, -14.10382304977623669 ) ) ;
#12644 = CARTESIAN_POINT ( 'NONE',  ( 125.1059481442452750, -8.166667518702819706, -8.995218007635861213 ) ) ;
#12645 = EDGE_LOOP ( 'NONE', ( #19982, #33835, #14528, #44732, #23764 ) ) ;
#12646 = CARTESIAN_POINT ( 'NONE',  ( 122.6099748109119929, -0.8288870151387760510, -10.36305467784173118 ) ) ;
#12647 = CARTESIAN_POINT ( 'NONE',  ( 116.7104014775786425, -0.4660016031367893996, -10.09054647747474043 ) ) ;
#12648 = CARTESIAN_POINT ( 'NONE',  ( 122.6099748109119929, -9.261995988541697145, -16.69588392320189030 ) ) ;
#12649 = CARTESIAN_POINT ( 'NONE',  ( 122.4965214775786251, 0.1319031606808879209, -14.10382304977623669 ) ) ;
#12650 = ORIENTED_EDGE ( 'NONE', *, *, #11649, .T. ) ;
#12651 = CARTESIAN_POINT ( 'NONE',  ( 123.4660871540078375, -2.348512537728041583, -17.99195118506215962 ) ) ;
#12652 = AXIS2_PLACEMENT_3D ( 'NONE', #39477, #1389, #8013 ) ;
#12653 = CARTESIAN_POINT ( 'NONE',  ( 122.7234281442452755, -5.638512984488999180, -18.83840828888717311 ) ) ;
#12654 = CARTESIAN_POINT ( 'NONE',  ( 124.7442371152529006, -8.343757344481284477, -6.432680279141536950 ) ) ;
#12655 = CARTESIAN_POINT ( 'NONE',  ( 124.5386814775786206, -5.638512984488999180, -18.83840828888717311 ) ) ;
#12656 = CARTESIAN_POINT ( 'NONE',  ( 106.8015515045248378, -2.477300249445798297, -7.631215200338321125 ) ) ;
#12657 = DIRECTION ( 'NONE',  ( 0.000000000000000000, -1.000000000000000000, 0.000000000000000000 ) ) ;
#12658 = CARTESIAN_POINT ( 'NONE',  ( 119.1138497606643512, -2.236191541394346061, -18.14152338500401029 ) ) ;
#12659 = CARTESIAN_POINT ( 'NONE',  ( 110.6909265045248247, -2.791137627527939813, -8.388885654883777576 ) ) ;
#12660 = DIRECTION ( 'NONE',  ( 3.332709719099110404E-30, -9.283845114648369353E-44, 1.000000000000000000 ) ) ;
#12661 = CARTESIAN_POINT ( 'NONE',  ( 118.2987481442453088, -7.894159318335828068, -9.358103419637847864 ) ) ;
#12662 = CARTESIAN_POINT ( 'NONE',  ( 111.5482748109120053, -0.1624402480850797581, -16.17319339645315424 ) ) ;
#12663 = CARTESIAN_POINT ( 'NONE',  ( 126.6690297232769780, -6.379022919317676177, -18.39419181305856910 ) ) ;
#12664 = EDGE_LOOP ( 'NONE', ( #7997, #35155, #30719, #10939 ) ) ;
#12665 = CARTESIAN_POINT ( 'NONE',  ( 116.3892577545247349, -6.935066607705044461, -8.393215200338321580 ) ) ;
#12666 = CARTESIAN_POINT ( 'NONE',  ( 115.2355081442453155, 0.1319031606808879209, -14.10382304977623669 ) ) ;
#12667 = CARTESIAN_POINT ( 'NONE',  ( 117.2294421295247844, -9.690077956319688823, -4.893215200338314474 ) ) ;
#12668 = DIRECTION ( 'NONE',  ( -0.9908103287288503314, 0.1352586133457950868, 0.000000000000000000 ) ) ;
#12669 = CARTESIAN_POINT ( 'NONE',  ( 111.9453614775786434, -7.894159318335828068, -9.358103419637847864 ) ) ;
#12671 = CARTESIAN_POINT ( 'NONE',  ( 123.6877814775786533, -3.383040157471821630, -19.15922257007629170 ) ) ;
#12670 = CARTESIAN_POINT ( 'NONE',  ( 70.27992438911469719, -26.36696139213632506, -5.630764001613508540 ) ) ;
#12672 = EDGE_CURVE ( 'NONE', #42783, #6454, #37551, .T. ) ;
#12673 = CARTESIAN_POINT ( 'NONE',  ( 124.1415948109119540, -3.505236298600246325, -18.68346056562440793 ) ) ;
#12674 = ORIENTED_EDGE ( 'NONE', *, *, #24470, .T. ) ;
#12675 = CARTESIAN_POINT ( 'NONE',  ( 110.3910934012278773, 0.04929351793716424401, -14.64321520033829493 ) ) ;
#12676 = CARTESIAN_POINT ( 'NONE',  ( 125.3328548109119964, -9.261995988541697145, -16.69588392320189030 ) ) ;
#12677 = CARTESIAN_POINT ( 'NONE',  ( 111.3854577545248645, -2.791137627527939813, -18.39754474579286025 ) ) ;
#12678 = CARTESIAN_POINT ( 'NONE',  ( 126.4106614775786284, -6.222761293078241884, -8.102969835052219238 ) ) ;
#12679 = CARTESIAN_POINT ( 'NONE',  ( 119.9438214775786378, -2.084020599724406786, -8.691656652584148546 ) ) ;
#12680 = DIRECTION ( 'NONE',  ( 1.000000000000000000, 0.000000000000000000, 0.000000000000000000 ) ) ;
#12681 = CARTESIAN_POINT ( 'NONE',  ( 105.8986608795248401, -8.938348069036489818, -9.318865927141430916 ) ) ;
#12682 = CARTESIAN_POINT ( 'NONE',  ( 83.83554121260367253, -25.99489077589524300, -13.39321520033831625 ) ) ;
#12683 = DIRECTION ( 'NONE',  ( 0.000000000000000000, -0.3818493186865927203, 0.9242245927363029745 ) ) ;
#12684 = CARTESIAN_POINT ( 'NONE',  ( 113.1933481442453058, -5.574606645277164318, -18.38911715685844683 ) ) ;
#12685 = CARTESIAN_POINT ( 'NONE',  ( 112.0799890045248475, 0.8980012041604421569, -15.77991374673208469 ) ) ;
#12686 = CARTESIAN_POINT ( 'NONE',  ( -13.55938949877377020, -4.790790901322431239, -17.98555846284454418 ) ) ;
#12687 = CARTESIAN_POINT ( 'NONE',  ( 115.2053796295247849, -4.863998795839590272, -19.15521520033831493 ) ) ;
#12688 = CARTESIAN_POINT ( 'NONE',  ( 121.0783548109119749, 0.2603800115204892296, -16.42320221600525088 ) ) ;
#12689 = CARTESIAN_POINT ( 'NONE',  ( 120.8514481442452961, -7.893985811506177619, -18.51759400769804742 ) ) ;
#12690 = CARTESIAN_POINT ( 'NONE',  ( 70.19189222814998175, -55.76308905022629858, -35.50805039322867884 ) ) ;
#12691 = CARTESIAN_POINT ( 'NONE',  ( 117.9583881442453048, -10.30919188438810075, -12.61870101168855918 ) ) ;
#12692 = FACE_OUTER_BOUND ( 'NONE', #15088, .T. ) ;
#12693 = ORIENTED_EDGE ( 'NONE', *, *, #13141, .T. ) ;
#12694 = CARTESIAN_POINT ( 'NONE',  ( 114.4413348109119823, -0.8288870151387760510, -10.36305467784173118 ) ) ;
#12695 = CARTESIAN_POINT ( 'NONE',  ( 112.6828081442453282, -2.084020599724406786, -8.691656652584148546 ) ) ;
#12696 = CARTESIAN_POINT ( 'NONE',  ( 121.9292548109119849, -1.561330072975668948, -17.79121239304076951 ) ) ;
#12697 = CARTESIAN_POINT ( 'NONE',  ( 112.3991748109119868, -8.166667518702817929, -8.995218007635859436 ) ) ;
#12698 = CARTESIAN_POINT ( 'NONE',  ( 114.1009748109119784, -5.574606645277164318, -18.38911715685844683 ) ) ;
#12699 = ORIENTED_EDGE ( 'NONE', *, *, #7752, .T. ) ;
#12700 = CARTESIAN_POINT ( 'NONE',  ( 119.0929214775786278, -4.153390946401325223, -8.397313243818185668 ) ) ;
#12701 = CARTESIAN_POINT ( 'NONE',  ( 125.9001214775786224, -4.089484607189486809, -7.948022111789456723 ) ) ;
#12702 = CARTESIAN_POINT ( 'NONE',  ( 111.0381921295247878, 0.8980012041604618078, -13.39321520033831447 ) ) ;
#12703 = CARTESIAN_POINT ( 'NONE',  ( 119.5467348109119712, -5.574606645277164318, -18.38911715685844683 ) ) ;
#12704 = CARTESIAN_POINT ( 'NONE',  ( 116.7875679639338244, -3.298653660685034961, -18.34516049763993450 ) ) ;
#12705 = CARTESIAN_POINT ( 'NONE',  ( 116.5249890045247980, 0.8980012041604421569, -15.77991374673208469 ) ) ;
#12706 = ORIENTED_EDGE ( 'NONE', *, *, #19437, .F. ) ;
#12707 = CARTESIAN_POINT ( 'NONE',  ( 123.1466579359119891, -4.360204210389833968, -8.000047426360245240 ) ) ;
#12708 = CARTESIAN_POINT ( 'NONE',  ( 122.4397948109119767, -9.988377603198976828, -10.36322818467138340 ) ) ;
#12709 = CARTESIAN_POINT ( 'NONE',  ( 71.02242295334774269, -99.02728775972636299, -55.91838671430374319 ) ) ;
#12710 = CARTESIAN_POINT ( 'NONE',  ( 112.0588148109119828, 0.5811942927096154232, -14.16772938898807155 ) ) ;
#12711 = PRODUCT_DEFINITION ( 'UNKNOWN', '', #4558, #39259 ) ;
#12712 = CARTESIAN_POINT ( 'NONE',  ( 122.4521266859119777, -0.06289925094098039460, -9.412459353600686640 ) ) ;
#12713 = DIRECTION ( 'NONE',  ( 1.000000000000000000, 0.000000000000000000, -0.000000000000000000 ) ) ;
#12714 = CARTESIAN_POINT ( 'NONE',  ( 104.9957702545248566, 0.1403307496149616695, -11.32035403202665336 ) ) ;
#12715 = CARTESIAN_POINT ( 'NONE',  ( 125.6732148109119862, -9.859900752359378018, -12.68260735090039759 ) ) ;
#12716 = CARTESIAN_POINT ( 'NONE',  ( 125.3455228489891198, -11.53585155397754924, -15.73626133961844609 ) ) ;
#12717 = CARTESIAN_POINT ( 'NONE',  ( 126.1270281442452870, -10.30919188438810075, -12.61870101168855918 ) ) ;
#12718 = CARTESIAN_POINT ( 'NONE',  ( 117.9583881442453048, 0.1319031606808879209, -14.10382304977623669 ) ) ;
#12719 = CARTESIAN_POINT ( 'NONE',  ( 125.4463081442452932, -4.153390946401325223, -8.397313243818185668 ) ) ;
#12720 = VERTEX_POINT ( 'NONE', #40306 ) ;
#12721 = CARTESIAN_POINT ( 'NONE',  ( 122.0427081442452817, 0.5811942927096110934, -14.16772938898807510 ) ) ;
#12722 = CARTESIAN_POINT ( 'NONE',  ( 115.5758681442453053, -1.561330072975668060, -17.79121239304076951 ) ) ;
#12723 = CARTESIAN_POINT ( 'NONE',  ( 116.4555358795247884, -8.402594152722688392, -9.854619843455216355 ) ) ;
#12724 = CARTESIAN_POINT ( 'NONE',  ( 151.2860562277021472, -4.863998795839242995, -13.39321520033831447 ) ) ;
#12725 =( BOUNDED_SURFACE ( )  B_SPLINE_SURFACE ( 1, 2, ( 
 ( #1180, #31955, #15093, #29003, #18064, #36274, #42911, #18957, #29221, #11673, #32847, #25801, #18287, #39711, #15537, #25136, #43357, #42689, #25582, #39031, #24904, #39485, #35368, #38799, #22156, #21483, #7570, #4144, #14642, #42465, #36049, #21928, #4817, #954, #11457, #8694, #2295, #29670, #5487, #26251, #12352, #40162, #5942, #9374, #43582, #30349, #19865, #40849, #19407, #2522, #40389, #19186, #8924, #12580, #22826, #39934, #16223, #16675, #30570, #15993, #13029, #33753, #9150, #36717, #2070, #29898, #16449, #1838, #44273, #26485, #23283, #33065, #44041, #43814, #26927, #12805, #23519, #15767, #33294, #23057, #9604, #36943, #37407, #5713, #20097, #22600, #12126, #19631, #33515, #33982, #37167, #6176, #2751, #40617, #30128, #26029, #36500, #5269, #26705, #3862, #20984, #20544, #17563, #41741, #31457, #41962, #23747, #38295, #44947, #17784, #6412, #20319, #44490, #13256, #34857, #6631, #28054, #20765, #13920, #13705, #37638, #27159, #225, #10728, #31017, #41526, #6858, #27612, #34203, #10505, #41308, #41081, #17348, #9837, #2978, #7074, #3644, #34423, #16906, #30798, #7287, #13483, #37856, #27830, #14139, #31237, #44723, #24406, #10069, #24628, #27385, #38510, #21203, #23970, #3204, #17129, #38080, #9, #10284, #24188, #35082, #34644, #3430, #12469, #28504, #15660, #19305, #669, #43695, #43478, #1735, #14586, #31678, #26369, #25306, #36834, #447, #42410, #18232, #4081, #35770, #35541, #32958, #39200, #7966, #9043, #35310, #11174, #28727, #4312, #22942, #21876, #42186, #7511, #22714, #10946, #896, #29561, #1959, #25078, #4540, #5603, #14363, #8811, #19073, #29783, #12245, #21650, #26142, #38970, #28277, #24849, #7739, #40277, #32128, #11397, #18005, #21426, #38741, #14815, #31904, #40044, #42633, #36612, #5388, #33184, #15887, #27049, #37521, #30010, #23867, #44383, #13377, #44161, #6523, #9954, #6058, #24083, #41194, #40733, #37753, #16796, #20439, #17023, #13146, #3096, #34322, #30463, #9489, #30915, #44838, #5829, #12925, #40968, #9722, #23635, #16336 ),
 ( #40508, #13594, #43927, #33867, #30692, #27503, #30239, #6294, #41422, #37977, #10177, #20214, #19526, #34099, #23404, #2867, #2409, #33403, #2178, #26821, #16108, #37288, #44611, #37057, #9268, #12695, #19978, #23179, #27279, #2636, #26595, #19749, #33634, #16568, #14256, #24736, #17240, #11063, #31574, #569, #31348, #31131, #14479, #7180, #11288, #13815, #27726, #6752, #25196, #42300, #14035, #35432, #28173, #21319, #21090, #45055, #34538, #24965, #18124, #38410, #3755, #42081, #34967, #41642, #3978, #3538, #20662, #38625, #3319, #10398, #28389, #38861, #27951, #24308, #38194, #14704, #20880, #122, #35204, #7629, #7401, #6971, #17901, #17453, #4206, #34755, #32019, #21543, #41859, #10621, #24523, #343, #31798, #17677, #10841, #783, #28618, #42528, #22438, #26086, #8090, #5332, #5101, #8537, #21993, #39094, #33130, #32687, #43640, #7864, #35883, #25647, #11517, #43197, #42968, #39766, #1457, #15378, #15829, #42754, #4653, #36110, #11735, #29726, #29282, #4435, #14931, #29505, #18353, #8313, #36331, #8756, #18574, #11963, #12414, #21770, #15601, #25862, #36557, #19016, #29059, #32903, #32466, #35663, #32244, #1242, #19249, #15153, #18798, #25422, #28842, #1015, #39551, #39323, #1679, #22213, #43421, #4881, #12186, #39990, #22661, #1900, #36780, #30637, #6003, #20163, #5772, #5551, #34046, #26772, #30861, #33351, #2124, #26314, #44784, #16743, #33579, #9901, #2583, #40912, #40681, #19469, #8987, #44554, #37702, #12873, #23346, #33813, #9433, #16053, #23584, #23124, #40222, #44333, #22887, #29959, #2814, #13319, #2354, #43874, #12646, #34271, #40453, #19692, #9665, #27224, #13093, #26542, #37468, #37001, #23814, #9215, #6473, #41142, #16286, #30188, #44106, #19926, #26992, #37229, #16514, #20385, #30413, #3044, #16968, #6240, #10568, #31079, #3490, #17406, #21266, #3263, #35148, #13981, #24684, #20610, #290, #31295, #3926, #14204, #24909, #34485, #10346, #24464, #17846, #38356, #31745, #7131, #21489, #10128, #13542, #21042, #17188, #35373, #10787, #38571, #513 ) ),
 .UNSPECIFIED., .F., .F., .T. ) 
 B_SPLINE_SURFACE_WITH_KNOTS ( ( 2, 2 ),
 ( 3, 2, 2, 2, 2, 2, 2, 2, 2, 2, 2, 2, 2, 2, 2, 2, 2, 2, 2, 2, 2, 2, 2, 2, 2, 2, 2, 2, 2, 2, 2, 2, 2, 2, 2, 2, 2, 2, 2, 2, 2, 2, 2, 2, 2, 2, 2, 2, 2, 2, 2, 2, 2, 2, 2, 2, 2, 2, 2, 2, 2, 2, 2, 2, 2, 2, 2, 2, 2, 2, 2, 2, 2, 2, 2, 2, 2, 2, 2, 2, 2, 2, 2, 2, 2, 2, 2, 2, 2, 2, 2, 2, 2, 2, 2, 2, 2, 2, 2, 2, 2, 2, 2, 2, 2, 2, 2, 2, 2, 2, 2, 2, 2, 2, 2, 2, 2, 2, 2, 2, 2, 2, 2, 2, 2, 2, 2, 2, 3 ),
 ( 0.000000000000000000, 1.000000000000000000 ),
 ( 0.000000000000000000, 0.007812500000000000000, 0.01562500000000000000, 0.02343750000000000000, 0.03125000000000000000, 0.03906250000000000000, 0.04687500000000000000, 0.05468750000000000000, 0.06250000000000000000, 0.07031250000000000000, 0.07812500000000000000, 0.08593750000000000000, 0.09375000000000000000, 0.1015625000000000000, 0.1093750000000000000, 0.1171875000000000000, 0.1250000000000000000, 0.1328125000000000000, 0.1406250000000000000, 0.1484375000000000000, 0.1562500000000000000, 0.1640625000000000000, 0.1718750000000000000, 0.1796875000000000000, 0.1875000000000000000, 0.1953125000000000000, 0.2031250000000000000, 0.2109375000000000000, 0.2187500000000000000, 0.2265625000000000000, 0.2343750000000000000, 0.2421875000000000000, 0.2500000000000000000, 0.2578125000000000000, 0.2656250000000000000, 0.2734375000000000000, 0.2812500000000000000, 0.2890625000000000000, 0.2968750000000000000, 0.3046875000000000000, 0.3125000000000000000, 0.3203125000000000000, 0.3281250000000000000, 0.3359375000000000000, 0.3437500000000000000, 0.3515625000000000000, 0.3593750000000000000, 0.3671875000000000000, 0.3750000000000000000, 0.3828125000000000000, 0.3906250000000000000, 0.3984375000000000000, 0.4062500000000000000, 0.4140625000000000000, 0.4218750000000000000, 0.4296875000000000000, 0.4375000000000000000, 0.4453125000000000000, 0.4531250000000000000, 0.4609375000000000000, 0.4687500000000000000, 0.4765625000000000000, 0.4843750000000000000, 0.4921875000000000000, 0.5000000000000000000, 0.5078125000000000000, 0.5156250000000000000, 0.5234375000000000000, 0.5312500000000000000, 0.5390625000000000000, 0.5468750000000000000, 0.5546875000000000000, 0.5625000000000000000, 0.5703125000000000000, 0.5781250000000000000, 0.5859375000000000000, 0.5937500000000000000, 0.6015625000000000000, 0.6093750000000000000, 0.6171875000000000000, 0.6250000000000000000, 0.6328125000000000000, 0.6406250000000000000, 0.6484375000000000000, 0.6562500000000000000, 0.6640625000000000000, 0.6718750000000000000, 0.6796875000000000000, 0.6875000000000000000, 0.6953125000000000000, 0.7031250000000000000, 0.7109375000000000000, 0.7187500000000000000, 0.7265625000000000000, 0.7343750000000000000, 0.7421875000000000000, 0.7500000000000000000, 0.7578125000000000000, 0.7656250000000000000, 0.7734375000000000000, 0.7812500000000000000, 0.7890625000000000000, 0.7968750000000000000, 0.8046875000000000000, 0.8125000000000000000, 0.8203125000000000000, 0.8281250000000000000, 0.8359375000000000000, 0.8437500000000000000, 0.8515625000000000000, 0.8593750000000000000, 0.8671875000000000000, 0.8750000000000000000, 0.8828125000000000000, 0.8906250000000000000, 0.8984375000000000000, 0.9062500000000000000, 0.9140625000000000000, 0.9218750000000000000, 0.9296875000000000000, 0.9375000000000000000, 0.9453125000000000000, 0.9531250000000000000, 0.9609375000000000000, 0.9687500000000000000, 0.9765625000000000000, 0.9843750000000000000, 0.9921875000000000000, 1.000000000000000000 ),
 .UNSPECIFIED. ) 
 GEOMETRIC_REPRESENTATION_ITEM ( )  RATIONAL_B_SPLINE_SURFACE ( (
 ( 1.000000000000000000, 0.9238795325112869605, 1.000000000000000000, 0.9238795325112869605, 1.000000000000000000, 0.9238795325112869605, 1.000000000000000000, 0.9238795325112869605, 1.000000000000000000, 0.9238795325112869605, 1.000000000000000000, 0.9238795325112869605, 1.000000000000000000, 0.9238795325112869605, 1.000000000000000000, 0.9238795325112869605, 1.000000000000000000, 0.9238795325112869605, 1.000000000000000000, 0.9238795325112869605, 1.000000000000000000, 0.9238795325112869605, 1.000000000000000000, 0.9238795325112869605, 1.000000000000000000, 0.9238795325112869605, 1.000000000000000000, 0.9238795325112869605, 1.000000000000000000, 0.9238795325112869605, 1.000000000000000000, 0.9238795325112869605, 1.000000000000000000, 0.9238795325112869605, 1.000000000000000000, 0.9238795325112869605, 1.000000000000000000, 0.9238795325112869605, 1.000000000000000000, 0.9238795325112869605, 1.000000000000000000, 0.9238795325112869605, 1.000000000000000000, 0.9238795325112869605, 1.000000000000000000, 0.9238795325112869605, 1.000000000000000000, 0.9238795325112869605, 1.000000000000000000, 0.9238795325112869605, 1.000000000000000000, 0.9238795325112869605, 1.000000000000000000, 0.9238795325112869605, 1.000000000000000000, 0.9238795325112869605, 1.000000000000000000, 0.9238795325112869605, 1.000000000000000000, 0.9238795325112869605, 1.000000000000000000, 0.9238795325112869605, 1.000000000000000000, 0.9238795325112869605, 1.000000000000000000, 0.9238795325112869605, 1.000000000000000000, 0.9238795325112869605, 1.000000000000000000, 0.9238795325112869605, 1.000000000000000000, 0.9238795325112869605, 1.000000000000000000, 0.9238795325112869605, 1.000000000000000000, 0.9238795325112869605, 1.000000000000000000, 0.9238795325112869605, 1.000000000000000000, 0.9238795325112869605, 1.000000000000000000, 0.9238795325112869605, 1.000000000000000000, 0.9238795325112869605, 1.000000000000000000, 0.9238795325112869605, 1.000000000000000000, 0.9238795325112869605, 1.000000000000000000, 0.9238795325112869605, 1.000000000000000000, 0.9238795325112869605, 1.000000000000000000, 0.9238795325112869605, 1.000000000000000000, 0.9238795325112869605, 1.000000000000000000, 0.9238795325112869605, 1.000000000000000000, 0.9238795325112869605, 1.000000000000000000, 0.9238795325112869605, 1.000000000000000000, 0.9238795325112869605, 1.000000000000000000, 0.9238795325112869605, 1.000000000000000000, 0.9238795325112869605, 1.000000000000000000, 0.9238795325112869605, 1.000000000000000000, 0.9238795325112869605, 1.000000000000000000, 0.9238795325112869605, 1.000000000000000000, 0.9238795325112869605, 1.000000000000000000, 0.9238795325112869605, 1.000000000000000000, 0.9238795325112869605, 1.000000000000000000, 0.9238795325112869605, 1.000000000000000000, 0.9238795325112869605, 1.000000000000000000, 0.9238795325112869605, 1.000000000000000000, 0.9238795325112869605, 1.000000000000000000, 0.9238795325112869605, 1.000000000000000000, 0.9238795325112869605, 1.000000000000000000, 0.9238795325112869605, 1.000000000000000000, 0.9238795325112869605, 1.000000000000000000, 0.9238795325112869605, 1.000000000000000000, 0.9238795325112869605, 1.000000000000000000, 0.9238795325112869605, 1.000000000000000000, 0.9238795325112869605, 1.000000000000000000, 0.9238795325112869605, 1.000000000000000000, 0.9238795325112869605, 1.000000000000000000, 0.9238795325112869605, 1.000000000000000000, 0.9238795325112869605, 1.000000000000000000, 0.9238795325112869605, 1.000000000000000000, 0.9238795325112869605, 1.000000000000000000, 0.9238795325112869605, 1.000000000000000000, 0.9238795325112869605, 1.000000000000000000, 0.9238795325112869605, 1.000000000000000000, 0.9238795325112869605, 1.000000000000000000, 0.9238795325112869605, 1.000000000000000000, 0.9238795325112869605, 1.000000000000000000, 0.9238795325112869605, 1.000000000000000000, 0.9238795325112869605, 1.000000000000000000, 0.9238795325112869605, 1.000000000000000000, 0.9238795325112869605, 1.000000000000000000, 0.9238795325112869605, 1.000000000000000000, 0.9238795325112869605, 1.000000000000000000, 0.9238795325112869605, 1.000000000000000000, 0.9238795325112869605, 1.000000000000000000, 0.9238795325112869605, 1.000000000000000000, 0.9238795325112869605, 1.000000000000000000, 0.9238795325112869605, 1.000000000000000000, 0.9238795325112869605, 1.000000000000000000, 0.9238795325112869605, 1.000000000000000000, 0.9238795325112869605, 1.000000000000000000, 0.9238795325112869605, 1.000000000000000000, 0.9238795325112869605, 1.000000000000000000, 0.9238795325112869605, 1.000000000000000000, 0.9238795325112869605, 1.000000000000000000, 0.9238795325112869605, 1.000000000000000000, 0.9238795325112869605, 1.000000000000000000, 0.9238795325112869605, 1.000000000000000000, 0.9238795325112869605, 1.000000000000000000, 0.9238795325112869605, 1.000000000000000000, 0.9238795325112869605, 1.000000000000000000, 0.9238795325112869605, 1.000000000000000000, 0.9238795325112869605, 1.000000000000000000, 0.9238795325112869605, 1.000000000000000000, 0.9238795325112869605, 1.000000000000000000, 0.9238795325112869605, 1.000000000000000000, 0.9238795325112869605, 1.000000000000000000, 0.9238795325112869605, 1.000000000000000000, 0.9238795325112869605, 1.000000000000000000, 0.9238795325112869605, 1.000000000000000000, 0.9238795325112869605, 1.000000000000000000, 0.9238795325112869605, 1.000000000000000000, 0.9238795325112869605, 1.000000000000000000, 0.9238795325112869605, 1.000000000000000000, 0.9238795325112869605, 1.000000000000000000, 0.9238795325112869605, 1.000000000000000000, 0.9238795325112869605, 1.000000000000000000, 0.9238795325112869605, 1.000000000000000000, 0.9238795325112869605, 1.000000000000000000, 0.9238795325112869605, 1.000000000000000000, 0.9238795325112869605, 1.000000000000000000),
 ( 1.000000000000000000, 0.9238795325112869605, 1.000000000000000000, 0.9238795325112869605, 1.000000000000000000, 0.9238795325112869605, 1.000000000000000000, 0.9238795325112869605, 1.000000000000000000, 0.9238795325112869605, 1.000000000000000000, 0.9238795325112869605, 1.000000000000000000, 0.9238795325112869605, 1.000000000000000000, 0.9238795325112869605, 1.000000000000000000, 0.9238795325112869605, 1.000000000000000000, 0.9238795325112869605, 1.000000000000000000, 0.9238795325112869605, 1.000000000000000000, 0.9238795325112869605, 1.000000000000000000, 0.9238795325112869605, 1.000000000000000000, 0.9238795325112869605, 1.000000000000000000, 0.9238795325112869605, 1.000000000000000000, 0.9238795325112869605, 1.000000000000000000, 0.9238795325112869605, 1.000000000000000000, 0.9238795325112869605, 1.000000000000000000, 0.9238795325112869605, 1.000000000000000000, 0.9238795325112869605, 1.000000000000000000, 0.9238795325112869605, 1.000000000000000000, 0.9238795325112869605, 1.000000000000000000, 0.9238795325112869605, 1.000000000000000000, 0.9238795325112869605, 1.000000000000000000, 0.9238795325112869605, 1.000000000000000000, 0.9238795325112869605, 1.000000000000000000, 0.9238795325112869605, 1.000000000000000000, 0.9238795325112869605, 1.000000000000000000, 0.9238795325112869605, 1.000000000000000000, 0.9238795325112869605, 1.000000000000000000, 0.9238795325112869605, 1.000000000000000000, 0.9238795325112869605, 1.000000000000000000, 0.9238795325112869605, 1.000000000000000000, 0.9238795325112869605, 1.000000000000000000, 0.9238795325112869605, 1.000000000000000000, 0.9238795325112869605, 1.000000000000000000, 0.9238795325112869605, 1.000000000000000000, 0.9238795325112869605, 1.000000000000000000, 0.9238795325112869605, 1.000000000000000000, 0.9238795325112869605, 1.000000000000000000, 0.9238795325112869605, 1.000000000000000000, 0.9238795325112869605, 1.000000000000000000, 0.9238795325112869605, 1.000000000000000000, 0.9238795325112869605, 1.000000000000000000, 0.9238795325112869605, 1.000000000000000000, 0.9238795325112869605, 1.000000000000000000, 0.9238795325112869605, 1.000000000000000000, 0.9238795325112869605, 1.000000000000000000, 0.9238795325112869605, 1.000000000000000000, 0.9238795325112869605, 1.000000000000000000, 0.9238795325112869605, 1.000000000000000000, 0.9238795325112869605, 1.000000000000000000, 0.9238795325112869605, 1.000000000000000000, 0.9238795325112869605, 1.000000000000000000, 0.9238795325112869605, 1.000000000000000000, 0.9238795325112869605, 1.000000000000000000, 0.9238795325112869605, 1.000000000000000000, 0.9238795325112869605, 1.000000000000000000, 0.9238795325112869605, 1.000000000000000000, 0.9238795325112869605, 1.000000000000000000, 0.9238795325112869605, 1.000000000000000000, 0.9238795325112869605, 1.000000000000000000, 0.9238795325112869605, 1.000000000000000000, 0.9238795325112869605, 1.000000000000000000, 0.9238795325112869605, 1.000000000000000000, 0.9238795325112869605, 1.000000000000000000, 0.9238795325112869605, 1.000000000000000000, 0.9238795325112869605, 1.000000000000000000, 0.9238795325112869605, 1.000000000000000000, 0.9238795325112869605, 1.000000000000000000, 0.9238795325112869605, 1.000000000000000000, 0.9238795325112869605, 1.000000000000000000, 0.9238795325112869605, 1.000000000000000000, 0.9238795325112869605, 1.000000000000000000, 0.9238795325112869605, 1.000000000000000000, 0.9238795325112869605, 1.000000000000000000, 0.9238795325112869605, 1.000000000000000000, 0.9238795325112869605, 1.000000000000000000, 0.9238795325112869605, 1.000000000000000000, 0.9238795325112869605, 1.000000000000000000, 0.9238795325112869605, 1.000000000000000000, 0.9238795325112869605, 1.000000000000000000, 0.9238795325112869605, 1.000000000000000000, 0.9238795325112869605, 1.000000000000000000, 0.9238795325112869605, 1.000000000000000000, 0.9238795325112869605, 1.000000000000000000, 0.9238795325112869605, 1.000000000000000000, 0.9238795325112869605, 1.000000000000000000, 0.9238795325112869605, 1.000000000000000000, 0.9238795325112869605, 1.000000000000000000, 0.9238795325112869605, 1.000000000000000000, 0.9238795325112869605, 1.000000000000000000, 0.9238795325112869605, 1.000000000000000000, 0.9238795325112869605, 1.000000000000000000, 0.9238795325112869605, 1.000000000000000000, 0.9238795325112869605, 1.000000000000000000, 0.9238795325112869605, 1.000000000000000000, 0.9238795325112869605, 1.000000000000000000, 0.9238795325112869605, 1.000000000000000000, 0.9238795325112869605, 1.000000000000000000, 0.9238795325112869605, 1.000000000000000000, 0.9238795325112869605, 1.000000000000000000, 0.9238795325112869605, 1.000000000000000000, 0.9238795325112869605, 1.000000000000000000, 0.9238795325112869605, 1.000000000000000000, 0.9238795325112869605, 1.000000000000000000, 0.9238795325112869605, 1.000000000000000000, 0.9238795325112869605, 1.000000000000000000, 0.9238795325112869605, 1.000000000000000000, 0.9238795325112869605, 1.000000000000000000, 0.9238795325112869605, 1.000000000000000000, 0.9238795325112869605, 1.000000000000000000, 0.9238795325112869605, 1.000000000000000000, 0.9238795325112869605, 1.000000000000000000, 0.9238795325112869605, 1.000000000000000000, 0.9238795325112869605, 1.000000000000000000, 0.9238795325112869605, 1.000000000000000000, 0.9238795325112869605, 1.000000000000000000, 0.9238795325112869605, 1.000000000000000000, 0.9238795325112869605, 1.000000000000000000, 0.9238795325112869605, 1.000000000000000000, 0.9238795325112869605, 1.000000000000000000, 0.9238795325112869605, 1.000000000000000000, 0.9238795325112869605, 1.000000000000000000, 0.9238795325112869605, 1.000000000000000000, 0.9238795325112869605, 1.000000000000000000, 0.9238795325112869605, 1.000000000000000000, 0.9238795325112869605, 1.000000000000000000) ) ) 
 REPRESENTATION_ITEM ( '' )  SURFACE ( )  );
#12726 = CARTESIAN_POINT ( 'NONE',  ( 123.1205148109119563, -7.643976991954077427, -18.09477374809248928 ) ) ;
#12727 = CARTESIAN_POINT ( 'NONE',  ( 124.9924948109119924, -4.089484607189486809, -7.948022111789456723 ) ) ;
#12728 = CARTESIAN_POINT ( 'NONE',  ( 115.3442858795247759, -0.7896495226426338832, -17.46756447353520159 ) ) ;
#12729 = CARTESIAN_POINT ( 'NONE',  ( 109.9269421295247753, -9.868328341294093420, -13.39321520033831447 ) ) ;
#12730 = CARTESIAN_POINT ( 'NONE',  ( 83.14901522432917602, -31.89413582345784803, -23.38874658933293560 ) ) ;
#12731 = AXIS2_PLACEMENT_3D ( 'NONE', #36959, #5730, #19650 ) ;
#12732 = CARTESIAN_POINT ( 'NONE',  ( 117.2209414775786485, -2.084020599724406786, -8.691656652584148546 ) ) ;
#12733 = CARTESIAN_POINT ( 'NONE',  ( 115.0653281442453277, -3.505236298600246325, -18.68346056562440793 ) ) ;
#12734 = CARTESIAN_POINT ( 'NONE',  ( 41.72636039845269096, -11.37347657059392070, -17.89321520033831447 ) ) ;
#12735 = CARTESIAN_POINT ( 'NONE',  ( 114.2330358795247776, -8.402594152722688392, -9.854619843455216355 ) ) ;
#12736 = ORIENTED_EDGE ( 'NONE', *, *, #42339, .F. ) ;
#12737 = CARTESIAN_POINT ( 'NONE',  ( 122.8368814775786291, -7.894159318335801423, -9.358103419637830100 ) ) ;
#12738 = CARTESIAN_POINT ( 'NONE',  ( 126.4673881442452910, -7.894159318335828068, -9.358103419637847864 ) ) ;
#12739 = CARTESIAN_POINT ( 'NONE',  ( 120.6463454359119822, 0.5291689781388270175, -13.89700978578772705 ) ) ;
#12740 = CARTESIAN_POINT ( 'NONE',  ( 122.3826735609119680, 0.6414057260225851653, -11.69287257290600657 ) ) ;
#12741 = ORIENTED_EDGE ( 'NONE', *, *, #25298, .F. ) ;
#12742 = CARTESIAN_POINT ( 'NONE',  ( 70.19189222814998175, -51.12070001563444066, -33.65111096193285078 ) ) ;
#12743 = TOROIDAL_SURFACE ( 'NONE', #44054, 33.80000000000000426, 1.199999999999999956 ) ;
#12744 = CARTESIAN_POINT ( 'NONE',  ( 116.9654664325269238, -11.55218184020096395, -21.57977077210596306 ) ) ;
#12745 = ORIENTED_EDGE ( 'NONE', *, *, #15835, .F. ) ;
#12746 = CARTESIAN_POINT ( 'NONE',  ( 118.4689281442453392, 0.9020085738987339008, -11.91225656197089222 ) ) ;
#12747 = CARTESIAN_POINT ( 'NONE',  ( 123.5743281442453139, -2.084020599724406786, -8.691656652584148546 ) ) ;
#12748 = CARTESIAN_POINT ( 'NONE',  ( 113.8173414775786512, -9.565557343593413364, -10.61323700422348004 ) ) ;
#12749 =( NAMED_UNIT ( * ) SI_UNIT ( $, .STERADIAN. ) SOLID_ANGLE_UNIT ( ) );
#12750 = DIRECTION ( 'NONE',  ( 0.000000000000000000, 0.000000000000000000, -1.000000000000000000 ) ) ;
#12751 = DIRECTION ( 'NONE',  ( 0.000000000000000000, 0.000000000000000000, 1.000000000000000000 ) ) ;
#12752 = CARTESIAN_POINT ( 'NONE',  ( 113.2500748109119968, -6.344957434206662583, -7.627207830600332805 ) ) ;
#12753 = CARTESIAN_POINT ( 'NONE',  ( 110.8298327545248299, -6.936859964151250502, -8.388885654883777576 ) ) ;
#12754 = CARTESIAN_POINT ( 'NONE',  ( 125.0492214775786266, -6.344957434206665248, -7.627207830600338134 ) ) ;
#12755 = CARTESIAN_POINT ( 'NONE',  ( 121.9470836909669913, -25.99489077589524300, -13.39321520033831447 ) ) ;
#12756 = ORIENTED_EDGE ( 'NONE', *, *, #851, .F. ) ;
#12757 = CARTESIAN_POINT ( 'NONE',  ( 114.3846081442453197, -10.63000616557722466, -14.87417383870573495 ) ) ;
#12758 = EDGE_CURVE ( 'NONE', #7750, #30137, #22972, .T. ) ;
#12759 = EDGE_CURVE ( 'NONE', #23986, #25646, #23449, .T. ) ;
#12760 = CARTESIAN_POINT ( 'NONE',  ( 115.5758681442453053, -7.894159318335828068, -9.358103419637847864 ) ) ;
#12761 = CARTESIAN_POINT ( 'NONE',  ( 127.0264730702704838, -4.566927068118824984, -18.78905399823883826 ) ) ;
#12762 = CARTESIAN_POINT ( 'NONE',  ( 111.8319081442453182, -5.638512984488999180, -18.83840828888717311 ) ) ;
#12763 = CIRCLE ( 'NONE', #20056, 2.999999999999999556 ) ;
#12764 = ORIENTED_EDGE ( 'NONE', *, *, #34740, .T. ) ;
#12765 = CARTESIAN_POINT ( 'NONE',  ( 123.1772414775786189, -4.089484607189486809, -7.948022111789456723 ) ) ;
#12766 = DIRECTION ( 'NONE',  ( -0.000000000000000000, -0.9284778069183718952, -0.3713878862591649677 ) ) ;
#12767 = CARTESIAN_POINT ( 'NONE',  ( 110.3436608795247764, -1.325403438956436419, -16.93181055722137174 ) ) ;
#12768 = CARTESIAN_POINT ( 'NONE',  ( 70.19189222814998175, -56.33107134722149567, -35.73524133214168330 ) ) ;
#12769 = CARTESIAN_POINT ( 'NONE',  ( 137.4282737236246987, -3.645634682062916188, -8.450363672471354448 ) ) ;
#12770 = CIRCLE ( 'NONE', #31692, 2.000000000000000444 ) ;
#12771 = CARTESIAN_POINT ( 'NONE',  ( 113.6471614775786492, -4.153390946401321671, -8.397313243818183892 ) ) ;
#12772 = CARTESIAN_POINT ( 'NONE',  ( 91.11246428952674137, -25.99489077589524300, -13.39321520033831625 ) ) ;
#12773 = CARTESIAN_POINT ( 'NONE',  ( 125.3563243388396984, -2.728216552653024873, -20.10610198443428231 ) ) ;
#12774 = CARTESIAN_POINT ( 'NONE',  ( 115.6893214775786447, -9.859900752359374465, -12.68260735090039404 ) ) ;
#12775 = CARTESIAN_POINT ( 'NONE',  ( 115.9729548109119861, -6.344957434206662583, -7.627207830600332805 ) ) ;
#12776 = CARTESIAN_POINT ( 'NONE',  ( 122.1743141859119817, -8.321307733199551748, -9.223433127585318303 ) ) ;
#12777 = CARTESIAN_POINT ( 'NONE',  ( 113.7038881442453402, -3.383040157471821630, -19.15922257007629170 ) ) ;
#12778 = CARTESIAN_POINT ( 'NONE',  ( 114.2144281442453178, -1.833838273342658809, -17.42832698103878286 ) ) ;
#12779 = CARTESIAN_POINT ( 'NONE',  ( 123.0070614775786169, 0.9020085738987339008, -11.91225656197089222 ) ) ;
#12780 = CARTESIAN_POINT ( 'NONE',  ( 122.6667014775786413, -7.893985811506177619, -18.51759400769804742 ) ) ;
#12781 = VERTEX_POINT ( 'NONE', #42500 ) ;
#12782 = CARTESIAN_POINT ( 'NONE',  ( 112.3991748109119868, -8.166667518702817929, -8.995218007635859436 ) ) ;
#12783 = CARTESIAN_POINT ( 'NONE',  ( 110.4825671295247815, -10.62599879583958540, -13.39321520033831447 ) ) ;
#12784 = ADVANCED_FACE ( 'NONE', ( #8060 ), #25618, .F. ) ;
#12785 = CARTESIAN_POINT ( 'NONE',  ( 105.9681140045248355, 0.1403307496149616695, -15.46607636864997204 ) ) ;
#12786 = CARTESIAN_POINT ( 'NONE',  ( 107.6349890045248401, -9.868328341294098749, -11.32035403202665869 ) ) ;
#12787 = DIRECTION ( 'NONE',  ( -0.9609149988134837450, 0.1028163501681639419, -0.2570431154366518145 ) ) ;
#12788 = CARTESIAN_POINT ( 'NONE',  ( 119.7169148109119874, -9.988377603198976828, -10.36322818467138340 ) ) ;
#12789 = ORIENTED_EDGE ( 'NONE', *, *, #20009, .T. ) ;
#12790 = CARTESIAN_POINT ( 'NONE',  ( 77.77634386988383142, 3.254514819260860392, -4.893215200338314474 ) ) ;
#12791 = CARTESIAN_POINT ( 'NONE',  ( 124.6713397424434078, -0.9924539043446091169, -17.29976612834908423 ) ) ;
#12792 = CARTESIAN_POINT ( 'NONE',  ( 116.1431348109119881, 0.1319031606808879209, -14.10382304977623669 ) ) ;
#12793 = EDGE_CURVE ( 'NONE', #3055, #45059, #29896, .T. ) ;
#12794 = CARTESIAN_POINT ( 'NONE',  ( 107.0099108795247815, -1.325403438956436419, -16.93181055722141792 ) ) ;
#12795 = CARTESIAN_POINT ( 'NONE',  ( 119.4900081442453086, -1.834011780172310813, -8.268836392978581529 ) ) ;
#12796 = EDGE_CURVE ( 'NONE', #25152, #26514, #11490, .T. ) ;
#12797 = CARTESIAN_POINT ( 'NONE',  ( 107.8433483795247838, -0.7896495226426338832, -9.318865927141430916 ) ) ;
#12798 = DIRECTION ( 'NONE',  ( -0.1352586133457944206, -0.9908103287288505534, 0.000000000000000000 ) ) ;
#12799 = AXIS2_PLACEMENT_3D ( 'NONE', #1697, #14946, #29523 ) ;
#12800 = EDGE_LOOP ( 'NONE', ( #17293, #17160, #29262 ) ) ;
#12801 = CYLINDRICAL_SURFACE ( 'NONE', #505, 1.587500000000000355 ) ;
#12802 = CARTESIAN_POINT ( 'NONE',  ( 121.3619881442452879, -5.574606645277164318, -18.38911715685844683 ) ) ;
#12803 = CARTESIAN_POINT ( 'NONE',  ( 120.9649014775786355, -3.383040157471821630, -19.15922257007629170 ) ) ;
#12804 = CARTESIAN_POINT ( 'NONE',  ( 112.6828081442453282, -2.084020599724406786, -8.691656652584148546 ) ) ;
#12805 = CARTESIAN_POINT ( 'NONE',  ( 115.9729548109119861, -6.344957434206662583, -7.627207830600332805 ) ) ;
#12806 = DIRECTION ( 'NONE',  ( 0.000000000000000000, 0.000000000000000000, 1.000000000000000000 ) ) ;
#12807 = CARTESIAN_POINT ( 'NONE',  ( 126.3063647503471998, -1.053199401995885021, -10.08875103278353258 ) ) ;
#12808 = CARTESIAN_POINT ( 'NONE',  ( 118.7525614775786380, -1.833838273342659253, -17.42832698103878286 ) ) ;
#12809 = ORIENTED_EDGE ( 'NONE', *, *, #28101, .F. ) ;
#12810 = AXIS2_PLACEMENT_3D ( 'NONE', #16528, #41154, #10361 ) ;
#12811 = ADVANCED_FACE ( 'NONE', ( #7836 ), #21516, .T. ) ;
#12812 = CARTESIAN_POINT ( 'NONE',  ( 119.7736414775786358, -10.30919188438809719, -12.61870101168856273 ) ) ;
#12813 = CARTESIAN_POINT ( 'NONE',  ( 114.6682414775786469, -1.561330072975668060, -17.79121239304076596 ) ) ;
#12814 = CARTESIAN_POINT ( 'NONE',  ( 120.7947214775786193, -0.8288870151387760510, -10.36305467784173118 ) ) ;
#12815 = ORIENTED_EDGE ( 'NONE', *, *, #8010, .T. ) ;
#12816 = ADVANCED_FACE ( 'NONE', ( #25395 ), #31546, .T. ) ;
#12817 = CARTESIAN_POINT ( 'NONE',  ( 124.4662673109119737, -9.289237151508434209, -11.05642687123711276 ) ) ;
#12818 = ADVANCED_FACE ( 'NONE', ( #21289 ), #39523, .T. ) ;
#12819 = EDGE_CURVE ( 'NONE', #27420, #38550, #14453, .T. ) ;
#12820 = CARTESIAN_POINT ( 'NONE',  ( 117.6180281442453150, -0.4660016031367893996, -10.09054647747474043 ) ) ;
#12821 = CARTESIAN_POINT ( 'NONE',  ( 112.9828796295247884, -4.863998795839590272, -19.15521520033831493 ) ) ;
#12822 = CARTESIAN_POINT ( 'NONE',  ( 116.1998614775786507, 0.4262465694468514643, -12.03445270309931736 ) ) ;
#12823 = ORIENTED_EDGE ( 'NONE', *, *, #42931, .F. ) ;
#12824 = VERTEX_POINT ( 'NONE', #4408 ) ;
#12825 = CARTESIAN_POINT ( 'NONE',  ( 111.7184548109119788, -9.261995988541697145, -16.69588392320189030 ) ) ;
#12826 = AXIS2_PLACEMENT_3D ( 'NONE', #5374, #1946, #19059 ) ;
#12827 = CARTESIAN_POINT ( 'NONE',  ( 119.7736414775786358, 0.1319031606808879209, -14.10382304977623669 ) ) ;
#12828 = FACE_OUTER_BOUND ( 'NONE', #15522, .T. ) ;
#12829 = CARTESIAN_POINT ( 'NONE',  ( 82.31000308962319423, -13.76004065658516673, -18.64321520033831803 ) ) ;
#12830 = CARTESIAN_POINT ( 'NONE',  ( 117.2776681442452968, -5.638512984488999180, -18.83840828888717311 ) ) ;
#12831 = CONICAL_SURFACE ( 'NONE', #38288, 2.445500000000004448, 0.9599310885968757034 ) ;
#12832 = CARTESIAN_POINT ( 'NONE',  ( 108.7462390045248242, 0.8980012041604421569, -15.77991374673208469 ) ) ;
#12833 = CARTESIAN_POINT ( 'NONE',  ( 120.1707281442453166, 0.2603800115204892296, -16.42320221600525088 ) ) ;
#12835 = CARTESIAN_POINT ( 'NONE',  ( 117.1642148109119859, -0.8288870151387760510, -10.36305467784173118 ) ) ;
#12834 = CARTESIAN_POINT ( 'NONE',  ( 117.0507614775786465, -10.30919188438810075, -12.61870101168855918 ) ) ;
#12836 = DIRECTION ( 'NONE',  ( 0.9609149988134843001, -0.1028163501681632064, 0.2570431154366505933 ) ) ;
#12837 = CARTESIAN_POINT ( 'NONE',  ( 70.19189222814998175, -57.05206236706784040, -36.02363522683400276 ) ) ;
#12838 = ORIENTED_EDGE ( 'NONE', *, *, #39328, .F. ) ;
#12839 = AXIS2_PLACEMENT_3D ( 'NONE', #35163, #28581, #7826 ) ;
#12840 = CARTESIAN_POINT ( 'NONE',  ( 123.2339681442453241, -3.505236298600246325, -18.68346056562440793 ) ) ;
#12841 = CARTESIAN_POINT ( 'NONE',  ( 122.8560864091100626, -0.9924539043446216624, -17.29976612834909133 ) ) ;
#12842 = DIRECTION ( 'NONE',  ( 0.000000000000000000, 0.3818493186865929423, -0.9242245927363027524 ) ) ;
#12843 = CARTESIAN_POINT ( 'NONE',  ( 114.5108483795247878, -0.7896495226426338832, -9.318865927141430916 ) ) ;
#12844 = CARTESIAN_POINT ( 'NONE',  ( 111.7327233795247849, -1.325403438956436419, -9.854619843455211026 ) ) ;
#12845 = CARTESIAN_POINT ( 'NONE',  ( 111.5938171295247940, -10.62599879583958540, -13.39321520033831447 ) ) ;
#12846 = AXIS2_PLACEMENT_3D ( 'NONE', #26201, #4766, #36225 ) ;
#12847 = CARTESIAN_POINT ( 'NONE',  ( 123.6877814775786533, -3.383040157471821630, -19.15922257007629170 ) ) ;
#12848 = VERTEX_POINT ( 'NONE', #18323 ) ;
#12849 = CARTESIAN_POINT ( 'NONE',  ( 120.1707281442453166, 0.2603800115204892296, -16.42320221600525088 ) ) ;
#12850 = DIRECTION ( 'NONE',  ( 1.000000000000000000, 0.000000000000000000, 0.000000000000000000 ) ) ;
#12851 = CARTESIAN_POINT ( 'NONE',  ( 65.08556096878474762, -20.51665340220043277, -5.893215200338312698 ) ) ;
#12852 = CARTESIAN_POINT ( 'NONE',  ( 121.3052614775786111, -1.834011780172310813, -8.268836392978581529 ) ) ;
#12853 = CARTESIAN_POINT ( 'NONE',  ( 120.3409081442453044, -0.4660016031367893996, -10.09054647747474043 ) ) ;
#12854 = CARTESIAN_POINT ( 'NONE',  ( 64.04848551113317967, -2.916203086156882840, -18.83592047541311132 ) ) ;
#12855 = CARTESIAN_POINT ( 'NONE',  ( 123.0070614775786169, -10.15424416112533912, -14.75197769757731336 ) ) ;
#12856 = CARTESIAN_POINT ( 'NONE',  ( 96.23375075340858587, -26.75621354156143994, -11.55051655297938318 ) ) ;
#12857 = CARTESIAN_POINT ( 'NONE',  ( 122.6604860609119640, -3.387241619883791355, -18.17469012370385073 ) ) ;
#12858 = ORIENTED_EDGE ( 'NONE', *, *, #17794, .T. ) ;
#12859 = CARTESIAN_POINT ( 'NONE',  ( 87.14323352029596492, -25.99489077589524300, -13.39321520033831625 ) ) ;
#12860 = CARTESIAN_POINT ( 'NONE',  ( 118.6164486996681973, -1.172797794773247304, -17.05961127468924587 ) ) ;
#12861 = CARTESIAN_POINT ( 'NONE',  ( 123.8579614775786126, -9.859900752359378018, -12.68260735090039759 ) ) ;
#12862 = AXIS2_PLACEMENT_3D ( 'NONE', #41799, #16730, #27440 ) ;
#12863 = CARTESIAN_POINT ( 'NONE',  ( 109.3713171295247832, 0.1403307496149613920, -13.39321520033831447 ) ) ;
#12864 = CARTESIAN_POINT ( 'NONE',  ( 112.0799890045248475, -9.868328341294098749, -11.32035403202665869 ) ) ;
#12865 = CARTESIAN_POINT ( 'NONE',  ( 117.2209414775786485, -2.084020599724406786, -8.691656652584148546 ) ) ;
#12866 = CARTESIAN_POINT ( 'NONE',  ( 64.17717360238856372, -55.76310523276723075, -40.89321520033833224 ) ) ;
#12867 = CARTESIAN_POINT ( 'NONE',  ( 68.68839935636917460, -25.95913848132418522, -5.893215200338315363 ) ) ;
#12868 = CARTESIAN_POINT ( 'NONE',  ( 113.5904348109119866, -2.084020599724406786, -8.691656652584148546 ) ) ;
#12869 = CARTESIAN_POINT ( 'NONE',  ( 122.1561614775786353, -0.4660016031367893996, -10.09054647747474043 ) ) ;
#12871 = VERTEX_POINT ( 'NONE', #44472 ) ;
#12870 = ADVANCED_FACE ( 'NONE', ( #24707 ), #23521, .T. ) ;
#12872 = AXIS2_PLACEMENT_3D ( 'NONE', #35278, #194, #14110 ) ;
#12873 = CARTESIAN_POINT ( 'NONE',  ( 121.7590748109119687, -2.084020599724406786, -8.691656652584148546 ) ) ;
#12874 = CARTESIAN_POINT ( 'NONE',  ( 115.4624148109119943, -5.638512984488999180, -18.83840828888717311 ) ) ;
#12875 = CARTESIAN_POINT ( 'NONE',  ( 123.8579614775786126, 0.5811942927096110934, -14.16772938898807510 ) ) ;
#12876 = CARTESIAN_POINT ( 'NONE',  ( 123.9714148109119805, -8.899110576539710493, -16.42337572283490132 ) ) ;
#12877 = VERTEX_POINT ( 'NONE', #13011 ) ;
#12878 = CARTESIAN_POINT ( 'NONE',  ( 120.7157985609119635, -0.08252387247371148482, -11.91645802438286772 ) ) ;
#12879 = CARTESIAN_POINT ( 'NONE',  ( 122.2128881442453263, -1.834011780172310813, -8.268836392978581529 ) ) ;
#12880 = CARTESIAN_POINT ( 'NONE',  ( 114.4413348109119823, -0.8288870151387760510, -10.36305467784173118 ) ) ;
#12881 = CARTESIAN_POINT ( 'NONE',  ( 125.8433948109119456, -1.834011780172310813, -8.268836392978581529 ) ) ;
#12882 = ADVANCED_FACE ( 'NONE', ( #16657 ), #37836, .F. ) ;
#12883 = CARTESIAN_POINT ( 'NONE',  ( 105.9681140045248355, -10.62599879583958717, -11.00651665394454604 ) ) ;
#12884 = DIRECTION ( 'NONE',  ( 1.000000000000000000, 0.000000000000000000, 0.000000000000000000 ) ) ;
#12885 = ORIENTED_EDGE ( 'NONE', *, *, #13638, .F. ) ;
#12886 = DIRECTION ( 'NONE',  ( 0.000000000000000000, 0.000000000000000000, 1.000000000000000000 ) ) ;
#12887 = CARTESIAN_POINT ( 'NONE',  ( 108.2600671295247992, 0.1403307496149613920, -13.39321520033831447 ) ) ;
#12888 = AXIS2_PLACEMENT_3D ( 'NONE', #5338, #42973, #29732 ) ;
#12889 = CARTESIAN_POINT ( 'NONE',  ( 67.19031194842951038, -1.707697914625855296, -14.39321520033831625 ) ) ;
#12890 = CARTESIAN_POINT ( 'NONE',  ( 117.6180281442453150, -8.899110576539710493, -16.42337572283490132 ) ) ;
#12891 = CARTESIAN_POINT ( 'NONE',  ( 113.7606148109119886, -7.894159318335828068, -9.358103419637847864 ) ) ;
#12892 = CARTESIAN_POINT ( 'NONE',  ( 126.7960359500334135, -6.485669677952845547, -18.42724950168021181 ) ) ;
#12893 = ORIENTED_EDGE ( 'NONE', *, *, #34453, .T. ) ;
#12894 = CARTESIAN_POINT ( 'NONE',  ( 63.69189222814998175, -62.82237896425675672, -47.71602681600972318 ) ) ;
#12895 = CARTESIAN_POINT ( 'NONE',  ( 116.5969481442453031, -9.859900752359374465, -12.68260735090039404 ) ) ;
#12896 = CARTESIAN_POINT ( 'NONE',  ( 112.9664414775786412, -9.859900752359374465, -12.68260735090039404 ) ) ;
#12897 = AXIS2_PLACEMENT_3D ( 'NONE', #41896, #2965, #35241 ) ;
#12898 = CARTESIAN_POINT ( 'NONE',  ( 67.96085940327634489, -0.5773760052095162632, -10.39321520033831447 ) ) ;
#12899 = PLANE ( 'NONE',  #28957 ) ;
#12901 = CARTESIAN_POINT ( 'NONE',  ( 121.7023481442452777, -9.261995988541697145, -16.69588392320189030 ) ) ;
#12900 = DIRECTION ( 'NONE',  ( -0.5040994586965557023, -0.8636456077245108220, 0.000000000000000000 ) ) ;
#12902 = CARTESIAN_POINT ( 'NONE',  ( 126.3539348109119800, -4.153390946401325223, -8.397313243818185668 ) ) ;
#12903 = ORIENTED_EDGE ( 'NONE', *, *, #44280, .F. ) ;
#12904 = LINE ( 'NONE', #1938, #22240 ) ;
#12905 = CARTESIAN_POINT ( 'NONE',  ( 127.3434826498001087, 0.3281563814195650464, -15.39656318237291366 ) ) ;
#12906 = CARTESIAN_POINT ( 'NONE',  ( 106.3848327545248651, -6.936859964151250502, -8.388885654883777576 ) ) ;
#12907 = CARTESIAN_POINT ( 'NONE',  ( 126.6942948109119840, -8.899110576539710493, -16.42337572283490132 ) ) ;
#12908 = AXIS2_PLACEMENT_3D ( 'NONE', #23424, #37074, #2886 ) ;
#12909 = CARTESIAN_POINT ( 'NONE',  ( 120.5110881442453206, -3.505236298600246325, -18.68346056562440793 ) ) ;
#12910 = DIRECTION ( 'NONE',  ( -0.2768435750659241079, -0.3568721902840695792, 0.8921882507333129819 ) ) ;
#12911 = CARTESIAN_POINT ( 'NONE',  ( 114.3719421295247827, -9.868328341294093420, -13.39321520033831447 ) ) ;
#12912 = DIRECTION ( 'NONE',  ( 0.5735764363510498232, -0.3127926500124802445, 0.7570804645221007600 ) ) ;
#12913 = CARTESIAN_POINT ( 'NONE',  ( 63.10250807381770244, -31.76310523276724140, -23.47900163796522222 ) ) ;
#12914 = CARTESIAN_POINT ( 'NONE',  ( 113.4769814775786330, 0.4262465694468514643, -12.03445270309931736 ) ) ;
#12915 = CARTESIAN_POINT ( 'NONE',  ( 112.3578015045248861, -2.477300249445798297, -7.631215200338321125 ) ) ;
#12916 = DIRECTION ( 'NONE',  ( 1.000000000000000000, 0.000000000000000000, 0.000000000000000000 ) ) ;
#12917 = CARTESIAN_POINT ( 'NONE',  ( 112.4272546295247821, -4.863998795839590272, -7.631215200338315796 ) ) ;
#12918 = CARTESIAN_POINT ( 'NONE',  ( 125.5030348109119558, -3.383040157471821630, -19.15922257007629170 ) ) ;
#12919 = CARTESIAN_POINT ( 'NONE',  ( 122.0994348109119443, 0.9020085738987339008, -11.91225656197089222 ) ) ;
#12920 = CARTESIAN_POINT ( 'NONE',  ( 55.68041887817022939, -39.85035523279287162, -9.393215200338314474 ) ) ;
#12921 = CARTESIAN_POINT ( 'NONE',  ( 118.1852948109119836, -5.638512984488999180, -18.83840828888717311 ) ) ;
#12922 = CARTESIAN_POINT ( 'NONE',  ( 112.0588148109119828, 0.5811942927096154232, -14.16772938898807155 ) ) ;
#12923 = VERTEX_POINT ( 'NONE', #37148 ) ;
#12924 = CARTESIAN_POINT ( 'NONE',  ( 113.8740681442453138, -9.859900752359374465, -12.68260735090039404 ) ) ;
#12925 = CARTESIAN_POINT ( 'NONE',  ( 126.0135748109119902, -8.166667518702819706, -8.995218007635861213 ) ) ;
#12926 = CARTESIAN_POINT ( 'NONE',  ( 119.7736414775786358, -10.30919188438810075, -12.61870101168855918 ) ) ;
#12927 = CARTESIAN_POINT ( 'NONE',  ( 113.6471614775786492, -5.638512984488999180, -18.83840828888717311 ) ) ;
#12928 = CARTESIAN_POINT ( 'NONE',  ( 112.9097148109120070, -9.565557343593413364, -10.61323700422348004 ) ) ;
#12929 = ORIENTED_EDGE ( 'NONE', *, *, #38158, .T. ) ;
#12930 = CARTESIAN_POINT ( 'NONE',  ( 119.4332814775786318, -8.899110576539710493, -16.42337572283490132 ) ) ;
#12931 = CARTESIAN_POINT ( 'NONE',  ( 123.6877814775786533, -3.383040157471821630, -19.15922257007629170 ) ) ;
#12932 = CARTESIAN_POINT ( 'NONE',  ( 111.1076452545248259, 0.8980012041604421569, -11.00651665394454071 ) ) ;
#12933 = ADVANCED_FACE ( 'NONE', ( #5923 ), #2205, .T. ) ;
#12934 = CARTESIAN_POINT ( 'NONE',  ( 123.5743281442453139, -2.084020599724406786, -8.691656652584148546 ) ) ;
#12935 = CARTESIAN_POINT ( 'NONE',  ( 116.8512505633842835, -0.6435572107194698077, -16.52836391485888612 ) ) ;
#12936 = CYLINDRICAL_SURFACE ( 'NONE', #5387, 1.499999999999999334 ) ;
#12937 = ORIENTED_EDGE ( 'NONE', *, *, #17770, .F. ) ;
#12938 = CARTESIAN_POINT ( 'NONE',  ( 121.2714235609119697, -9.645473719204776586, -14.86997237629376656 ) ) ;
#12939 = CARTESIAN_POINT ( 'NONE',  ( 122.9503348109119827, 0.5811942927096110934, -14.16772938898807510 ) ) ;
#12940 = CARTESIAN_POINT ( 'NONE',  ( 72.54180985774836188, -54.15757082072580175, -34.13667568191001322 ) ) ;
#12941 = CARTESIAN_POINT ( 'NONE',  ( 112.2857214775786474, -4.089484607189486809, -7.948022111789456723 ) ) ;
#12942 = CARTESIAN_POINT ( 'NONE',  ( 116.4006440670287219, 2.246832347042422739, -6.423500348738977017 ) ) ;
#12943 = CARTESIAN_POINT ( 'NONE',  ( 121.9470836909669913, -27.84333996136784961, -14.15691383771150136 ) ) ;
#12944 = CARTESIAN_POINT ( 'NONE',  ( 108.5378796295247810, -4.863998795839590272, -8.388885654883775800 ) ) ;
#12945 = CARTESIAN_POINT ( 'NONE',  ( 120.8933699480702586, -6.365377317481695663, -18.95617363400926081 ) ) ;
#12946 = CARTESIAN_POINT ( 'NONE',  ( 123.0077516859119839, -0.6942167230862511529, -9.935906262978004833 ) ) ;
#12947 = DIRECTION ( 'NONE',  ( 1.387778780781445676E-17, -0.9284778069183720062, -0.3713878862591650232 ) ) ;
#12948 = EDGE_CURVE ( 'NONE', #7488, #44558, #7322, .T. ) ;
#12950 = CARTESIAN_POINT ( 'NONE',  ( 124.5388954359119822, -10.25250061710393190, -12.88985647778305932 ) ) ;
#12949 = VECTOR ( 'NONE', #36134, 1000.000000000000000 ) ;
#12951 = CARTESIAN_POINT ( 'NONE',  ( 119.7169148109119874, -0.1624402480850797581, -16.17319339645315424 ) ) ;
#12952 = CARTESIAN_POINT ( 'NONE',  ( 119.7434548109119845, 0.2675062114431748794, -12.38956156844279910 ) ) ;
#12953 = ORIENTED_EDGE ( 'NONE', *, *, #27344, .T. ) ;
#12954 = CARTESIAN_POINT ( 'NONE',  ( 121.3619881442452879, -4.089484607189486809, -7.948022111789456723 ) ) ;
#12955 = CARTESIAN_POINT ( 'NONE',  ( 118.8660148109119774, -10.30919188438810075, -12.61870101168855918 ) ) ;
#12956 = CARTESIAN_POINT ( 'NONE',  ( 114.5803015045248117, -6.936859964151250502, -18.39754474579286025 ) ) ;
#12957 = CARTESIAN_POINT ( 'NONE',  ( 113.3068014775786594, -8.166667518702816153, -8.995218007635859436 ) ) ;
#12958 = CARTESIAN_POINT ( 'NONE',  ( 126.4106614775786284, -6.222761293078241884, -8.102969835052219238 ) ) ;
#12959 = CARTESIAN_POINT ( 'NONE',  ( 124.9357681442453014, -1.834011780172310813, -8.268836392978581529 ) ) ;
#12960 = CARTESIAN_POINT ( 'NONE',  ( 112.0105358795247810, -0.7896495226426338832, -17.46756447353520159 ) ) ;
#12961 = CARTESIAN_POINT ( 'NONE',  ( 107.7738952545248310, -9.868328341294098749, -15.46607636864997204 ) ) ;
#12962 = CARTESIAN_POINT ( 'NONE',  ( 123.9584548109119737, -12.80254289275730173, -14.38292102596908784 ) ) ;
#12963 = CARTESIAN_POINT ( 'NONE',  ( 115.2922348109119781, 0.4262465694468514643, -12.03445270309931736 ) ) ;
#12964 = CARTESIAN_POINT ( 'NONE',  ( 115.5191414775786569, -6.222761293078241884, -8.102969835052219238 ) ) ;
#12965 = CARTESIAN_POINT ( 'NONE',  ( 112.9865389883689915, 0.3193521225029610777, -12.14321520033829493 ) ) ;
#12966 = CARTESIAN_POINT ( 'NONE',  ( 112.5661608795247872, -1.325403438956436419, -16.93181055722141792 ) ) ;
#12967 = ORIENTED_EDGE ( 'NONE', *, *, #16682, .F. ) ;
#12968 = CARTESIAN_POINT ( 'NONE',  ( 109.2295115170851716, -0.2778941975186199898, -15.60097546659909540 ) ) ;
#12969 = CARTESIAN_POINT ( 'NONE',  ( 111.7751814775786556, -7.893985811506177619, -18.51759400769804742 ) ) ;
#12970 = CARTESIAN_POINT ( 'NONE',  ( 111.8319081442453182, -5.638512984488999180, -18.83840828888717311 ) ) ;
#12971 = CARTESIAN_POINT ( 'NONE',  ( 119.2572829359120021, -5.367793381288652910, -18.78638297431638904 ) ) ;
#12972 = CARTESIAN_POINT ( 'NONE',  ( 121.2714235609119697, -9.645473719204776586, -14.86997237629376656 ) ) ;
#12973 = ORIENTED_EDGE ( 'NONE', *, *, #40399, .F. ) ;
#12974 = CARTESIAN_POINT ( 'NONE',  ( 123.4976477054562594, -2.905774387498770928, -14.75189568944841056 ) ) ;
#12975 = CARTESIAN_POINT ( 'NONE',  ( 105.4124890045248293, -9.868328341294098749, -11.32035403202665869 ) ) ;
#12976 = VERTEX_POINT ( 'NONE', #37387 ) ;
#12977 = CARTESIAN_POINT ( 'NONE',  ( 116.9373081442452929, -8.166667518702817929, -8.995218007635861213 ) ) ;
#12978 = CARTESIAN_POINT ( 'NONE',  ( 125.3895814775786448, -2.084020599724406786, -8.691656652584148546 ) ) ;
#12979 = CARTESIAN_POINT ( 'NONE',  ( 114.8951481442453115, -8.899110576539710493, -16.42337572283490132 ) ) ;
#12980 = DIRECTION ( 'NONE',  ( 0.000000000000000000, 0.6004852223388321697, -0.7996358532186279566 ) ) ;
#12981 = CARTESIAN_POINT ( 'NONE',  ( 122.7234281442452755, -5.638512984488999180, -18.83840828888717311 ) ) ;
#12982 = CARTESIAN_POINT ( 'NONE',  ( 115.3489614775786407, -9.261995988541697145, -16.69588392320189030 ) ) ;
#12983 = B_SPLINE_CURVE_WITH_KNOTS ( 'NONE', 3,
 ( #14936, #28847, #29510, #12191, #21998, #35888, #11968, #36563, #4886, #15159 ),
 .UNSPECIFIED., .F., .F.,
 ( 4, 3, 3, 4 ),
 ( 0.000000000000000000, 0.0001671877560958114864, 0.0003343755126086585196, 0.0006438490228505489759 ),
 .UNSPECIFIED. ) ;
#12984 = CARTESIAN_POINT ( 'NONE',  ( 112.1494421295248003, -9.868328341294093420, -13.39321520033831447 ) ) ;
#12985 = CARTESIAN_POINT ( 'NONE',  ( 124.1415948109119540, -6.344957434206665248, -7.627207830600338134 ) ) ;
#12986 = EDGE_LOOP ( 'NONE', ( #29706, #33431, #10292, #20383 ) ) ;
#12987 = CARTESIAN_POINT ( 'NONE',  ( 116.1431348109119881, -10.30919188438810075, -12.61870101168855918 ) ) ;
#12988 = CARTESIAN_POINT ( 'NONE',  ( 115.7460481442453357, -10.15424416112533912, -14.75197769757731336 ) ) ;
#12989 = CARTESIAN_POINT ( 'NONE',  ( 126.5041214912219516, -4.953991576021822496, -18.53526297036774650 ) ) ;
#12990 = CARTESIAN_POINT ( 'NONE',  ( 113.5337081442453240, -9.261995988541697145, -16.69588392320189030 ) ) ;
#12991 = ORIENTED_EDGE ( 'NONE', *, *, #1868, .F. ) ;
#12992 = CARTESIAN_POINT ( 'NONE',  ( 120.2841814775786276, 0.9020085738987339008, -11.91225656197089222 ) ) ;
#12993 = FACE_OUTER_BOUND ( 'NONE', #20140, .T. ) ;
#12994 = DIRECTION ( 'NONE',  ( -0.000000000000000000, -0.9284778069183721172, -0.3713878862591650232 ) ) ;
#12995 = DIRECTION ( 'NONE',  ( 1.000000000000000000, 0.000000000000000000, 0.000000000000000000 ) ) ;
#12996 =( BOUNDED_SURFACE ( )  B_SPLINE_SURFACE ( 1, 2, ( 
 ( #44382, #20438, #13374, #40732, #44610, #27278, #16335, #9952, #19977, #9720, #44159, #3095, #27048, #23178, #44835, #13145, #40506, #23866, #37056, #30691, #37752, #40966, #30237, #17021, #37287, #13592, #9267, #23634, #2407, #9488, #12924, #26820, #23402, #6522, #2866, #6056, #34321, #30913, #27502, #20213, #12694, #26593, #33865, #2635, #37520, #16567, #33633, #16795, #5827, #19747, #30462, #34098, #20296, #34834, #6389, #23497, #27591, #37383, #16652, #17324, #31214, #16883, #30775, #44700, #17107, #30547, #2956, #38058, #27803, #41504, #6154, #6836, #34181, #38270, #44468, #7051, #45140, #27135, #13461, #27363, #3182, #10259, #20074, #33959, #3619, #28032, #24384, #17539, #41283, #20742, #41718, #23724, #20962, #34621, #2727, #10482, #31432, #13897, #10046, #3407, #199, #41058, #14115, #23950, #30997, #37615, #9581, #44923, #13233, #9815, #34401, #37831, #6608, #20521, #13681, #24166, #4288, #10923, #4743, #31882, #1323, #38488, #32105, #14339, #35285, #24825, #42162, #38716, #35748, #39177, #28253, #15017, #4521, #18663, #28705, #11596, #21852, #3838, #7487, #42385, #21404, #24605, #872, #15234, #41939, #35516, #647, #32556, #31655, #4058, #14562, #28481, #18444, #423, #32333, #11149, #7941, #1100, #28928, #17982, #39411, #42612, #8174, #17758, #25055, #7715, #42835, #38948, #25506, #18207, #10702, #7263, #21180, #21628, #14791, #35057, #22084, #35972, #11375, #25281, #19337, #23211, #16145, #19559, #15693, #33668, #5638, #5190, #2215, #37090, #29143, #36201, #19107, #12726, #33436, #40085, #32993, #30048, #43962, #15464, #22525, #5420, #8846, #33222, #25953, #19786, #25730, #39637, #1997, #1543, #22745, #4968, #40312, #1767, #36647, #18878, #15923, #39860, #26629, #40542, #29595, #9303, #22979, #29820, #36868, #43736, #5864, #2448, #8625, #43056, #11822, #29370, #8401, #43512, #12506, #43281, #22305, #26402, #32769, #12052, #9076, #36421, #12281, #26177, #10820, #17881, #24504, #31112, #24945, #6953, #21524, #12958, #7161, #33900, #10379, #45037, #17222 ),
 ( #549, #16368, #17437, #31555, #31330, #9525, #44196, #35182, #28368, #3519, #14017, #104, #17659, #27709, #42281, #13797, #30271, #34950, #26854, #23441, #24717, #38606, #24288, #38174, #20858, #38388, #37325, #34736, #323, #3959, #3736, #40767, #14236, #41623, #14461, #6096, #11043, #7382, #2670, #27932, #41841, #10601, #28152, #20017, #21073, #38841, #35411, #31778, #7610, #42062, #21299, #36314, #18331, #15583, #15361, #14684, #5084, #26070, #42733, #42951, #8737, #4186, #32224, #35861, #21750, #8294, #8071, #4863, #11717, #25628, #39974, #7844, #997, #1222, #21974, #22196, #32887, #762, #36092, #39750, #28598, #18556, #1439, #28823, #35641, #11498, #29487, #1661, #18781, #39301, #39533, #14912, #18104, #31999, #25403, #43400, #4635, #29042, #4417, #25177, #22645, #32448, #15136, #32671, #29266, #43178, #11946, #25842, #8518, #42509, #12168, #22421, #19000, #11269, #39075, #16035, #15809, #30395, #36983, #41124, #43623, #12397, #36541, #9883, #8970, #20145, #5315, #5752, #5984, #19672, #29710, #19231, #9646, #2797, #23103, #33560, #2337, #37212, #2107, #16724, #33333, #33112, #9414, #1882, #26297, #44317, #13073, #43856, #12628, #26526, #44087, #40204, #29943, #19909, #23568, #23326, #22869, #33794, #40435, #34029, #36762, #30619, #26972, #5531, #9196, #16266, #30170, #2566, #19450, #12852, #44536, #26753, #6221, #13298, #40660, #16495, #37449, #40893, #27206, #34898, #34253, #24667, #494, #17172, #17389, #28317, #23793, #6681, #10330, #41355, #27876, #27657, #24447, #31278, #52, #14407, #27433, #20589, #20807, #41570, #41790, #7330, #20366, #10547, #14181, #3026, #38124, #21025, #3246, #10112, #31061, #35127, #42229, #272, #13965, #34686, #21249, #31501, #44989, #17609, #28099, #24015, #42007, #24233, #38338, #37903, #3909, #7115, #16949, #37684, #3474, #30843, #10771, #44766, #38554, #17827, #3687, #34467, #31723, #13748, #6457, #13525, #6897, #28549, #4357, #25125, #11219, #39020, #4807, #8239, #42453, #29210, #18728, #18946, #42900, #25791, #36038 ) ),
 .UNSPECIFIED., .F., .F., .F. ) 
 B_SPLINE_SURFACE_WITH_KNOTS ( ( 2, 2 ),
 ( 3, 2, 2, 2, 2, 2, 2, 2, 2, 2, 2, 2, 2, 2, 2, 2, 2, 2, 2, 2, 2, 2, 2, 2, 2, 2, 2, 2, 2, 2, 2, 2, 2, 2, 2, 2, 2, 2, 2, 2, 2, 2, 2, 2, 2, 2, 2, 2, 2, 2, 2, 2, 2, 2, 2, 2, 2, 2, 2, 2, 2, 2, 2, 2, 2, 2, 2, 2, 2, 2, 2, 2, 2, 2, 2, 2, 2, 2, 2, 2, 2, 2, 2, 2, 2, 2, 2, 2, 2, 2, 2, 2, 2, 2, 2, 2, 2, 2, 2, 2, 2, 2, 2, 2, 2, 2, 2, 2, 2, 2, 2, 2, 2, 2, 2, 2, 2, 2, 2, 2, 2, 2, 2, 2, 2, 2, 2, 2, 3 ),
 ( 0.000000000000000000, 1.000000000000000000 ),
 ( 0.000000000000000000, 0.007812500000000000000, 0.01562500000000000000, 0.02343750000000000000, 0.03125000000000000000, 0.03906250000000000000, 0.04687500000000000000, 0.05468750000000000000, 0.06250000000000000000, 0.07031250000000000000, 0.07812500000000000000, 0.08593750000000000000, 0.09375000000000000000, 0.1015625000000000000, 0.1093750000000000000, 0.1171875000000000000, 0.1250000000000000000, 0.1328125000000000000, 0.1406250000000000000, 0.1484375000000000000, 0.1562500000000000000, 0.1640625000000000000, 0.1718750000000000000, 0.1796875000000000000, 0.1875000000000000000, 0.1953125000000000000, 0.2031250000000000000, 0.2109375000000000000, 0.2187500000000000000, 0.2265625000000000000, 0.2343750000000000000, 0.2421875000000000000, 0.2500000000000000000, 0.2578125000000000000, 0.2656250000000000000, 0.2734375000000000000, 0.2812500000000000000, 0.2890625000000000000, 0.2968750000000000000, 0.3046875000000000000, 0.3125000000000000000, 0.3203125000000000000, 0.3281250000000000000, 0.3359375000000000000, 0.3437500000000000000, 0.3515625000000000000, 0.3593750000000000000, 0.3671875000000000000, 0.3750000000000000000, 0.3828125000000000000, 0.3906250000000000000, 0.3984375000000000000, 0.4062500000000000000, 0.4140625000000000000, 0.4218750000000000000, 0.4296875000000000000, 0.4375000000000000000, 0.4453125000000000000, 0.4531250000000000000, 0.4609375000000000000, 0.4687500000000000000, 0.4765625000000000000, 0.4843750000000000000, 0.4921875000000000000, 0.5000000000000000000, 0.5078125000000000000, 0.5156250000000000000, 0.5234375000000000000, 0.5312500000000000000, 0.5390625000000000000, 0.5468750000000000000, 0.5546875000000000000, 0.5625000000000000000, 0.5703125000000000000, 0.5781250000000000000, 0.5859375000000000000, 0.5937500000000000000, 0.6015625000000000000, 0.6093750000000000000, 0.6171875000000000000, 0.6250000000000000000, 0.6328125000000000000, 0.6406250000000000000, 0.6484375000000000000, 0.6562500000000000000, 0.6640625000000000000, 0.6718750000000000000, 0.6796875000000000000, 0.6875000000000000000, 0.6953125000000000000, 0.7031250000000000000, 0.7109375000000000000, 0.7187500000000000000, 0.7265625000000000000, 0.7343750000000000000, 0.7421875000000000000, 0.7500000000000000000, 0.7578125000000000000, 0.7656250000000000000, 0.7734375000000000000, 0.7812500000000000000, 0.7890625000000000000, 0.7968750000000000000, 0.8046875000000000000, 0.8125000000000000000, 0.8203125000000000000, 0.8281250000000000000, 0.8359375000000000000, 0.8437500000000000000, 0.8515625000000000000, 0.8593750000000000000, 0.8671875000000000000, 0.8750000000000000000, 0.8828125000000000000, 0.8906250000000000000, 0.8984375000000000000, 0.9062500000000000000, 0.9140625000000000000, 0.9218750000000000000, 0.9296875000000000000, 0.9375000000000000000, 0.9453125000000000000, 0.9531250000000000000, 0.9609375000000000000, 0.9687500000000000000, 0.9765625000000000000, 0.9843750000000000000, 0.9921875000000000000, 1.000000000000000000 ),
 .UNSPECIFIED. ) 
 GEOMETRIC_REPRESENTATION_ITEM ( )  RATIONAL_B_SPLINE_SURFACE ( (
 ( 1.000000000000000000, 0.9238795325112869605, 1.000000000000000000, 0.9238795325112869605, 1.000000000000000000, 0.9238795325112869605, 1.000000000000000000, 0.9238795325112869605, 1.000000000000000000, 0.9238795325112869605, 1.000000000000000000, 0.9238795325112869605, 1.000000000000000000, 0.9238795325112869605, 1.000000000000000000, 0.9238795325112869605, 1.000000000000000000, 0.9238795325112869605, 1.000000000000000000, 0.9238795325112869605, 1.000000000000000000, 0.9238795325112869605, 1.000000000000000000, 0.9238795325112869605, 1.000000000000000000, 0.9238795325112869605, 1.000000000000000000, 0.9238795325112869605, 1.000000000000000000, 0.9238795325112869605, 1.000000000000000000, 0.9238795325112869605, 1.000000000000000000, 0.9238795325112869605, 1.000000000000000000, 0.9238795325112869605, 1.000000000000000000, 0.9238795325112869605, 1.000000000000000000, 0.9238795325112869605, 1.000000000000000000, 0.9238795325112869605, 1.000000000000000000, 0.9238795325112869605, 1.000000000000000000, 0.9238795325112869605, 1.000000000000000000, 0.9238795325112869605, 1.000000000000000000, 0.9238795325112869605, 1.000000000000000000, 0.9238795325112869605, 1.000000000000000000, 0.9238795325112869605, 1.000000000000000000, 0.9238795325112869605, 1.000000000000000000, 0.9238795325112869605, 1.000000000000000000, 0.9238795325112869605, 1.000000000000000000, 0.9238795325112869605, 1.000000000000000000, 0.9238795325112869605, 1.000000000000000000, 0.9238795325112869605, 1.000000000000000000, 0.9238795325112869605, 1.000000000000000000, 0.9238795325112869605, 1.000000000000000000, 0.9238795325112869605, 1.000000000000000000, 0.9238795325112869605, 1.000000000000000000, 0.9238795325112869605, 1.000000000000000000, 0.9238795325112869605, 1.000000000000000000, 0.9238795325112869605, 1.000000000000000000, 0.9238795325112869605, 1.000000000000000000, 0.9238795325112869605, 1.000000000000000000, 0.9238795325112869605, 1.000000000000000000, 0.9238795325112869605, 1.000000000000000000, 0.9238795325112869605, 1.000000000000000000, 0.9238795325112869605, 1.000000000000000000, 0.9238795325112869605, 1.000000000000000000, 0.9238795325112869605, 1.000000000000000000, 0.9238795325112869605, 1.000000000000000000, 0.9238795325112869605, 1.000000000000000000, 0.9238795325112869605, 1.000000000000000000, 0.9238795325112869605, 1.000000000000000000, 0.9238795325112869605, 1.000000000000000000, 0.9238795325112869605, 1.000000000000000000, 0.9238795325112869605, 1.000000000000000000, 0.9238795325112869605, 1.000000000000000000, 0.9238795325112869605, 1.000000000000000000, 0.9238795325112869605, 1.000000000000000000, 0.9238795325112869605, 1.000000000000000000, 0.9238795325112869605, 1.000000000000000000, 0.9238795325112869605, 1.000000000000000000, 0.9238795325112869605, 1.000000000000000000, 0.9238795325112869605, 1.000000000000000000, 0.9238795325112869605, 1.000000000000000000, 0.9238795325112869605, 1.000000000000000000, 0.9238795325112869605, 1.000000000000000000, 0.9238795325112869605, 1.000000000000000000, 0.9238795325112869605, 1.000000000000000000, 0.9238795325112869605, 1.000000000000000000, 0.9238795325112869605, 1.000000000000000000, 0.9238795325112869605, 1.000000000000000000, 0.9238795325112869605, 1.000000000000000000, 0.9238795325112869605, 1.000000000000000000, 0.9238795325112869605, 1.000000000000000000, 0.9238795325112869605, 1.000000000000000000, 0.9238795325112869605, 1.000000000000000000, 0.9238795325112869605, 1.000000000000000000, 0.9238795325112869605, 1.000000000000000000, 0.9238795325112869605, 1.000000000000000000, 0.9238795325112869605, 1.000000000000000000, 0.9238795325112869605, 1.000000000000000000, 0.9238795325112869605, 1.000000000000000000, 0.9238795325112869605, 1.000000000000000000, 0.9238795325112869605, 1.000000000000000000, 0.9238795325112869605, 1.000000000000000000, 0.9238795325112869605, 1.000000000000000000, 0.9238795325112869605, 1.000000000000000000, 0.9238795325112869605, 1.000000000000000000, 0.9238795325112869605, 1.000000000000000000, 0.9238795325112869605, 1.000000000000000000, 0.9238795325112869605, 1.000000000000000000, 0.9238795325112869605, 1.000000000000000000, 0.9238795325112869605, 1.000000000000000000, 0.9238795325112869605, 1.000000000000000000, 0.9238795325112869605, 1.000000000000000000, 0.9238795325112869605, 1.000000000000000000, 0.9238795325112869605, 1.000000000000000000, 0.9238795325112869605, 1.000000000000000000, 0.9238795325112869605, 1.000000000000000000, 0.9238795325112869605, 1.000000000000000000, 0.9238795325112869605, 1.000000000000000000, 0.9238795325112869605, 1.000000000000000000, 0.9238795325112869605, 1.000000000000000000, 0.9238795325112869605, 1.000000000000000000, 0.9238795325112869605, 1.000000000000000000, 0.9238795325112869605, 1.000000000000000000, 0.9238795325112869605, 1.000000000000000000, 0.9238795325112869605, 1.000000000000000000, 0.9238795325112869605, 1.000000000000000000, 0.9238795325112869605, 1.000000000000000000, 0.9238795325112869605, 1.000000000000000000, 0.9238795325112869605, 1.000000000000000000, 0.9238795325112869605, 1.000000000000000000, 0.9238795325112869605, 1.000000000000000000, 0.9238795325112869605, 1.000000000000000000, 0.9238795325112869605, 1.000000000000000000, 0.9238795325112869605, 1.000000000000000000, 0.9238795325112869605, 1.000000000000000000, 0.9238795325112869605, 1.000000000000000000, 0.9238795325112869605, 1.000000000000000000, 0.9238795325112869605, 1.000000000000000000, 0.9238795325112869605, 1.000000000000000000, 0.9238795325112869605, 1.000000000000000000, 0.9238795325112869605, 1.000000000000000000, 0.9238795325112869605, 1.000000000000000000, 0.9238795325112869605, 1.000000000000000000, 0.9238795325112869605, 1.000000000000000000, 0.9238795325112869605, 1.000000000000000000),
 ( 1.000000000000000000, 0.9238795325112869605, 1.000000000000000000, 0.9238795325112869605, 1.000000000000000000, 0.9238795325112869605, 1.000000000000000000, 0.9238795325112869605, 1.000000000000000000, 0.9238795325112869605, 1.000000000000000000, 0.9238795325112869605, 1.000000000000000000, 0.9238795325112869605, 1.000000000000000000, 0.9238795325112869605, 1.000000000000000000, 0.9238795325112869605, 1.000000000000000000, 0.9238795325112869605, 1.000000000000000000, 0.9238795325112869605, 1.000000000000000000, 0.9238795325112869605, 1.000000000000000000, 0.9238795325112869605, 1.000000000000000000, 0.9238795325112869605, 1.000000000000000000, 0.9238795325112869605, 1.000000000000000000, 0.9238795325112869605, 1.000000000000000000, 0.9238795325112869605, 1.000000000000000000, 0.9238795325112869605, 1.000000000000000000, 0.9238795325112869605, 1.000000000000000000, 0.9238795325112869605, 1.000000000000000000, 0.9238795325112869605, 1.000000000000000000, 0.9238795325112869605, 1.000000000000000000, 0.9238795325112869605, 1.000000000000000000, 0.9238795325112869605, 1.000000000000000000, 0.9238795325112869605, 1.000000000000000000, 0.9238795325112869605, 1.000000000000000000, 0.9238795325112869605, 1.000000000000000000, 0.9238795325112869605, 1.000000000000000000, 0.9238795325112869605, 1.000000000000000000, 0.9238795325112869605, 1.000000000000000000, 0.9238795325112869605, 1.000000000000000000, 0.9238795325112869605, 1.000000000000000000, 0.9238795325112869605, 1.000000000000000000, 0.9238795325112869605, 1.000000000000000000, 0.9238795325112869605, 1.000000000000000000, 0.9238795325112869605, 1.000000000000000000, 0.9238795325112869605, 1.000000000000000000, 0.9238795325112869605, 1.000000000000000000, 0.9238795325112869605, 1.000000000000000000, 0.9238795325112869605, 1.000000000000000000, 0.9238795325112869605, 1.000000000000000000, 0.9238795325112869605, 1.000000000000000000, 0.9238795325112869605, 1.000000000000000000, 0.9238795325112869605, 1.000000000000000000, 0.9238795325112869605, 1.000000000000000000, 0.9238795325112869605, 1.000000000000000000, 0.9238795325112869605, 1.000000000000000000, 0.9238795325112869605, 1.000000000000000000, 0.9238795325112869605, 1.000000000000000000, 0.9238795325112869605, 1.000000000000000000, 0.9238795325112869605, 1.000000000000000000, 0.9238795325112869605, 1.000000000000000000, 0.9238795325112869605, 1.000000000000000000, 0.9238795325112869605, 1.000000000000000000, 0.9238795325112869605, 1.000000000000000000, 0.9238795325112869605, 1.000000000000000000, 0.9238795325112869605, 1.000000000000000000, 0.9238795325112869605, 1.000000000000000000, 0.9238795325112869605, 1.000000000000000000, 0.9238795325112869605, 1.000000000000000000, 0.9238795325112869605, 1.000000000000000000, 0.9238795325112869605, 1.000000000000000000, 0.9238795325112869605, 1.000000000000000000, 0.9238795325112869605, 1.000000000000000000, 0.9238795325112869605, 1.000000000000000000, 0.9238795325112869605, 1.000000000000000000, 0.9238795325112869605, 1.000000000000000000, 0.9238795325112869605, 1.000000000000000000, 0.9238795325112869605, 1.000000000000000000, 0.9238795325112869605, 1.000000000000000000, 0.9238795325112869605, 1.000000000000000000, 0.9238795325112869605, 1.000000000000000000, 0.9238795325112869605, 1.000000000000000000, 0.9238795325112869605, 1.000000000000000000, 0.9238795325112869605, 1.000000000000000000, 0.9238795325112869605, 1.000000000000000000, 0.9238795325112869605, 1.000000000000000000, 0.9238795325112869605, 1.000000000000000000, 0.9238795325112869605, 1.000000000000000000, 0.9238795325112869605, 1.000000000000000000, 0.9238795325112869605, 1.000000000000000000, 0.9238795325112869605, 1.000000000000000000, 0.9238795325112869605, 1.000000000000000000, 0.9238795325112869605, 1.000000000000000000, 0.9238795325112869605, 1.000000000000000000, 0.9238795325112869605, 1.000000000000000000, 0.9238795325112869605, 1.000000000000000000, 0.9238795325112869605, 1.000000000000000000, 0.9238795325112869605, 1.000000000000000000, 0.9238795325112869605, 1.000000000000000000, 0.9238795325112869605, 1.000000000000000000, 0.9238795325112869605, 1.000000000000000000, 0.9238795325112869605, 1.000000000000000000, 0.9238795325112869605, 1.000000000000000000, 0.9238795325112869605, 1.000000000000000000, 0.9238795325112869605, 1.000000000000000000, 0.9238795325112869605, 1.000000000000000000, 0.9238795325112869605, 1.000000000000000000, 0.9238795325112869605, 1.000000000000000000, 0.9238795325112869605, 1.000000000000000000, 0.9238795325112869605, 1.000000000000000000, 0.9238795325112869605, 1.000000000000000000, 0.9238795325112869605, 1.000000000000000000, 0.9238795325112869605, 1.000000000000000000, 0.9238795325112869605, 1.000000000000000000, 0.9238795325112869605, 1.000000000000000000, 0.9238795325112869605, 1.000000000000000000, 0.9238795325112869605, 1.000000000000000000, 0.9238795325112869605, 1.000000000000000000, 0.9238795325112869605, 1.000000000000000000, 0.9238795325112869605, 1.000000000000000000, 0.9238795325112869605, 1.000000000000000000, 0.9238795325112869605, 1.000000000000000000, 0.9238795325112869605, 1.000000000000000000, 0.9238795325112869605, 1.000000000000000000, 0.9238795325112869605, 1.000000000000000000, 0.9238795325112869605, 1.000000000000000000, 0.9238795325112869605, 1.000000000000000000, 0.9238795325112869605, 1.000000000000000000, 0.9238795325112869605, 1.000000000000000000, 0.9238795325112869605, 1.000000000000000000, 0.9238795325112869605, 1.000000000000000000, 0.9238795325112869605, 1.000000000000000000, 0.9238795325112869605, 1.000000000000000000, 0.9238795325112869605, 1.000000000000000000, 0.9238795325112869605, 1.000000000000000000, 0.9238795325112869605, 1.000000000000000000, 0.9238795325112869605, 1.000000000000000000) ) ) 
 REPRESENTATION_ITEM ( '' )  SURFACE ( )  );
#12997 = CARTESIAN_POINT ( 'NONE',  ( 115.3489614775786407, -0.8288870151387760510, -10.36305467784173118 ) ) ;
#12998 = CARTESIAN_POINT ( 'NONE',  ( 137.2618751060971647, -3.292307989136469271, -8.378698585220082151 ) ) ;
#12999 = CARTESIAN_POINT ( 'NONE',  ( 119.6034614775786196, -3.505236298600246325, -18.68346056562440793 ) ) ;
#13000 = CARTESIAN_POINT ( 'NONE',  ( 121.9470836909669913, -27.84333996136784961, -14.15691383771150136 ) ) ;
#13001 = CARTESIAN_POINT ( 'NONE',  ( 116.6536748109119941, -10.15424416112533912, -14.75197769757731336 ) ) ;
#13002 = CARTESIAN_POINT ( 'NONE',  ( 115.5758681442453053, -1.561330072975668060, -17.79121239304076951 ) ) ;
#13003 = CARTESIAN_POINT ( 'NONE',  ( 124.0495485609119584, -0.08252387247370887580, -11.91645802438286417 ) ) ;
#13004 = CARTESIAN_POINT ( 'NONE',  ( 111.7184548109119788, -9.261995988541697145, -16.69588392320189030 ) ) ;
#13005 = CARTESIAN_POINT ( 'NONE',  ( 116.5969481442453031, -9.859900752359374465, -12.68260735090039404 ) ) ;
#13006 = CARTESIAN_POINT ( 'NONE',  ( 123.8579614775786126, 0.5811942927096110934, -14.16772938898807510 ) ) ;
#13007 = CARTESIAN_POINT ( 'NONE',  ( 123.2906948109119867, -8.166667518702819706, -8.995218007635861213 ) ) ;
#13008 = ORIENTED_EDGE ( 'NONE', *, *, #4404, .F. ) ;
#13009 = CARTESIAN_POINT ( 'NONE',  ( 114.6682414775786469, -1.561330072975668060, -17.79121239304076596 ) ) ;
#13010 = CARTESIAN_POINT ( 'NONE',  ( 111.8716296295247901, -4.863998795839590272, -19.15521520033831493 ) ) ;
#13011 = CARTESIAN_POINT ( 'NONE',  ( 71.02242295334774269, -59.69535702388913023, -40.18575152407060358 ) ) ;
#13012 = DIRECTION ( 'NONE',  ( 0.5735764363510499342, 0.3127926500124801890, -0.7570804645221008711 ) ) ;
#13013 = CARTESIAN_POINT ( 'NONE',  ( 128.0388906786927805, -4.056017420846984578, -15.71820436844875424 ) ) ;
#13014 = CARTESIAN_POINT ( 'NONE',  ( 117.0507614775786465, -10.30919188438810075, -12.61870101168855918 ) ) ;
#13015 = EDGE_LOOP ( 'NONE', ( #25591, #24673, #30668, #9094, #21520, #36920 ) ) ;
#13016 = LINE ( 'NONE', #34191, #10007 ) ;
#13017 = DIRECTION ( 'NONE',  ( 1.000000000000000000, 0.000000000000000000, 0.000000000000000000 ) ) ;
#13018 = CARTESIAN_POINT ( 'NONE',  ( 113.1366214775786432, -7.643976991954077427, -18.09477374809248928 ) ) ;
#13019 = EDGE_CURVE ( 'NONE', #15443, #17364, #44928, .T. ) ;
#13020 = DIRECTION ( 'NONE',  ( 1.000000000000000000, 0.000000000000000000, 0.000000000000000000 ) ) ;
#13021 = CARTESIAN_POINT ( 'NONE',  ( 122.9503348109119827, 0.5811942927096110934, -14.16772938898807510 ) ) ;
#13022 = CARTESIAN_POINT ( 'NONE',  ( 115.0664733795247798, -1.325403438956436419, -9.854619843455211026 ) ) ;
#13023 = CARTESIAN_POINT ( 'NONE',  ( 72.54180985774836188, -59.72843766223603268, -36.36500299946500547 ) ) ;
#13024 = EDGE_LOOP ( 'NONE', ( #1427, #36504, #26738, #7863, #75 ) ) ;
#13025 = LINE ( 'NONE', #16445, #36167 ) ;
#13026 = CARTESIAN_POINT ( 'NONE',  ( 121.5888948109119809, 0.1319031606808879209, -14.10382304977623669 ) ) ;
#13027 = CARTESIAN_POINT ( 'NONE',  ( 120.0005481442453146, -5.638512984488999180, -18.83840828888717311 ) ) ;
#13028 = CARTESIAN_POINT ( 'NONE',  ( 115.1220548109119761, -1.833838273342658809, -17.42832698103878286 ) ) ;
#13029 = CARTESIAN_POINT ( 'NONE',  ( 115.1220548109119761, -8.166667518702817929, -8.995218007635861213 ) ) ;
#13030 = CARTESIAN_POINT ( 'NONE',  ( 89.01247232317646763, -24.14644159042263993, -12.62951656296512937 ) ) ;
#13031 = CARTESIAN_POINT ( 'NONE',  ( 78.69189222814998175, -46.76310523276723785, -23.89321520033831803 ) ) ;
#13032 = CARTESIAN_POINT ( 'NONE',  ( 118.6958348109119754, -3.505236298600246325, -18.68346056562440793 ) ) ;
#13033 = ORIENTED_EDGE ( 'NONE', *, *, #36601, .T. ) ;
#13034 = CARTESIAN_POINT ( 'NONE',  ( 124.1884548109119777, -7.554583864224885481, -18.48844787311982785 ) ) ;
#13035 = CARTESIAN_POINT ( 'NONE',  ( 111.8319081442453182, -5.638512984488999180, -18.83840828888717311 ) ) ;
#13036 = CARTESIAN_POINT ( 'NONE',  ( 120.6812681442452941, 0.1319031606808879209, -14.10382304977623669 ) ) ;
#13037 = EDGE_LOOP ( 'NONE', ( #42852, #912, #42498, #27704, #25597 ) ) ;
#13038 = CARTESIAN_POINT ( 'NONE',  ( 121.6881423109119709, -0.4387604401700512802, -15.73000352943951619 ) ) ;
#13039 = CARTESIAN_POINT ( 'NONE',  ( 119.6034614775786196, -6.344957434206665248, -7.627207830600338134 ) ) ;
#13040 = CARTESIAN_POINT ( 'NONE',  ( 114.2330358795247776, -0.7896495226426338832, -17.46756447353520159 ) ) ;
#13041 = CARTESIAN_POINT ( 'NONE',  ( 117.1642148109119859, -0.8288870151387760510, -10.36305467784173118 ) ) ;
#13042 = EDGE_CURVE ( 'NONE', #24400, #38783, #16822, .T. ) ;
#13043 = VERTEX_POINT ( 'NONE', #28709 ) ;
#13044 = ORIENTED_EDGE ( 'NONE', *, *, #14764, .F. ) ;
#13045 = CARTESIAN_POINT ( 'NONE',  ( 124.0848681442452772, -5.574606645277164318, -18.38911715685844683 ) ) ;
#13046 = CARTESIAN_POINT ( 'NONE',  ( 120.5110881442453206, -3.505236298600246325, -18.68346056562440793 ) ) ;
#13047 = CARTESIAN_POINT ( 'NONE',  ( -7.917624645353497748, -12.21642755857638818, -19.39321520033831447 ) ) ;
#13048 = EDGE_CURVE ( 'NONE', #30068, #14242, #24846, .T. ) ;
#13049 = DIRECTION ( 'NONE',  ( 0.000000000000000000, -0.3818493186865927203, 0.9242245927363029745 ) ) ;
#13050 = EDGE_CURVE ( 'NONE', #45054, #7584, #18448, .T. ) ;
#13051 = CARTESIAN_POINT ( 'NONE',  ( 116.8238548109119819, -4.089484607189486809, -7.948022111789456723 ) ) ;
#13052 = CARTESIAN_POINT ( 'NONE',  ( 108.6073327545248048, -2.477300249445798297, -19.15521520033831138 ) ) ;
#13053 = CARTESIAN_POINT ( 'NONE',  ( 119.8870948109119752, -9.261995988541697145, -16.69588392320189030 ) ) ;
#13055 = CARTESIAN_POINT ( 'NONE',  ( 119.3765548109119834, -10.15424416112533912, -14.75197769757731336 ) ) ;
#13054 = CARTESIAN_POINT ( 'NONE',  ( 120.2841814775786276, 0.9020085738987339008, -11.91225656197089222 ) ) ;
#13056 = CARTESIAN_POINT ( 'NONE',  ( 125.6164881442453094, -9.565557343593413364, -10.61323700422348004 ) ) ;
#13057 = CARTESIAN_POINT ( 'NONE',  ( 111.9453614775786434, -1.561330072975668060, -17.79121239304076596 ) ) ;
#13058 = ORIENTED_EDGE ( 'NONE', *, *, #8377, .F. ) ;
#13059 = CARTESIAN_POINT ( 'NONE',  ( 122.7234281442452755, -4.153390946401325223, -8.397313243818185668 ) ) ;
#13060 = CARTESIAN_POINT ( 'NONE',  ( 78.69189222814998175, -49.76310523276723785, -13.39321520033831447 ) ) ;
#13061 = EDGE_CURVE ( 'NONE', #19163, #4387, #17559, .T. ) ;
#13062 = CARTESIAN_POINT ( 'NONE',  ( 125.4584548109119737, -4.863998795839242995, -13.39321520033831447 ) ) ;
#13063 = CARTESIAN_POINT ( 'NONE',  ( 108.6767858795247861, -0.7896495226426338832, -17.46756447353520159 ) ) ;
#13064 = CARTESIAN_POINT ( 'NONE',  ( 115.5526452545247622, -9.868328341294098749, -15.46607636864997204 ) ) ;
#13065 = CARTESIAN_POINT ( 'NONE',  ( 107.4266296295248821, -4.863998795839590272, -19.15521520033831493 ) ) ;
#13066 = CARTESIAN_POINT ( 'NONE',  ( 123.4608748109119745, -10.63000616557722466, -14.87417383870573495 ) ) ;
#13067 = CARTESIAN_POINT ( 'NONE',  ( 121.5888948109119809, 0.1319031606808879209, -14.10382304977623669 ) ) ;
#13068 = ORIENTED_EDGE ( 'NONE', *, *, #21309, .T. ) ;
#13069 = EDGE_CURVE ( 'NONE', #29689, #7697, #10927, .T. ) ;
#13070 = CARTESIAN_POINT ( 'NONE',  ( 125.4463081442452932, -5.638512984488999180, -18.83840828888717311 ) ) ;
#13071 = CARTESIAN_POINT ( 'NONE',  ( 113.9875214775786532, -8.899110576539710493, -16.42337572283490132 ) ) ;
#13072 = CARTESIAN_POINT ( 'NONE',  ( 65.31031011413875831, -19.24203766017952333, -5.548074201837920327 ) ) ;
#13073 = CARTESIAN_POINT ( 'NONE',  ( 120.0005481442453146, -5.638512984488999180, -18.83840828888717311 ) ) ;
#13074 = EDGE_CURVE ( 'NONE', #6181, #35601, #5111, .T. ) ;
#13075 = EDGE_CURVE ( 'NONE', #4322, #26462, #29923, .T. ) ;
#13076 = CARTESIAN_POINT ( 'NONE',  ( 120.4543614775786295, -4.089484607189486809, -7.948022111789456723 ) ) ;
#13077 = CARTESIAN_POINT ( 'NONE',  ( 123.4366330209070099, -6.157706758239399392, -18.56290235964623392 ) ) ;
#13078 = CARTESIAN_POINT ( 'NONE',  ( 124.8790414775786246, -8.899110576539710493, -16.42337572283490132 ) ) ;
#13079 = CARTESIAN_POINT ( 'NONE',  ( 115.6893214775786447, 0.5811942927096102052, -14.16772938898808221 ) ) ;
#13080 = DIRECTION ( 'NONE',  ( 0.000000000000000000, 0.000000000000000000, 1.000000000000000000 ) ) ;
#13081 = VERTEX_POINT ( 'NONE', #3842 ) ;
#13082 = LINE ( 'NONE', #3481, #33952 ) ;
#13083 = CARTESIAN_POINT ( 'NONE',  ( 118.3912731944929391, -1.036737761566197014, -17.24079555149560861 ) ) ;
#13084 = CARTESIAN_POINT ( 'NONE',  ( 124.1415948109119540, -3.505236298600246325, -18.68346056562440793 ) ) ;
#13085 = CIRCLE ( 'NONE', #38528, 0.8509999999999994236 ) ;
#13086 = CARTESIAN_POINT ( 'NONE',  ( 109.5102233795247884, -1.325403438956436419, -9.854619843455211026 ) ) ;
#13087 = CARTESIAN_POINT ( 'NONE',  ( 113.3995983795247895, -8.402594152722688392, -16.93181055722141792 ) ) ;
#13089 = AXIS2_PLACEMENT_3D ( 'NONE', #33331, #2105, #4633 ) ;
#13088 = CARTESIAN_POINT ( 'NONE',  ( 118.9794681442453026, -0.8288870151387760510, -10.36305467784173118 ) ) ;
#13090 = CARTESIAN_POINT ( 'NONE',  ( 116.9373081442452929, -1.833838273342659253, -17.42832698103878286 ) ) ;
#13091 = CARTESIAN_POINT ( 'NONE',  ( 123.6877814775786533, -3.383040157471821630, -19.15922257007629170 ) ) ;
#13092 = EDGE_LOOP ( 'NONE', ( #23292, #14800, #16661, #26716, #5398, #33309 ) ) ;
#13093 = CARTESIAN_POINT ( 'NONE',  ( 122.9503348109119827, -9.859900752359378018, -12.68260735090039759 ) ) ;
#13094 = CARTESIAN_POINT ( 'NONE',  ( 119.1496481442453046, -3.383040157471821630, -19.15922257007629170 ) ) ;
#13095 = CARTESIAN_POINT ( 'NONE',  ( 124.4252281442452812, -9.261995988541697145, -16.69588392320189030 ) ) ;
#13096 = CARTESIAN_POINT ( 'NONE',  ( 124.5954081442453116, -6.222761293078241884, -8.102969835052219238 ) ) ;
#13097 = ORIENTED_EDGE ( 'NONE', *, *, #21801, .F. ) ;
#13098 = CARTESIAN_POINT ( 'NONE',  ( 69.48815586033239811, -68.74046964786722924, -38.06815038123374251 ) ) ;
#13099 = CARTESIAN_POINT ( 'NONE',  ( 125.4463081442452932, -5.638512984488999180, -18.83840828888717311 ) ) ;
#13100 = CARTESIAN_POINT ( 'NONE',  ( 114.6682414775786469, -7.894159318335828068, -9.358103419637847864 ) ) ;
#13101 = CARTESIAN_POINT ( 'NONE',  ( 123.4041481442452834, -10.30919188438810075, -12.61870101168855918 ) ) ;
#13102 = CARTESIAN_POINT ( 'NONE',  ( 106.5931921295248372, 0.8980012041604618078, -13.39321520033831447 ) ) ;
#13103 = CARTESIAN_POINT ( 'NONE',  ( 123.1466579359119891, -4.360204210389833968, -8.000047426360245240 ) ) ;
#13104 = ORIENTED_EDGE ( 'NONE', *, *, #5695, .T. ) ;
#13105 = CARTESIAN_POINT ( 'NONE',  ( 94.20708369096698220, -25.99489077589524300, -13.39321520033831447 ) ) ;
#13106 = CARTESIAN_POINT ( 'NONE',  ( 111.1770983795247787, -8.402594152722688392, -16.93181055722141792 ) ) ;
#13107 = VECTOR ( 'NONE', #19971, 1000.000000000000000 ) ;
#13108 = DIRECTION ( 'NONE',  ( 0.9609149988134837450, -0.1028163501681639419, 0.2570431154366518145 ) ) ;
#13109 = CARTESIAN_POINT ( 'NONE',  ( 119.3765548109119834, -10.15424416112533912, -14.75197769757731336 ) ) ;
#13110 = CARTESIAN_POINT ( 'NONE',  ( 114.3278814775786429, 0.1319031606808879209, -14.10382304977623669 ) ) ;
#13111 = CARTESIAN_POINT ( 'NONE',  ( 126.4599182912884743, -0.4449873272706824645, -10.80585118086940533 ) ) ;
#13112 = ORIENTED_EDGE ( 'NONE', *, *, #39257, .T. ) ;
#13113 = CARTESIAN_POINT ( 'NONE',  ( 70.19189222814998175, -60.97346038181336070, -37.59218076343751136 ) ) ;
#13114 = CARTESIAN_POINT ( 'NONE',  ( 121.3052614775786111, -7.643976991954077427, -18.09477374809248928 ) ) ;
#13115 = LINE ( 'NONE', #27474, #42064 ) ;
#13116 = AXIS2_PLACEMENT_3D ( 'NONE', #8845, #40541, #9302 ) ;
#13117 = CARTESIAN_POINT ( 'NONE',  ( 68.08062758086367694, -0.7900929402678026348, -10.39321520033831625 ) ) ;
#13118 = CARTESIAN_POINT ( 'NONE',  ( 111.6722681442453222, -0.8658195297461032114, -10.39078908864415496 ) ) ;
#13120 = CARTESIAN_POINT ( 'NONE',  ( 123.9146881442452894, 0.9020085738987339008, -11.91225656197089222 ) ) ;
#13119 = CARTESIAN_POINT ( 'NONE',  ( 73.07463722459043254, -54.78256478388924933, -34.22133621331339981 ) ) ;
#13121 = CARTESIAN_POINT ( 'NONE',  ( 113.1366214775786432, -1.834011780172310813, -8.268836392978581529 ) ) ;
#13122 = EDGE_LOOP ( 'NONE', ( #28798, #33500, #9437, #1937, #18351 ) ) ;
#13123 = VECTOR ( 'NONE', #15219, 1000.000000000000000 ) ;
#13124 = CARTESIAN_POINT ( 'NONE',  ( 114.1577014775786552, -6.344957434206662583, -7.627207830600332805 ) ) ;
#13125 = CARTESIAN_POINT ( 'NONE',  ( 113.7798197424434363, -0.9924539043446216624, -17.29976612834909133 ) ) ;
#13126 = CARTESIAN_POINT ( 'NONE',  ( 114.5108483795247878, -0.7896495226426338832, -9.318865927141430916 ) ) ;
#13127 = ADVANCED_FACE ( 'NONE', ( #427 ), #30680, .T. ) ;
#13128 = CARTESIAN_POINT ( 'NONE',  ( 124.7088614775786226, -9.565557343593413364, -10.61323700422348004 ) ) ;
#13129 = CARTESIAN_POINT ( 'NONE',  ( 121.0783548109119749, -9.565557343593413364, -10.61323700422348004 ) ) ;
#13130 = DIRECTION ( 'NONE',  ( 0.000000000000000000, 0.000000000000000000, -1.000000000000000000 ) ) ;
#13131 = CARTESIAN_POINT ( 'NONE',  ( 105.4819421295248247, 0.8980012041604618078, -13.39321520033831447 ) ) ;
#13132 = CYLINDRICAL_SURFACE ( 'NONE', #9170, 3.000000000000001776 ) ;
#13133 = CARTESIAN_POINT ( 'NONE',  ( 63.10250807381770244, -31.76310523276723430, -22.89321520033831803 ) ) ;
#13134 = CARTESIAN_POINT ( 'NONE',  ( 113.0798948109119948, -8.899110576539710493, -16.42337572283490132 ) ) ;
#13135 = CARTESIAN_POINT ( 'NONE',  ( 108.9545983795247821, -0.7896495226426338832, -9.318865927141430916 ) ) ;
#13136 = CARTESIAN_POINT ( 'NONE',  ( 111.7184548109119788, -9.261995988541697145, -16.69588392320189030 ) ) ;
#13137 = CARTESIAN_POINT ( 'NONE',  ( 113.1912390045248031, 0.8980012041604421569, -15.77991374673208469 ) ) ;
#13138 = CARTESIAN_POINT ( 'NONE',  ( 123.1205148109119563, -1.834011780172310813, -8.268836392978581529 ) ) ;
#13139 = CARTESIAN_POINT ( 'NONE',  ( 120.5678148109119832, -8.166667518702819706, -8.995218007635861213 ) ) ;
#13140 = PLANE ( 'NONE',  #21173 ) ;
#13141 = EDGE_CURVE ( 'NONE', #21889, #26433, #31659, .T. ) ;
#13142 = CARTESIAN_POINT ( 'NONE',  ( 122.0427081442452817, 0.5811942927096110934, -14.16772938898807510 ) ) ;
#13143 = CARTESIAN_POINT ( 'NONE',  ( 113.0231681442453322, 0.9020085738987339008, -11.91225656197089222 ) ) ;
#13144 = ORIENTED_EDGE ( 'NONE', *, *, #12499, .F. ) ;
#13145 = CARTESIAN_POINT ( 'NONE',  ( 113.0231681442453180, -10.15424416112533912, -14.75197769757731336 ) ) ;
#13146 = CARTESIAN_POINT ( 'NONE',  ( 125.5597614775786326, -1.561330072975669392, -17.79121239304076951 ) ) ;
#13147 = CARTESIAN_POINT ( 'NONE',  ( 125.1626748109119802, -9.988377603198980381, -10.36322818467138518 ) ) ;
#13148 = VECTOR ( 'NONE', #10324, 1000.000000000000000 ) ;
#13149 = CARTESIAN_POINT ( 'NONE',  ( 115.8027748109119841, -0.4660016031367893996, -10.09054647747474043 ) ) ;
#13150 = CARTESIAN_POINT ( 'NONE',  ( 112.0020881442453344, -9.565557343593413364, -10.61323700422348004 ) ) ;
#13151 = VERTEX_POINT ( 'NONE', #204 ) ;
#13152 = CARTESIAN_POINT ( 'NONE',  ( 117.2209414775786485, -2.084020599724406786, -8.691656652584148546 ) ) ;
#13153 = CARTESIAN_POINT ( 'NONE',  ( 112.9097148109120070, 0.2603800115204892296, -16.42320221600525088 ) ) ;
#13154 = VECTOR ( 'NONE', #18167, 1000.000000000000000 ) ;
#13155 = CARTESIAN_POINT ( 'NONE',  ( 109.0935046295247872, -4.863998795839590272, -18.39754474579285315 ) ) ;
#13156 = CARTESIAN_POINT ( 'NONE',  ( 121.9859814775786333, -9.565557343593413364, -10.61323700422348004 ) ) ;
#13157 = FACE_OUTER_BOUND ( 'NONE', #31083, .T. ) ;
#13158 = CARTESIAN_POINT ( 'NONE',  ( 112.0799890045248475, 0.8980012041604421569, -15.77991374673208469 ) ) ;
#13159 = ORIENTED_EDGE ( 'NONE', *, *, #18470, .F. ) ;
#13160 = VECTOR ( 'NONE', #31811, 1000.000000000000114 ) ;
#13161 = CARTESIAN_POINT ( 'NONE',  ( 114.5308753496756680, -1.087735405160637603, -17.17288456429614030 ) ) ;
#13162 = DIRECTION ( 'NONE',  ( 0.9609149988134843001, -0.1028163501681632064, 0.2570431154366505933 ) ) ;
#13163 = CARTESIAN_POINT ( 'NONE',  ( 113.1217858795247935, -8.402594152722736354, -9.854619843455244776 ) ) ;
#13164 = CARTESIAN_POINT ( 'NONE',  ( 112.6828081442453282, -7.893985811506177619, -18.51759400769804742 ) ) ;
#13165 = CARTESIAN_POINT ( 'NONE',  ( 116.5169474460644494, 2.197673667592547453, -6.272794238025070079 ) ) ;
#13166 = CARTESIAN_POINT ( 'NONE',  ( -13.78505786849281911, -3.796669023460696124, -19.39321520033831447 ) ) ;
#13167 = CARTESIAN_POINT ( 'NONE',  ( 107.7738952545248310, -9.868328341294098749, -15.46607636864997204 ) ) ;
#13168 = ADVANCED_FACE ( 'NONE', ( #42389 ), #28465, .T. ) ;
#13169 = DIRECTION ( 'NONE',  ( -1.000000000000000000, 0.000000000000000000, 0.000000000000000000 ) ) ;
#13170 = CARTESIAN_POINT ( 'NONE',  ( 119.0929214775786278, -5.638512984488999180, -18.83840828888717311 ) ) ;
#13171 = CARTESIAN_POINT ( 'NONE',  ( 137.4565547821518976, -5.984952545581320393, -18.32735042449561291 ) ) ;
#13172 = VECTOR ( 'NONE', #27101, 1000.000000000000227 ) ;
#13173 = DIRECTION ( 'NONE',  ( -1.000000000000000000, 0.000000000000000000, -0.000000000000000000 ) ) ;
#13174 = CARTESIAN_POINT ( 'NONE',  ( 123.8411891859119862, -1.406689858478695543, -17.56299727309111347 ) ) ;
#13175 = CARTESIAN_POINT ( 'NONE',  ( 119.6601881442453106, -1.833838273342659253, -17.42832698103878286 ) ) ;
#13176 = CARTESIAN_POINT ( 'NONE',  ( 125.6164881442453094, -9.565557343593413364, -10.61323700422348004 ) ) ;
#13177 = ORIENTED_EDGE ( 'NONE', *, *, #27960, .F. ) ;
#13178 = CARTESIAN_POINT ( 'NONE',  ( 121.3052614775786111, -1.834011780172310813, -8.268836392978581529 ) ) ;
#13179 = CARTESIAN_POINT ( 'NONE',  ( 120.2274548109119934, 0.5811942927096110934, -14.16772938898807510 ) ) ;
#13180 = CARTESIAN_POINT ( 'NONE',  ( 126.1837548109119211, -10.63000616557722466, -14.87417383870573495 ) ) ;
#13181 = CARTESIAN_POINT ( 'NONE',  ( 112.4559014775786778, -0.1624402480850797581, -16.17319339645315424 ) ) ;
#13182 = CARTESIAN_POINT ( 'NONE',  ( 125.3895814775786448, -7.893985811506177619, -18.51759400769804742 ) ) ;
#13183 = CARTESIAN_POINT ( 'NONE',  ( 110.4131140045248287, -10.62599879583958717, -11.00651665394454604 ) ) ;
#13184 = CARTESIAN_POINT ( 'NONE',  ( 105.3430358795248338, -8.402594152722688392, -9.854619843455216355 ) ) ;
#13185 = CARTESIAN_POINT ( 'NONE',  ( 116.5944421295247793, 0.8980012041604618078, -13.39321520033831447 ) ) ;
#13186 = CARTESIAN_POINT ( 'NONE',  ( 117.6747548109119919, -7.643976991954077427, -18.09477374809248928 ) ) ;
#13187 = VECTOR ( 'NONE', #37511, 1000.000000000000000 ) ;
#13188 = CARTESIAN_POINT ( 'NONE',  ( 117.3911214775786505, -7.894159318335828068, -9.358103419637847864 ) ) ;
#13189 = EDGE_CURVE ( 'NONE', #39449, #18952, #39395, .T. ) ;
#13190 = CARTESIAN_POINT ( 'NONE',  ( 113.2103884760652761, 0.6362173239733635022, -12.14321520033831625 ) ) ;
#13191 = CARTESIAN_POINT ( 'NONE',  ( 113.3301452545248083, -9.868328341294098749, -15.46607636864997204 ) ) ;
#13192 = ORIENTED_EDGE ( 'NONE', *, *, #38276, .T. ) ;
#13193 = AXIS2_PLACEMENT_3D ( 'NONE', #10216, #12566, #24124 ) ;
#13194 = FACE_OUTER_BOUND ( 'NONE', #42927, .T. ) ;
#13195 = CARTESIAN_POINT ( 'NONE',  ( 115.2355081442453155, -10.30919188438810075, -12.61870101168855918 ) ) ;
#13196 = DIRECTION ( 'NONE',  ( 1.000000000000000000, 0.000000000000000000, -0.000000000000000000 ) ) ;
#13197 = CARTESIAN_POINT ( 'NONE',  ( 121.6881423109119709, -0.4387604401700512802, -15.73000352943951619 ) ) ;
#13198 = CARTESIAN_POINT ( 'NONE',  ( 122.5910329359119970, -5.367793381288652910, -18.78638297431638904 ) ) ;
#13199 = VERTEX_POINT ( 'NONE', #34838 ) ;
#13200 = CARTESIAN_POINT ( 'NONE',  ( 114.3339130180080616, 0.7607806665038616689, -14.64321520033833757 ) ) ;
#13201 = CARTESIAN_POINT ( 'NONE',  ( 111.4812862606558923, -1.286823604262816279, -16.90776886114078437 ) ) ;
#13202 = ORIENTED_EDGE ( 'NONE', *, *, #15130, .F. ) ;
#13203 = CARTESIAN_POINT ( 'NONE',  ( 117.6747548109119919, -1.834011780172310813, -8.268836392978581529 ) ) ;
#13204 = CARTESIAN_POINT ( 'NONE',  ( 112.9664414775786412, 0.5811942927096154232, -14.16772938898807155 ) ) ;
#13205 = CARTESIAN_POINT ( 'NONE',  ( 119.9438214775786378, -2.084020599724406786, -8.691656652584148546 ) ) ;
#13206 = B_SPLINE_CURVE_WITH_KNOTS ( 'NONE', 3,
 ( #35633, #25170, #21968, #39526 ),
 .UNSPECIFIED., .F., .F.,
 ( 4, 4 ),
 ( 0.003793286375430135211, 0.004704238447046320444 ),
 .UNSPECIFIED. ) ;
#13207 =( NAMED_UNIT ( * ) SI_UNIT ( $, .STERADIAN. ) SOLID_ANGLE_UNIT ( ) );
#13208 = LINE ( 'NONE', #23697, #27911 ) ;
#13209 = CARTESIAN_POINT ( 'NONE',  ( 123.1772414775786189, -4.089484607189486809, -7.948022111789456723 ) ) ;
#13210 = CARTESIAN_POINT ( 'NONE',  ( 119.4900081442453086, -1.834011780172310813, -8.268836392978581529 ) ) ;
#13211 = CARTESIAN_POINT ( 'NONE',  ( 111.2465515045248168, -6.936859964151250502, -18.39754474579286025 ) ) ;
#13212 = CARTESIAN_POINT ( 'NONE',  ( 113.9875214775786532, -8.899110576539710493, -16.42337572283490132 ) ) ;
#13213 = DIRECTION ( 'NONE',  ( -0.5735764363510450492, -0.3127926500124816878, 0.7570804645221038687 ) ) ;
#13214 = ORIENTED_EDGE ( 'NONE', *, *, #22126, .T. ) ;
#13215 = CARTESIAN_POINT ( 'NONE',  ( 118.7525614775786380, -8.166667518702819706, -8.995218007635861213 ) ) ;
#13216 = CARTESIAN_POINT ( 'NONE',  ( 126.4536383592362370, -5.007014633634890188, -18.50900364442074064 ) ) ;
#13217 = CARTESIAN_POINT ( 'NONE',  ( 115.4624148109119943, -5.638512984488999180, -18.83840828888717311 ) ) ;
#13218 = ORIENTED_EDGE ( 'NONE', *, *, #7588, .F. ) ;
#13219 = CARTESIAN_POINT ( 'NONE',  ( 122.2128881442453263, -1.834011780172310813, -8.268836392978581529 ) ) ;
#13220 = CARTESIAN_POINT ( 'NONE',  ( 87.80477198183443477, -25.99489077589524300, -13.39321520033831625 ) ) ;
#13221 = CARTESIAN_POINT ( 'NONE',  ( 113.7606148109119886, -7.894159318335828068, -9.358103419637847864 ) ) ;
#13222 = DIRECTION ( 'NONE',  ( 0.000000000000000000, -0.4669533266896289669, -0.8842819633428519177 ) ) ;
#13223 = CARTESIAN_POINT ( 'NONE',  ( 117.8449348109119938, -1.833838273342659253, -17.42832698103878286 ) ) ;
#13224 = CARTESIAN_POINT ( 'NONE',  ( 123.3190498203445031, -3.658217111620186035, -16.24788372853176099 ) ) ;
#13225 = CARTESIAN_POINT ( 'NONE',  ( 117.1074881442453233, 0.4262465694468514643, -12.03445270309931736 ) ) ;
#13226 = FACE_OUTER_BOUND ( 'NONE', #39481, .T. ) ;
#13227 = CARTESIAN_POINT ( 'NONE',  ( 114.8951481442453115, -8.899110576539710493, -16.42337572283490132 ) ) ;
#13228 = CARTESIAN_POINT ( 'NONE',  ( 114.6115148109119986, -3.383040157471821630, -19.15922257007629170 ) ) ;
#13229 = CARTESIAN_POINT ( 'NONE',  ( 121.2019704359119743, -10.25716656981731489, -12.88942061488890545 ) ) ;
#13230 = CARTESIAN_POINT ( 'NONE',  ( 113.3068014775786594, -8.166667518702817929, -8.995218007635859436 ) ) ;
#13231 = CARTESIAN_POINT ( 'NONE',  ( 115.5758681442453053, -7.894159318335828068, -9.358103419637847864 ) ) ;
#13232 = CARTESIAN_POINT ( 'NONE',  ( 123.4608748109119745, -10.63000616557722466, -14.87417383870573495 ) ) ;
#13233 = CARTESIAN_POINT ( 'NONE',  ( 118.2987481442453088, -7.894159318335828068, -9.358103419637847864 ) ) ;
#13234 = ORIENTED_EDGE ( 'NONE', *, *, #34763, .T. ) ;
#13235 = CARTESIAN_POINT ( 'NONE',  ( 112.6828081442453282, -7.893985811506177619, -18.51759400769804742 ) ) ;
#13236 = CARTESIAN_POINT ( 'NONE',  ( 105.8986608795248401, -8.938348069036489818, -9.318865927141430916 ) ) ;
#13237 = CARTESIAN_POINT ( 'NONE',  ( 105.1346765045248475, -2.791137627527939813, -8.388885654883777576 ) ) ;
#13238 = CARTESIAN_POINT ( 'NONE',  ( 106.4542858795248179, -8.402594152722688392, -9.854619843455216355 ) ) ;
#13239 = CIRCLE ( 'NONE', #38692, 2.999999999999999556 ) ;
#13240 = EDGE_CURVE ( 'NONE', #37616, #34939, #19736, .T. ) ;
#13241 = PLANE ( 'NONE',  #34212 ) ;
#13242 = CARTESIAN_POINT ( 'NONE',  ( 117.7314814775786260, -4.089484607189486809, -7.948022111789456723 ) ) ;
#13243 = ORIENTED_EDGE ( 'NONE', *, *, #16294, .T. ) ;
#13244 = CARTESIAN_POINT ( 'NONE',  ( 125.4463081442452932, -5.638512984488999180, -18.83840828888717311 ) ) ;
#13245 = CARTESIAN_POINT ( 'NONE',  ( 69.36136150295220659, -54.40876771024655056, -31.86151892959740550 ) ) ;
#13246 = CARTESIAN_POINT ( 'NONE',  ( 119.4332814775786318, -8.899110576539710493, -16.42337572283490132 ) ) ;
#13247 = CARTESIAN_POINT ( 'NONE',  ( 124.0495485609119584, -10.36940331770107093, -15.09355782777061350 ) ) ;
#13248 = CARTESIAN_POINT ( 'NONE',  ( 122.0427081442452817, 0.5811942927096110934, -14.16772938898807510 ) ) ;
#13249 = CARTESIAN_POINT ( 'NONE',  ( 105.8292077545248446, -7.250697342233347165, -7.631215200338321125 ) ) ;
#13250 = DIRECTION ( 'NONE',  ( 0.7871354856660167654, -0.6167752151498625546, -0.002461946824136807422 ) ) ;
#13251 = VERTEX_POINT ( 'NONE', #10707 ) ;
#13252 = CARTESIAN_POINT ( 'NONE',  ( 112.6260814775786514, -9.261995988541697145, -16.69588392320189030 ) ) ;
#13253 = CARTESIAN_POINT ( 'NONE',  ( 124.1983214775786166, -1.833838273342659697, -17.42832698103878286 ) ) ;
#13254 = CARTESIAN_POINT ( 'NONE',  ( 120.2841814775786276, 0.9020085738987339008, -11.91225656197089222 ) ) ;
#13255 = CARTESIAN_POINT ( 'NONE',  ( 113.3635281442453504, -0.1624402480850797581, -16.17319339645315424 ) ) ;
#13256 = CARTESIAN_POINT ( 'NONE',  ( 118.1285681442453068, -7.893985811506177619, -18.51759400769804742 ) ) ;
#13257 = CARTESIAN_POINT ( 'NONE',  ( 127.0264730702703417, -1.258626024824194056, -9.367719562983635839 ) ) ;
#13258 = CARTESIAN_POINT ( 'NONE',  ( 119.0361948109119652, -2.084020599724406786, -8.691656652584148546 ) ) ;
#13259 = ORIENTED_EDGE ( 'NONE', *, *, #38644, .T. ) ;
#13260 = CARTESIAN_POINT ( 'NONE',  ( 123.2161110609119561, -3.163656168406935087, -18.89861972220014508 ) ) ;
#13261 = CARTESIAN_POINT ( 'NONE',  ( 116.0296814775786345, -8.166667518702817929, -8.995218007635861213 ) ) ;
#13262 = CARTESIAN_POINT ( 'NONE',  ( 120.0572748109119772, -6.222761293078241884, -8.102969835052219238 ) ) ;
#13263 = ORIENTED_EDGE ( 'NONE', *, *, #28400, .T. ) ;
#13264 = CARTESIAN_POINT ( 'NONE',  ( 122.4521266859119635, -9.033780868592240054, -16.85052413769862056 ) ) ;
#13265 = CARTESIAN_POINT ( 'NONE',  ( 136.6675107540917793, -1.259382374902307422, -9.019811723025741301 ) ) ;
#13266 = CARTESIAN_POINT ( 'NONE',  ( 118.4689281442453392, 0.9020085738987339008, -11.91225656197089222 ) ) ;
#13267 = CARTESIAN_POINT ( 'NONE',  ( 111.1076452545248259, 0.8980012041604421569, -11.00651665394454071 ) ) ;
#13268 = CARTESIAN_POINT ( 'NONE',  ( 115.2922348109119781, 0.4262465694468514643, -12.03445270309931736 ) ) ;
#13269 = EDGE_LOOP ( 'NONE', ( #1886, #1904, #35980, #16428 ) ) ;
#13270 = VERTEX_POINT ( 'NONE', #17763 ) ;
#13271 = CIRCLE ( 'NONE', #27104, 6.000000000000000888 ) ;
#13272 = CARTESIAN_POINT ( 'NONE',  ( 124.3117748109119844, 0.1319031606808879209, -14.10382304977623669 ) ) ;
#13273 = DIRECTION ( 'NONE',  ( 1.000000000000000000, 0.000000000000000000, -0.000000000000000000 ) ) ;
#13274 = FILL_AREA_STYLE ('',( #2314 ) ) ;
#13275 = DIRECTION ( 'NONE',  ( 1.000000000000000000, 0.000000000000000000, -0.000000000000000000 ) ) ;
#13276 = CARTESIAN_POINT ( 'NONE',  ( 122.3263414775786373, -6.344957434206665248, -7.627207830600338134 ) ) ;
#13277 = CARTESIAN_POINT ( 'NONE',  ( 109.2294421295247844, 0.1210096558822565393, -14.64321520034217805 ) ) ;
#13278 = CIRCLE ( 'NONE', #11086, 3.853420195439741125 ) ;
#13279 = PLANE ( 'NONE',  #16443 ) ;
#13280 = CARTESIAN_POINT ( 'NONE',  ( 121.5321681442453183, -9.988377603198976828, -10.36322818467138340 ) ) ;
#13282 = CARTESIAN_POINT ( 'NONE',  ( 118.9794681442453026, -0.8288870151387760510, -10.36305467784173118 ) ) ;
#13281 = CARTESIAN_POINT ( 'NONE',  ( 120.2274548109119934, 0.5811942927096110934, -14.16772938898807510 ) ) ;
#13283 = DIRECTION ( 'NONE',  ( 0.000000000000000000, 0.000000000000000000, -1.000000000000000000 ) ) ;
#13284 = DIRECTION ( 'NONE',  ( -1.000000000000000000, 0.000000000000000000, 0.000000000000000000 ) ) ;
#13285 = EDGE_LOOP ( 'NONE', ( #568, #28012, #40340, #30867 ) ) ;
#13286 = CARTESIAN_POINT ( 'NONE',  ( 125.1059481442452750, -1.833838273342660141, -17.42832698103878286 ) ) ;
#13287 = CARTESIAN_POINT ( 'NONE',  ( 122.2469553663348449, -1.172797794773259072, -17.05961127468926719 ) ) ;
#13288 = DIRECTION ( 'NONE',  ( 0.000000000000000000, 0.9242245927363029745, 0.3818493186865928868 ) ) ;
#13289 = CARTESIAN_POINT ( 'NONE',  ( 108.8851452545248151, 0.8980012041604421569, -11.00651665394454071 ) ) ;
#13290 = CARTESIAN_POINT ( 'NONE',  ( 112.1494421295248003, -9.868328341294093420, -13.39321520033831447 ) ) ;
#13291 = CARTESIAN_POINT ( 'NONE',  ( 106.3153796295248412, -4.863998795839590272, -19.15521520033831493 ) ) ;
#13292 = CARTESIAN_POINT ( 'NONE',  ( 123.5743281442453139, -7.893985811506177619, -18.51759400769804742 ) ) ;
#13293 = CARTESIAN_POINT ( 'NONE',  ( 122.6667014775786413, -2.084020599724406786, -8.691656652584148546 ) ) ;
#13294 = VERTEX_POINT ( 'NONE', #25059 ) ;
#13295 = CARTESIAN_POINT ( 'NONE',  ( 125.1626748109119802, -9.988377603198980381, -10.36322818467138518 ) ) ;
#13296 = CARTESIAN_POINT ( 'NONE',  ( 114.2144281442453178, -1.833838273342658809, -17.42832698103878286 ) ) ;
#13297 = CARTESIAN_POINT ( 'NONE',  ( 121.6456214775786435, 0.4262465694468626776, -12.03445270309935111 ) ) ;
#13298 = CARTESIAN_POINT ( 'NONE',  ( 121.5321681442453183, -9.988377603198976828, -10.36322818467138340 ) ) ;
#13299 = CARTESIAN_POINT ( 'NONE',  ( 119.6034614775786196, -6.344957434206665248, -7.627207830600338134 ) ) ;
#13300 = CARTESIAN_POINT ( 'NONE',  ( 119.5319204359119993, 0.5245030254254168245, -13.89657392289387516 ) ) ;
#13301 = CARTESIAN_POINT ( 'NONE',  ( 126.3539348109119800, -4.153390946401325223, -8.397313243818185668 ) ) ;
#13302 = VECTOR ( 'NONE', #15039, 1000.000000000000000 ) ;
#13303 = DIRECTION ( 'NONE',  ( -0.2768435750659241079, -0.3568721902840695792, 0.8921882507333129819 ) ) ;
#13304 = CARTESIAN_POINT ( 'NONE',  ( 105.4819421295248247, 0.8980012041604618078, -13.39321520033831447 ) ) ;
#13305 = ORIENTED_EDGE ( 'NONE', *, *, #35388, .T. ) ;
#13306 = CARTESIAN_POINT ( 'NONE',  ( 94.20708369096698220, -25.99489077589524300, -13.39321520033831447 ) ) ;
#13307 = CARTESIAN_POINT ( 'NONE',  ( 114.2719877074049037, -2.419733177069680607, -17.89711025544712442 ) ) ;
#13308 = CIRCLE ( 'NONE', #30019, 2.000000000000000444 ) ;
#13309 = CARTESIAN_POINT ( 'NONE',  ( 122.1561614775786353, -8.899110576539710493, -16.42337572283490132 ) ) ;
#13310 = CARTESIAN_POINT ( 'NONE',  ( 107.5655358795247736, -8.402594152722688392, -9.854619843455216355 ) ) ;
#13311 = CARTESIAN_POINT ( 'NONE',  ( 109.5796765045248122, -2.791137627527939813, -8.388885654883777576 ) ) ;
#13312 = CARTESIAN_POINT ( 'NONE',  ( 120.6812681442452941, 0.1319031606808879209, -14.10382304977623669 ) ) ;
#13313 =( NAMED_UNIT ( * ) PLANE_ANGLE_UNIT ( ) SI_UNIT ( $, .RADIAN. ) );
#13314 = CARTESIAN_POINT ( 'NONE',  ( 115.1220548109119761, -1.833838273342658809, -17.42832698103878286 ) ) ;
#13315 = CARTESIAN_POINT ( 'NONE',  ( 123.2906948109119867, -8.166667518702819706, -8.995218007635861213 ) ) ;
#13316 = ORIENTED_EDGE ( 'NONE', *, *, #6698, .F. ) ;
#13317 = STYLED_ITEM ( 'NONE', ( #31403 ), #6345 ) ;
#13318 = EDGE_CURVE ( 'NONE', #11704, #17071, #876, .T. ) ;
#13319 = CARTESIAN_POINT ( 'NONE',  ( 122.4397948109119767, -0.1624402480850797581, -16.17319339645315424 ) ) ;
#13320 = CIRCLE ( 'NONE', #38765, 2.999999999999999556 ) ;
#13321 = CARTESIAN_POINT ( 'NONE',  ( 117.9016614775786280, -9.988377603198976828, -10.36322818467138340 ) ) ;
#13322 = CARTESIAN_POINT ( 'NONE',  ( 125.6164881442453094, 0.2603800115204892296, -16.42320221600525088 ) ) ;
#13323 = CARTESIAN_POINT ( 'NONE',  ( 124.8223148109119762, -10.15424416112533912, -14.75197769757731336 ) ) ;
#13324 = ORIENTED_EDGE ( 'NONE', *, *, #25101, .T. ) ;
#13325 = CARTESIAN_POINT ( 'NONE',  ( 123.5786714811013240, -2.280480477428469488, -18.08254604495227014 ) ) ;
#13326 = CARTESIAN_POINT ( 'NONE',  ( 124.1983214775786166, -8.166667518702819706, -8.995218007635861213 ) ) ;
#13327 = CARTESIAN_POINT ( 'NONE',  ( 115.5758681442453053, -7.894159318335828068, -9.358103419637847864 ) ) ;
#13328 = CARTESIAN_POINT ( 'NONE',  ( 124.4819548109119722, -7.893985811506177619, -18.51759400769804742 ) ) ;
#13329 = EDGE_CURVE ( 'NONE', #11788, #37616, #42166, .T. ) ;
#13330 = DIRECTION ( 'NONE',  ( 1.000000000000000000, 0.000000000000000000, -0.000000000000000000 ) ) ;
#13331 = EDGE_CURVE ( 'NONE', #9856, #44074, #40873, .T. ) ;
#13332 = ADVANCED_FACE ( 'NONE', ( #11828 ), #22750, .F. ) ;
#13333 = CARTESIAN_POINT ( 'NONE',  ( 124.3968141859119783, -8.321307733199551748, -9.223433127585318303 ) ) ;
#13334 = ORIENTED_EDGE ( 'NONE', *, *, #30046, .F. ) ;
#13335 = DIRECTION ( 'NONE',  ( -0.5735764363510450492, -0.3127926500124816878, 0.7570804645221038687 ) ) ;
#13336 = CARTESIAN_POINT ( 'NONE',  ( 61.00493324624891756, -4.079101092950570440, -7.393215200338313586 ) ) ;
#13337 = CARTESIAN_POINT ( 'NONE',  ( 116.3166296295247832, -4.863998795839590272, -19.15521520033831493 ) ) ;
#13338 = CIRCLE ( 'NONE', #40278, 5.999999999999997335 ) ;
#13339 = CARTESIAN_POINT ( 'NONE',  ( 70.19189222814998175, -49.76310523276723785, -29.87698278062876511 ) ) ;
#13340 = CARTESIAN_POINT ( 'NONE',  ( 123.9714148109119805, -8.899110576539710493, -16.42337572283490132 ) ) ;
#13341 = CARTESIAN_POINT ( 'NONE',  ( 112.8529881442453160, -7.894159318335828068, -9.358103419637847864 ) ) ;
#13342 = CARTESIAN_POINT ( 'NONE',  ( 127.7429221095975009, 0.4602738061672586589, -11.18760673166210218 ) ) ;
#13343 = VERTEX_POINT ( 'NONE', #1104 ) ;
#13344 = DIRECTION ( 'NONE',  ( -0.8949343913984424415, 0.4123869368673878100, 0.1703803081152053811 ) ) ;
#13345 = DIRECTION ( 'NONE',  ( 0.000000000000000000, 0.000000000000000000, -1.000000000000000000 ) ) ;
#13346 = VECTOR ( 'NONE', #1466, 1000.000000000000114 ) ;
#13347 = DIRECTION ( 'NONE',  ( -1.000000000000000000, 0.000000000000000000, 0.000000000000000000 ) ) ;
#13348 = CARTESIAN_POINT ( 'NONE',  ( 111.2751814775786556, -7.618532446445550832, -18.05174138884716228 ) ) ;
#13350 = CARTESIAN_POINT ( 'NONE',  ( 126.0703014775786102, -9.988377603198980381, -10.36322818467138518 ) ) ;
#13349 = CARTESIAN_POINT ( 'NONE',  ( 61.27778620743471549, -25.99489077589588604, -11.39321520033831447 ) ) ;
#13351 = CARTESIAN_POINT ( 'NONE',  ( 125.6732148109119862, -9.859900752359378018, -12.68260735090039759 ) ) ;
#13352 = ORIENTED_EDGE ( 'NONE', *, *, #44006, .T. ) ;
#13353 = CARTESIAN_POINT ( 'NONE',  ( 112.6828081442453282, -7.893985811506177619, -18.51759400769804742 ) ) ;
#13354 = CARTESIAN_POINT ( 'NONE',  ( 126.2184548109119788, -4.863998795839242995, -13.39321520033831447 ) ) ;
#13355 = CARTESIAN_POINT ( 'NONE',  ( 114.9970202545248412, -10.62599879583958717, -15.77991374673208469 ) ) ;
#13356 = CARTESIAN_POINT ( 'NONE',  ( 125.2761281442453054, 0.4262465694468514643, -12.03445270309931736 ) ) ;
#13357 = CARTESIAN_POINT ( 'NONE',  ( 123.2906948109119867, -1.833838273342659697, -17.42832698103878286 ) ) ;
#13358 = DIRECTION ( 'NONE',  ( -1.000000000000000000, 0.000000000000000000, -0.000000000000000000 ) ) ;
#13359 = CARTESIAN_POINT ( 'NONE',  ( 114.5108483795247878, -8.402594152722688392, -16.93181055722141792 ) ) ;
#13360 = EDGE_CURVE ( 'NONE', #44289, #30333, #40110, .T. ) ;
#13361 = CARTESIAN_POINT ( 'NONE',  ( 85.94012291206632881, -8.967540239925700263, -13.24321520033831412 ) ) ;
#13362 = DIRECTION ( 'NONE',  ( 0.2407039305251456596, -0.3604685577742790525, 0.9011792478113757054 ) ) ;
#13363 = CARTESIAN_POINT ( 'NONE',  ( 113.1366214775786432, -7.643976991954077427, -18.09477374809248928 ) ) ;
#13364 = CARTESIAN_POINT ( 'NONE',  ( 108.3295202545248657, -10.62599879583958717, -15.77991374673208469 ) ) ;
#13365 = DIRECTION ( 'NONE',  ( 1.000000000000000000, 0.000000000000000000, 0.000000000000000000 ) ) ;
#13366 = CARTESIAN_POINT ( 'NONE',  ( 113.7468640045248236, -10.62599879583958717, -11.00651665394454604 ) ) ;
#13367 = CARTESIAN_POINT ( 'NONE',  ( 125.7299414775786346, 0.9020085738987339008, -11.91225656197089222 ) ) ;
#13368 = CARTESIAN_POINT ( 'NONE',  ( 122.4965214775786251, -10.30919188438810075, -12.61870101168855918 ) ) ;
#13369 = FACE_OUTER_BOUND ( 'NONE', #21438, .T. ) ;
#13370 = EDGE_CURVE ( 'NONE', #14709, #22330, #39415, .T. ) ;
#13371 = CARTESIAN_POINT ( 'NONE',  ( 118.5256548109119876, -0.4660016031367893996, -10.09054647747474043 ) ) ;
#13372 = CARTESIAN_POINT ( 'NONE',  ( 112.7962614775786676, -3.383040157471821630, -19.15922257007629170 ) ) ;
#13373 = ORIENTED_EDGE ( 'NONE', *, *, #41494, .T. ) ;
#13374 = CARTESIAN_POINT ( 'NONE',  ( 112.2857214775786474, -5.574606645277164318, -18.38911715685844683 ) ) ;
#13375 = AXIS2_PLACEMENT_3D ( 'NONE', #19401, #33288, #43807 ) ;
#13376 = ADVANCED_FACE ( 'NONE', ( #43740 ), #25958, .T. ) ;
#13377 = CARTESIAN_POINT ( 'NONE',  ( 124.8790414775786246, -0.4660016031367893996, -10.09054647747474043 ) ) ;
#13378 = CIRCLE ( 'NONE', #32983, 6.000000000000005329 ) ;
#13379 = CARTESIAN_POINT ( 'NONE',  ( 122.6099748109119929, -9.261995988541697145, -16.69588392320189030 ) ) ;
#13380 = CARTESIAN_POINT ( 'NONE',  ( 116.0296814775786345, -8.166667518702817929, -8.995218007635861213 ) ) ;
#13381 = CARTESIAN_POINT ( 'NONE',  ( 111.2646414775786496, -8.899110576539710493, -16.42337572283490132 ) ) ;
#13382 = VERTEX_POINT ( 'NONE', #32774 ) ;
#13383 = CARTESIAN_POINT ( 'NONE',  ( 117.4478481442453131, -9.565557343593413364, -10.61323700422348004 ) ) ;
#13384 = CARTESIAN_POINT ( 'NONE',  ( 113.1366214775786432, -1.834011780172310813, -8.268836392978581529 ) ) ;
#13385 = CIRCLE ( 'NONE', #25736, 5.000000000000004441 ) ;
#13386 = CARTESIAN_POINT ( 'NONE',  ( 123.0637881442452937, -8.899110576539710493, -16.42337572283490132 ) ) ;
#13387 = CARTESIAN_POINT ( 'NONE',  ( 116.8455752247359953, -0.8306836925769603974, -16.75873294673692726 ) ) ;
#13388 = CARTESIAN_POINT ( 'NONE',  ( 113.4690515045247992, -2.477300249445798297, -7.631215200338321125 ) ) ;
#13389 = ORIENTED_EDGE ( 'NONE', *, *, #45120, .F. ) ;
#13390 = ADVANCED_FACE ( 'NONE', ( #8178 ), #37190, .T. ) ;
#13391 = FACE_OUTER_BOUND ( 'NONE', #44259, .T. ) ;
#13392 = CARTESIAN_POINT ( 'NONE',  ( 83.75466360696344736, -7.807702403958562520, -18.64321520033831803 ) ) ;
#13393 = DIRECTION ( 'NONE',  ( 0.9609149988134843001, -0.1028163501681632064, 0.2570431154366505933 ) ) ;
#13394 = CARTESIAN_POINT ( 'NONE',  ( 112.8529881442453302, -1.561330072975668060, -17.79121239304076596 ) ) ;
#13395 = CARTESIAN_POINT ( 'NONE',  ( 116.7494664628001004, 2.044003616876136853, -5.959107281052824057 ) ) ;
#13396 = CARTESIAN_POINT ( 'NONE',  ( 121.4618602343419411, -8.309924745830986836, -17.19909913565936321 ) ) ;
#13397 =( BOUNDED_CURVE ( )  B_SPLINE_CURVE ( 2, ( #27736, #24317, #23416, #34109, #9735, #19763, #2879, #30923, #30473 ),
 .UNSPECIFIED., .F., .F. ) 
 B_SPLINE_CURVE_WITH_KNOTS ( ( 3, 2, 2, 2, 3 ),
 ( 0.04111889706057585137, 0.1249999999999965999, 0.2499999999999915068, 0.3749999999999864553, 0.4999999999999819589 ),
 .UNSPECIFIED. ) 
 CURVE ( )  GEOMETRIC_REPRESENTATION_ITEM ( )  RATIONAL_B_SPLINE_CURVE ( ( 0.9663939858628909363, 0.9489194498462569793, 1.000000000000000000, 0.9238795325112869605, 1.000000000000000000, 0.9238795325112869605, 1.000000000000000000, 0.9238795325112979517, 0.9999999999999890088 ) ) 
 REPRESENTATION_ITEM ( '' )  );
#13398 = CARTESIAN_POINT ( 'NONE',  ( 105.8292077545248446, -2.791137627527939813, -18.39754474579286025 ) ) ;
#13399 = CARTESIAN_POINT ( 'NONE',  ( 94.20708369096698220, -26.72956082974378944, -12.96372607128127363 ) ) ;
#13400 = CARTESIAN_POINT ( 'NONE',  ( 118.6958348109119754, -6.344957434206665248, -7.627207830600338134 ) ) ;
#13401 = CARTESIAN_POINT ( 'NONE',  ( 122.5664060953690466, -6.001247023715324147, -18.26661038929047010 ) ) ;
#13402 = FACE_OUTER_BOUND ( 'NONE', #23914, .T. ) ;
#13403 = CARTESIAN_POINT ( 'NONE',  ( 124.2610829359120004, -4.360640073283988727, -8.004713379073630009 ) ) ;
#13404 = CARTESIAN_POINT ( 'NONE',  ( 119.9438214775786378, -2.084020599724406786, -8.691656652584148546 ) ) ;
#13405 = ORIENTED_EDGE ( 'NONE', *, *, #26777, .F. ) ;
#13406 = CARTESIAN_POINT ( 'NONE',  ( 125.7299414775786346, 0.9020085738987339008, -11.91225656197089222 ) ) ;
#13407 = CARTESIAN_POINT ( 'NONE',  ( 118.8092881442453290, -9.988377603198976828, -10.36322818467138340 ) ) ;
#13408 = CARTESIAN_POINT ( 'NONE',  ( 114.2144281442453178, -1.833838273342658809, -17.42832698103878286 ) ) ;
#13409 = CARTESIAN_POINT ( 'NONE',  ( 125.5030348109119558, -3.383040157471821630, -19.15922257007629170 ) ) ;
#13410 = CARTESIAN_POINT ( 'NONE',  ( 110.9687390045248350, 0.8980012041604421569, -15.77991374673208469 ) ) ;
#13411 = DIRECTION ( 'NONE',  ( 1.000000000000000000, 0.000000000000000000, -0.000000000000000000 ) ) ;
#13412 = CARTESIAN_POINT ( 'NONE',  ( 82.69078301141780685, -31.77851515411413885, -23.07115788542655821 ) ) ;
#13413 = CIRCLE ( 'NONE', #19223, 2.999999999999999556 ) ;
#13414 = CARTESIAN_POINT ( 'NONE',  ( 117.0507614775786465, 0.1319031606808879209, -14.10382304977623669 ) ) ;
#13415 = CARTESIAN_POINT ( 'NONE',  ( 119.0361948109119652, -2.084020599724406786, -8.691656652584148546 ) ) ;
#13416 = DIRECTION ( 'NONE',  ( 0.9908103287288504424, -0.1352586133457958084, 0.000000000000000000 ) ) ;
#13417 = CYLINDRICAL_SURFACE ( 'NONE', #10917, 5.132259260909280307 ) ;
#13418 = CARTESIAN_POINT ( 'NONE',  ( 109.2324108795247923, -1.325403438956436419, -16.93181055722141792 ) ) ;
#13419 = VERTEX_POINT ( 'NONE', #32560 ) ;
#13420 = CARTESIAN_POINT ( 'NONE',  ( 109.2294467943806353, -0.4195948248842314432, -15.84472584932758821 ) ) ;
#13421 = CARTESIAN_POINT ( 'NONE',  ( 114.8384214775786489, 0.9020085738987339008, -11.91225656197089222 ) ) ;
#13422 = CARTESIAN_POINT ( 'NONE',  ( 9.052690036452151645, -4.182915634381243919, -8.893215200338314474 ) ) ;
#13423 = CARTESIAN_POINT ( 'NONE',  ( 123.4244704359119709, -10.25716656981731489, -12.88942061488890545 ) ) ;
#13424 = CARTESIAN_POINT ( 'NONE',  ( 121.0630641859119976, -8.321307733199551748, -9.223433127585318303 ) ) ;
#13425 = ORIENTED_EDGE ( 'NONE', *, *, #41032, .F. ) ;
#13426 = DIRECTION ( 'NONE',  ( 0.000000000000000000, 0.6161630946014901022, 0.7876185884367606915 ) ) ;
#13427 = CARTESIAN_POINT ( 'NONE',  ( 116.8640794598117907, -11.66681915340833520, -21.47304352488360379 ) ) ;
#13428 = ORIENTED_EDGE ( 'NONE', *, *, #44692, .F. ) ;
#13429 = CARTESIAN_POINT ( 'NONE',  ( 123.0070614775786169, 0.9020085738987339008, -11.91225656197089222 ) ) ;
#13430 = CARTESIAN_POINT ( 'NONE',  ( 114.6682414775786469, -1.561330072975668060, -17.79121239304076596 ) ) ;
#13431 = CARTESIAN_POINT ( 'NONE',  ( 120.1140014775786398, -7.894159318335828068, -9.358103419637847864 ) ) ;
#13432 = CARTESIAN_POINT ( 'NONE',  ( 120.2537320239009375, -8.246984259551265239, -17.07990705884998661 ) ) ;
#13433 = CARTESIAN_POINT ( 'NONE',  ( 120.5110881442453206, -6.344957434206665248, -7.627207830600338134 ) ) ;
#13434 = CARTESIAN_POINT ( 'NONE',  ( 118.4122014775786340, 0.5811942927096110934, -14.16772938898807510 ) ) ;
#13435 = EDGE_CURVE ( 'NONE', #28262, #15443, #5172, .T. ) ;
#13436 = CARTESIAN_POINT ( 'NONE',  ( 107.4266296295248821, -4.863998795839590272, -8.388885654883775800 ) ) ;
#13437 = CARTESIAN_POINT ( 'NONE',  ( 113.6471614775786492, -4.153390946401321671, -8.397313243818183892 ) ) ;
#13438 = CARTESIAN_POINT ( 'NONE',  ( 135.3184548109119874, -1.191816558809784876, -8.648209655763537285 ) ) ;
#13439 = ORIENTED_EDGE ( 'NONE', *, *, #41794, .T. ) ;
#13440 = CARTESIAN_POINT ( 'NONE',  ( 117.2776681442452968, -5.638512984488999180, -18.83840828888717311 ) ) ;
#13441 = CARTESIAN_POINT ( 'NONE',  ( 121.1325173109119788, 0.2312338769422704887, -16.08380026872395874 ) ) ;
#13442 = CARTESIAN_POINT ( 'NONE',  ( 115.5191414775786569, -3.383040157471821630, -19.15922257007629170 ) ) ;
#13443 = EDGE_LOOP ( 'NONE', ( #32627, #38198 ) ) ;
#13444 = CARTESIAN_POINT ( 'NONE',  ( 121.9859814775786333, 0.2603800115204892296, -16.42320221600525088 ) ) ;
#13445 = LINE ( 'NONE', #23247, #27456 ) ;
#13446 = DIRECTION ( 'NONE',  ( 0.000000000000000000, 0.000000000000000000, -1.000000000000000000 ) ) ;
#13447 = DIRECTION ( 'NONE',  ( -1.000000000000000000, 0.000000000000000000, -0.000000000000000000 ) ) ;
#13448 = ADVANCED_FACE ( 'NONE', ( #22310 ), #3712, .T. ) ;
#13449 = CARTESIAN_POINT ( 'NONE',  ( 115.0653281442453277, -3.505236298600246325, -18.68346056562440793 ) ) ;
#13450 = DIRECTION ( 'NONE',  ( -0.000000000000000000, -0.9284778069183721172, -0.3713878862591650232 ) ) ;
#13451 = CARTESIAN_POINT ( 'NONE',  ( 117.7882081442453170, -3.505236298600246325, -18.68346056562440793 ) ) ;
#13452=STYLED_ITEM('',(#45190),#36189);
#13453 = LINE ( 'NONE', #25500, #37619 ) ;
#13454 = CARTESIAN_POINT ( 'NONE',  ( 116.3133148109120043, -2.084020599724406786, -8.691656652584148546 ) ) ;
#13455 = CARTESIAN_POINT ( 'NONE',  ( 114.2144281442453178, -8.166667518702817929, -8.995218007635859436 ) ) ;
#13456 = CARTESIAN_POINT ( 'NONE',  ( 121.2714235609119697, 0.6414057260225851653, -11.69287257290600657 ) ) ;
#13457 = CARTESIAN_POINT ( 'NONE',  ( 117.0507614775786465, -10.30919188438810075, -12.61870101168855918 ) ) ;
#13458 = CARTESIAN_POINT ( 'NONE',  ( 113.8173414775786512, -9.565557343593413364, -10.61323700422348004 ) ) ;
#13459 = CARTESIAN_POINT ( 'NONE',  ( 111.5482748109120053, -0.1624402480850797581, -16.17319339645315424 ) ) ;
#13460 = AXIS2_PLACEMENT_3D ( 'NONE', #11635, #42877, #35333 ) ;
#13461 = CARTESIAN_POINT ( 'NONE',  ( 116.5969481442453031, -9.859900752359374465, -12.68260735090039404 ) ) ;
#13462 = ORIENTED_EDGE ( 'NONE', *, *, #33087, .F. ) ;
#13463 = CARTESIAN_POINT ( 'NONE',  ( 112.6260814775786514, -9.261995988541697145, -16.69588392320189030 ) ) ;
#13464 = CARTESIAN_POINT ( 'NONE',  ( 107.4266296295248821, -4.863998795839590272, -19.15521520033831493 ) ) ;
#13465 = CARTESIAN_POINT ( 'NONE',  ( 106.1070202545248407, 0.1403307496149616695, -11.32035403202665336 ) ) ;
#13466 = CARTESIAN_POINT ( 'NONE',  ( 110.5511756189168011, -1.701529060415639671, -16.35552654288092356 ) ) ;
#13467 = DIRECTION ( 'NONE',  ( -0.000000000000000000, -0.9284778069183721172, -0.3713878862591650232 ) ) ;
#13468 = CARTESIAN_POINT ( 'NONE',  ( 117.8449348109119938, -8.166667518702817929, -8.995218007635861213 ) ) ;
#13469 = ORIENTED_EDGE ( 'NONE', *, *, #39772, .T. ) ;
#13470 = CARTESIAN_POINT ( 'NONE',  ( 115.7097481608379894, 0.3867979994853637526, -14.64321520033831447 ) ) ;
#13471 = CARTESIAN_POINT ( 'NONE',  ( 125.2194014775786286, -10.30919188438809542, -12.61870101168851832 ) ) ;
#13472 = CARTESIAN_POINT ( 'NONE',  ( 119.6601881442453106, -1.833838273342659253, -17.42832698103878286 ) ) ;
#13473 = CARTESIAN_POINT ( 'NONE',  ( 123.2161110609119561, -3.163656168406935087, -18.89861972220014508 ) ) ;
#13474 = CARTESIAN_POINT ( 'NONE',  ( 125.2194014775786286, -10.30919188438810075, -12.61870101168855918 ) ) ;
#13475 = CARTESIAN_POINT ( 'NONE',  ( 107.7044421295247929, 0.8980012041604618078, -13.39321520033831447 ) ) ;
#13476 = DIRECTION ( 'NONE',  ( -1.000000000000000000, 0.000000000000000000, -0.000000000000000000 ) ) ;
#13477 = ORIENTED_EDGE ( 'NONE', *, *, #22503, .T. ) ;
#13478 = CARTESIAN_POINT ( 'NONE',  ( 113.0231681442453322, 0.9020085738987339008, -11.91225656197089222 ) ) ;
#13479 = CARTESIAN_POINT ( 'NONE',  ( 121.9292548109119849, -7.894159318335828068, -9.358103419637847864 ) ) ;
#13480 = CARTESIAN_POINT ( 'NONE',  ( 123.0637881442452937, -0.4660016031367893996, -10.09054647747474043 ) ) ;
#13481 = CARTESIAN_POINT ( 'NONE',  ( 115.2922348109119781, 0.4262465694468514643, -12.03445270309931736 ) ) ;
#13482 =( BOUNDED_SURFACE ( )  B_SPLINE_SURFACE ( 3, 2, ( 
 ( #15405, #32490, #11760 ),
 ( #15631, #43451, #35686 ),
 ( #812, #18599, #29081 ),
 ( #42778, #39349, #11989 ),
 ( #25447, #4230, #8117 ),
 ( #29535, #18149, #29309 ),
 ( #28643, #25670, #39575 ),
 ( #1265, #22018, #14731 ),
 ( #42993, #4461, #1037 ),
 ( #7653, #15175, #12216 ),
 ( #42549, #11310, #25220 ),
 ( #8338, #38884, #43222 ),
 ( #7885, #22238, #39119 ),
 ( #18382, #25890, #4678 ),
 ( #35912, #1483, #22464 ),
 ( #36358, #32270, #36135 ) ),
 .UNSPECIFIED., .F., .F., .T. ) 
 B_SPLINE_SURFACE_WITH_KNOTS ( ( 4, 2, 2, 2, 2, 2, 2, 4 ),
 ( 3, 3 ),
 ( 0.000000000000000000, 0.001721956341060625019, 0.002582934511590937419, 0.003443912682121250037, 0.004304890852651562655, 0.005165869023181874839, 0.006026847193712187023, 0.006887825364242500074 ),
 ( 0.000000000000000000, 1.000000000000000000 ),
 .UNSPECIFIED. ) 
 GEOMETRIC_REPRESENTATION_ITEM ( )  RATIONAL_B_SPLINE_SURFACE ( (
 ( 1.000000000000000000, 0.7145271066604784727, 1.000000000000000000),
 ( 1.000000000000000000, 0.7222084595711586452, 1.000000000000000000),
 ( 1.000000000000000000, 0.7248469248598453651, 1.000000000000000000),
 ( 1.000000000000000000, 0.7198061150658591201, 1.000000000000000000),
 ( 1.000000000000000000, 0.7166464354070819498, 1.000000000000000000),
 ( 1.000000000000000000, 0.7075576805112285816, 1.000000000000000000),
 ( 1.000000000000000000, 0.7016223805004251357, 1.000000000000000000),
 ( 1.000000000000000000, 0.6870357897293317695, 1.000000000000000000),
 ( 1.000000000000000000, 0.6784576229549662552, 1.000000000000000000),
 ( 1.000000000000000000, 0.6592514108187733646, 1.000000000000000000),
 ( 1.000000000000000000, 0.6485859927021864202, 1.000000000000000000),
 ( 1.000000000000000000, 0.6253175026863306840, 1.000000000000000000),
 ( 1.000000000000000000, 0.6127418264104756984, 1.000000000000000000),
 ( 1.000000000000000000, 0.5864433665304108478, 1.000000000000000000),
 ( 1.000000000000000000, 0.5726514202820954802, 1.000000000000000000),
 ( 1.000000000000000000, 0.5583088333832483263, 1.000000000000000000) ) ) 
 REPRESENTATION_ITEM ( '' )  SURFACE ( )  );
#13483 = CARTESIAN_POINT ( 'NONE',  ( 119.7169148109119874, -9.988377603198976828, -10.36322818467138340 ) ) ;
#13484 = FACE_OUTER_BOUND ( 'NONE', #22578, .T. ) ;
#13485 = CARTESIAN_POINT ( 'NONE',  ( 127.2313854076961519, -1.266593818456560827, -9.224256396174785877 ) ) ;
#13486 = CARTESIAN_POINT ( 'NONE',  ( 121.4754414775786131, -1.833838273342659697, -17.42832698103878286 ) ) ;
#13487 = VERTEX_POINT ( 'NONE', #42840 ) ;
#13488 = CARTESIAN_POINT ( 'NONE',  ( 116.5960802213312775, -9.865703544234238009, -13.38317263089577480 ) ) ;
#13489 = CARTESIAN_POINT ( 'NONE',  ( 117.1642148109119859, -9.261995988541697145, -16.69588392320189030 ) ) ;
#13490 = CARTESIAN_POINT ( 'NONE',  ( 125.3328548109119964, -0.8288870151387760510, -10.36305467784173118 ) ) ;
#13491 = ORIENTED_EDGE ( 'NONE', *, *, #12303, .T. ) ;
#13492 = CARTESIAN_POINT ( 'NONE',  ( 123.1466579359119891, -5.444069387712269226, -19.60292469916370450 ) ) ;
#13493 = FACE_OUTER_BOUND ( 'NONE', #26819, .T. ) ;
#13494 = CARTESIAN_POINT ( 'NONE',  ( 117.5045748109119756, 0.5811942927096110934, -14.16772938898807510 ) ) ;
#13495 = CARTESIAN_POINT ( 'NONE',  ( 108.1906140045248463, -10.62599879583958717, -11.00651665394454604 ) ) ;
#13496 = CARTESIAN_POINT ( 'NONE',  ( 119.0929214775786278, -4.153390946401325223, -8.397313243818185668 ) ) ;
#13497 = ORIENTED_EDGE ( 'NONE', *, *, #32531, .T. ) ;
#13498 = ORIENTED_EDGE ( 'NONE', *, *, #26991, .T. ) ;
#13499 = CARTESIAN_POINT ( 'NONE',  ( 111.8886348109120092, -3.383040157471821630, -19.15922257007629170 ) ) ;
#13500 = EDGE_CURVE ( 'NONE', #27420, #1626, #12510, .T. ) ;
#13501 = CARTESIAN_POINT ( 'NONE',  ( 123.3474214775786209, -0.1624402480850797581, -16.17319339645315424 ) ) ;
#13502 = CARTESIAN_POINT ( 'NONE',  ( 122.6009548109119720, -12.80254289275730173, -14.38292102596908784 ) ) ;
#13503 = CARTESIAN_POINT ( 'NONE',  ( 59.36680634945872725, -12.84644995903807896, -17.39321520033831447 ) ) ;
#13504 = CARTESIAN_POINT ( 'NONE',  ( 120.2841814775786276, 0.9020085738987339008, -11.91225656197089222 ) ) ;
#13505 = CARTESIAN_POINT ( 'NONE',  ( 109.2946629278414861, 0.02815652521716283108, -14.64321520033829493 ) ) ;
#13506 = CARTESIAN_POINT ( 'NONE',  ( 91.23658249893594530, -5.844616714554617509, -16.89321520033831447 ) ) ;
#13507 = CARTESIAN_POINT ( 'NONE',  ( 118.5256548109119876, -0.4660016031367893996, -10.09054647747474043 ) ) ;
#13509 = CARTESIAN_POINT ( 'NONE',  ( 118.8092881442453290, -0.1624402480850797581, -16.17319339645315424 ) ) ;
#13508 = CARTESIAN_POINT ( 'NONE',  ( 117.3911214775786505, -1.561330072975668504, -17.79121239304076951 ) ) ;
#13510 = CARTESIAN_POINT ( 'NONE',  ( 125.5597614775786326, -7.894159318335828068, -9.358103419637847864 ) ) ;
#13511 = CARTESIAN_POINT ( 'NONE',  ( 117.6747548109119919, -1.834011780172310813, -8.268836392978581529 ) ) ;
#13512 = ORIENTED_EDGE ( 'NONE', *, *, #16225, .T. ) ;
#13513 = CARTESIAN_POINT ( 'NONE',  ( 121.9859814775786333, -9.565557343593413364, -10.61323700422348004 ) ) ;
#13514 = CARTESIAN_POINT ( 'NONE',  ( 125.1626748109119802, -0.1624402480845399399, -16.17319339645223053 ) ) ;
#13515 = CARTESIAN_POINT ( 'NONE',  ( 110.1353015045248469, -2.477300249445798297, -7.631215200338321125 ) ) ;
#13516 = CARTESIAN_POINT ( 'NONE',  ( 112.8439733795247832, -1.325403438956436419, -9.854619843455211026 ) ) ;
#13517 = CARTESIAN_POINT ( 'NONE',  ( 107.4960827545248350, -2.477300249445798297, -19.15521520033831138 ) ) ;
#13518 = CARTESIAN_POINT ( 'NONE',  ( 120.6812681442452941, -10.30919188438810075, -12.61870101168855918 ) ) ;
#13519 = CARTESIAN_POINT ( 'NONE',  ( 122.7801548109119665, -6.222761293078241884, -8.102969835052219238 ) ) ;
#13520 = ORIENTED_EDGE ( 'NONE', *, *, #34184, .F. ) ;
#13521 = CARTESIAN_POINT ( 'NONE',  ( 123.8012348109119642, 0.2603800115204892296, -16.42320221600525088 ) ) ;
#13522 = CARTESIAN_POINT ( 'NONE',  ( 110.8992858795247827, -0.7896495226426338832, -17.46756447353520159 ) ) ;
#13523 = CARTESIAN_POINT ( 'NONE',  ( 112.2289948109119848, -7.643976991954077427, -18.09477374809248928 ) ) ;
#13524 = DIRECTION ( 'NONE',  ( 0.1352586133457952255, 0.9908103287288504424, 0.000000000000000000 ) ) ;
#13525 = CARTESIAN_POINT ( 'NONE',  ( 125.3895814775786448, -7.893985811506177619, -18.51759400769804742 ) ) ;
#13526 = CARTESIAN_POINT ( 'NONE',  ( 121.1918081442452859, 0.9020085738987339008, -11.91225656197089222 ) ) ;
#13528 = CIRCLE ( 'NONE', #18584, 1.587500000000000355 ) ;
#13527 = CARTESIAN_POINT ( 'NONE',  ( 70.19189222814998175, -62.62292920857806422, -38.25196254438899501 ) ) ;
#13529 = CARTESIAN_POINT ( 'NONE',  ( 113.3068014775786594, -8.166667518702817929, -8.995218007635859436 ) ) ;
#13530 = FACE_OUTER_BOUND ( 'NONE', #14808, .T. ) ;
#13531 = CARTESIAN_POINT ( 'NONE',  ( 114.1635827545248389, -6.936859964151250502, -8.388885654883777576 ) ) ;
#13532 = ORIENTED_EDGE ( 'NONE', *, *, #28069, .F. ) ;
#13533 = CARTESIAN_POINT ( 'NONE',  ( 83.83554121260367253, -24.14644159042263993, -12.62951656296512937 ) ) ;
#13534 = CARTESIAN_POINT ( 'NONE',  ( 118.5771691344827587, -1.149058757900091265, -17.09122335155388939 ) ) ;
#13535 = CARTESIAN_POINT ( 'NONE',  ( 124.3685014775786328, 0.4262465694468514643, -12.03445270309931736 ) ) ;
#13536 = CARTESIAN_POINT ( 'NONE',  ( 106.0375671295248310, 0.1403307496149613920, -13.39321520033831447 ) ) ;
#13537 = CARTESIAN_POINT ( 'NONE',  ( 108.7462390045248242, -9.868328341294098749, -11.32035403202665869 ) ) ;
#13538 = CARTESIAN_POINT ( 'NONE',  ( 123.1205148109119563, -7.643976991954077427, -18.09477374809248928 ) ) ;
#13539 = CARTESIAN_POINT ( 'NONE',  ( 114.8951481442453115, -8.899110576539710493, -16.42337572283490132 ) ) ;
#13540 = CARTESIAN_POINT ( 'NONE',  ( 113.1933481442453058, -5.574606645277164318, -18.38911715685844683 ) ) ;
#13541 = ORIENTED_EDGE ( 'NONE', *, *, #35642, .F. ) ;
#13542 = CARTESIAN_POINT ( 'NONE',  ( 125.4463081442452932, -4.153390946401325223, -8.397313243818185668 ) ) ;
#13543 = CARTESIAN_POINT ( 'NONE',  ( 117.1642148109119859, -9.261995988541697145, -16.69588392320189030 ) ) ;
#13544 = CARTESIAN_POINT ( 'NONE',  ( 61.69189222814998175, -48.76310523276723785, -23.89321520033831803 ) ) ;
#13545 = VERTEX_POINT ( 'NONE', #12057 ) ;
#13546 = CARTESIAN_POINT ( 'NONE',  ( 121.3168205993907378, -9.245649465415475277, -16.16453161350214884 ) ) ;
#13547 = ORIENTED_EDGE ( 'NONE', *, *, #37268, .F. ) ;
#13548 = CARTESIAN_POINT ( 'NONE',  ( 116.5969481442453031, -9.859900752359374465, -12.68260735090039404 ) ) ;
#13549 = CARTESIAN_POINT ( 'NONE',  ( 113.6471614775786492, -4.153390946401321671, -8.397313243818183892 ) ) ;
#13550 = CARTESIAN_POINT ( 'NONE',  ( 115.1220548109119761, -8.166667518702807271, -8.995218007635852331 ) ) ;
#13551 = TOROIDAL_SURFACE ( 'NONE', #31726, 4.500000000000000000, 1.500000000000000000 ) ;
#13552 = CARTESIAN_POINT ( 'NONE',  ( 119.8823610609119754, -3.163656168406935087, -18.89861972220014508 ) ) ;
#13553 = EDGE_LOOP ( 'NONE', ( #44609, #21513, #16228, #5740, #13913 ) ) ;
#13554 = DIRECTION ( 'NONE',  ( 0.000000000000000000, 0.000000000000000000, -1.000000000000000000 ) ) ;
#13555 = CARTESIAN_POINT ( 'NONE',  ( 124.3692356341887830, 2.211163780387002564, -9.774729780252799927 ) ) ;
#13556 = CARTESIAN_POINT ( 'NONE',  ( 113.9552233795247815, -8.938348069036489818, -17.46756447353520159 ) ) ;
#13557 = VECTOR ( 'NONE', #31459, 1000.000000000000000 ) ;
#13558 = CARTESIAN_POINT ( 'NONE',  ( 118.0596094832010579, -2.324775150319241757, -18.02356106541842706 ) ) ;
#13559 = CARTESIAN_POINT ( 'NONE',  ( 124.8223148109119762, -10.15424416112533912, -14.75197769757731336 ) ) ;
#13560 = CARTESIAN_POINT ( 'NONE',  ( 113.9875214775786532, -8.899110576539710493, -16.42337572283490132 ) ) ;
#13561 = CARTESIAN_POINT ( 'NONE',  ( 126.3183919423436805, -5.950396648433367019, -18.32522280981617513 ) ) ;
#13562 = ORIENTED_EDGE ( 'NONE', *, *, #14431, .T. ) ;
#13563 = CARTESIAN_POINT ( 'NONE',  ( 86.09323753712084226, -25.38011337280982715, -14.88121679464376257 ) ) ;
#13564 = CARTESIAN_POINT ( 'NONE',  ( 112.2289948109119848, -7.643976991954077427, -18.09477374809248928 ) ) ;
#13565 = CARTESIAN_POINT ( 'NONE',  ( 112.1874712410415924, 0.7607806665037644134, -12.14321520033829493 ) ) ;
#13566 = CARTESIAN_POINT ( 'NONE',  ( 74.82520252044861309, -48.51951888521425360, -10.39321520033831625 ) ) ;
#13568 = CARTESIAN_POINT ( 'NONE',  ( 125.2761281442453054, -10.63000616557722466, -14.87417383870573495 ) ) ;
#13567 = CARTESIAN_POINT ( 'NONE',  ( 64.93843452746739331, -36.87240490544534310, -5.472084168854524755 ) ) ;
#13569 = AXIS2_PLACEMENT_3D ( 'NONE', #25359, #38794, #15089 ) ;
#13570 = CARTESIAN_POINT ( 'NONE',  ( 125.3328548109119964, -0.8288870151387760510, -10.36305467784173118 ) ) ;
#13571 = VERTEX_POINT ( 'NONE', #43516 ) ;
#13572 = CARTESIAN_POINT ( 'NONE',  ( 112.4559014775786494, -9.988377603198976828, -10.36322818467138340 ) ) ;
#13573 = CARTESIAN_POINT ( 'NONE',  ( 71.37572422742091760, -11.86958442233774313, -21.89321520033831447 ) ) ;
#13574 = CARTESIAN_POINT ( 'NONE',  ( 115.5526452545247622, 0.8980012041604421569, -11.00651665394454071 ) ) ;
#13575 = CARTESIAN_POINT ( 'NONE',  ( 125.7299414775786346, -10.15424416112533912, -14.75197769757731336 ) ) ;
#13576 = CARTESIAN_POINT ( 'NONE',  ( 123.4041481442452834, 0.1319031606808879209, -14.10382304977623669 ) ) ;
#13577 = CARTESIAN_POINT ( 'NONE',  ( 70.19189222814998175, -100.0979043305785581, -53.24182196210380624 ) ) ;
#13578 = CARTESIAN_POINT ( 'NONE',  ( 108.8851452545248151, -9.868328341294098749, -15.46607636864997204 ) ) ;
#13579 = AXIS2_PLACEMENT_3D ( 'NONE', #10866, #28642, #20907 ) ;
#13580 = CARTESIAN_POINT ( 'NONE',  ( 117.2294421295247844, -4.863998795839590272, -13.39321520033831447 ) ) ;
#13581 = CARTESIAN_POINT ( 'NONE',  ( 112.3308181469516995, -3.929494816604734098, -18.62311481910882804 ) ) ;
#13582 = CARTESIAN_POINT ( 'NONE',  ( 112.6828081442453282, -2.084020599724406786, -8.691656652584148546 ) ) ;
#13583 = CARTESIAN_POINT ( 'NONE',  ( 78.93021946355167984, -3.662536865724447921, -19.39321520033831447 ) ) ;
#13584 = CARTESIAN_POINT ( 'NONE',  ( 117.7882081442453170, -6.344957434206651037, -7.627207830600339911 ) ) ;
#13585 = CARTESIAN_POINT ( 'NONE',  ( 110.3436608795247764, -8.938348069036489818, -9.318865927141430916 ) ) ;
#13586 = CARTESIAN_POINT ( 'NONE',  ( 90.04708369096697140, -25.79823837677164988, -13.86919086559751157 ) ) ;
#13587 = CARTESIAN_POINT ( 'NONE',  ( 111.9453614775786434, -7.894159318335828068, -9.358103419637847864 ) ) ;
#13588 = CARTESIAN_POINT ( 'NONE',  ( 69.36136150295220659, -62.97255475958395010, -35.28700389749673860 ) ) ;
#13589 = CARTESIAN_POINT ( 'NONE',  ( 121.0783548109119749, 0.2603800115204892296, -16.42320221600525088 ) ) ;
#13590 = CARTESIAN_POINT ( 'NONE',  ( 116.6536748109119941, 0.9020085738987339008, -11.91225656197089222 ) ) ;
#13591 = ORIENTED_EDGE ( 'NONE', *, *, #5573, .F. ) ;
#13592 = CARTESIAN_POINT ( 'NONE',  ( 113.5904348109119866, -2.084020599724406786, -8.691656652584148546 ) ) ;
#13593 = TOROIDAL_SURFACE ( 'NONE', #44185, 5.952500000000000568, 0.9525000000000000133 ) ;
#13594 = CARTESIAN_POINT ( 'NONE',  ( 111.3213681442453264, -7.643976991954077427, -18.09477374809248928 ) ) ;
#13595 = CARTESIAN_POINT ( 'NONE',  ( 122.6667014775786413, -7.893985811506177619, -18.51759400769804742 ) ) ;
#13596 = CARTESIAN_POINT ( 'NONE',  ( 115.0653281442453277, -6.344957434206662583, -7.627207830600332805 ) ) ;
#13597 = CARTESIAN_POINT ( 'NONE',  ( 115.2355081442453155, 0.1319031606808879209, -14.10382304977623669 ) ) ;
#13598 = ORIENTED_EDGE ( 'NONE', *, *, #19193, .T. ) ;
#13599 = CARTESIAN_POINT ( 'NONE',  ( 115.9162281442453093, -5.574606645277164318, -18.38911715685844683 ) ) ;
#13600 = CARTESIAN_POINT ( 'NONE',  ( 117.5613014775786525, 0.9020085738987339008, -11.91225656197089222 ) ) ;
#13601 = CARTESIAN_POINT ( 'NONE',  ( 123.6877814775786533, -6.222761293078241884, -8.102969835052219238 ) ) ;
#13602 = CARTESIAN_POINT ( 'NONE',  ( 116.8348670993032528, -1.227467558651016644, -17.16727754148226026 ) ) ;
#13603 = AXIS2_PLACEMENT_3D ( 'NONE', #34199, #41303, #19860 ) ;
#13604 = CARTESIAN_POINT ( 'NONE',  ( 114.5108483795247878, -0.7896495226426338832, -9.318865927141430916 ) ) ;
#13605 = VERTEX_POINT ( 'NONE', #12285 ) ;
#13606 = DIRECTION ( 'NONE',  ( 0.000000000000000000, 0.000000000000000000, -1.000000000000000000 ) ) ;
#13607 = CARTESIAN_POINT ( 'NONE',  ( 113.0293531537514866, 0.4930828106260651267, -14.64321520033833579 ) ) ;
#13608 = EDGE_CURVE ( 'NONE', #4544, #18037, #36484, .T. ) ;
#13609 = VECTOR ( 'NONE', #30403, 1000.000000000000114 ) ;
#13610 = DIRECTION ( 'NONE',  ( 0.000000000000000000, -0.3818493186865936084, 0.9242245927363024194 ) ) ;
#13611 = CARTESIAN_POINT ( 'NONE',  ( 112.5126281442453120, -10.30919188438810075, -12.61870101168855918 ) ) ;
#13612 = CARTESIAN_POINT ( 'NONE',  ( 112.8529881442453302, -7.894159318335828068, -9.358103419637847864 ) ) ;
#13613 = ADVANCED_FACE ( 'NONE', ( #5642 ), #32997, .T. ) ;
#13614 = CARTESIAN_POINT ( 'NONE',  ( 107.0793640045248196, 0.1403307496149616695, -15.46607636864997204 ) ) ;
#13615 = CARTESIAN_POINT ( 'NONE',  ( 77.77634386988383142, 3.254514819260860392, -21.89321520033831447 ) ) ;
#13616 = CARTESIAN_POINT ( 'NONE',  ( 119.6601881442453106, -8.166667518702819706, -8.995218007635861213 ) ) ;
#13617 = CARTESIAN_POINT ( 'NONE',  ( 137.3216041022093066, -6.332459753521784585, -18.38014592818993620 ) ) ;
#13618 = EDGE_CURVE ( 'NONE', #32081, #15763, #34712, .T. ) ;
#13619 = CARTESIAN_POINT ( 'NONE',  ( 115.9017791257774803, 0.2334052082820642360, -12.14321520033831625 ) ) ;
#13620 = DIRECTION ( 'NONE',  ( -0.000000000000000000, -0.9284778069183721172, -0.3713878862591650232 ) ) ;
#13621 = CARTESIAN_POINT ( 'NONE',  ( 121.9292548109119849, -7.894159318335828068, -9.358103419637847864 ) ) ;
#13622 = ORIENTED_EDGE ( 'NONE', *, *, #27842, .T. ) ;
#13623 = CARTESIAN_POINT ( 'NONE',  ( 125.4463081442452932, -5.638512984488999180, -18.83840828888717311 ) ) ;
#13624 = CARTESIAN_POINT ( 'NONE',  ( 120.0005481442453146, -5.638512984488999180, -18.83840828888717311 ) ) ;
#13625 = CARTESIAN_POINT ( 'NONE',  ( 125.7866681442452688, -0.4660016031367893996, -10.09054647747474043 ) ) ;
#13626 = CARTESIAN_POINT ( 'NONE',  ( 114.3278814775786429, 0.1319031606808879209, -14.10382304977623669 ) ) ;
#13627 = EDGE_CURVE ( 'NONE', #40326, #511, #34277, .T. ) ;
#13628 = CARTESIAN_POINT ( 'NONE',  ( 112.3991748109119868, -1.833838273342658809, -17.42832698103878286 ) ) ;
#13629 = CARTESIAN_POINT ( 'NONE',  ( 109.5102233795247884, -8.938348069036489818, -17.46756447353520159 ) ) ;
#13630 = DIRECTION ( 'NONE',  ( -0.9908103287288504424, 0.1352586133457950035, 0.000000000000000000 ) ) ;
#13631 = CARTESIAN_POINT ( 'NONE',  ( 115.1359265045248605, -7.250697342233347165, -19.15521520033831138 ) ) ;
#13632 = CARTESIAN_POINT ( 'NONE',  ( 116.0864081442453113, -0.1624402480850797581, -16.17319339645315424 ) ) ;
#13633 = CARTESIAN_POINT ( 'NONE',  ( 120.4543614775786295, -5.574606645277164318, -18.38911715685844683 ) ) ;
#13634 = CARTESIAN_POINT ( 'NONE',  ( 89.33740294208338639, -9.098375579515472822, -18.64321520033831803 ) ) ;
#13635 = CARTESIAN_POINT ( 'NONE',  ( 122.3132204359119868, 1.345710702986147034, -13.97328579221134426 ) ) ;
#13636 = TOROIDAL_SURFACE ( 'NONE', #15092, 3.250000000000000000, 0.2500000000000000000 ) ;
#13637 = CARTESIAN_POINT ( 'NONE',  ( 108.9545983795247821, -8.402594152722688392, -16.93181055722141792 ) ) ;
#13638 = EDGE_CURVE ( 'NONE', #20846, #39210, #33540, .T. ) ;
#13639 = CARTESIAN_POINT ( 'NONE',  ( 78.69189222814998175, -49.76310523276723785, -40.89321520033831092 ) ) ;
#13640 = CARTESIAN_POINT ( 'NONE',  ( 113.3635281442453504, -9.988377603198976828, -10.36322818467138340 ) ) ;
#13641 = CARTESIAN_POINT ( 'NONE',  ( 115.4624148109119943, -5.638512984488999180, -18.83840828888717311 ) ) ;
#13642 = CARTESIAN_POINT ( 'NONE',  ( 121.4103298109119748, -7.200787124940443817, -17.81845355600750835 ) ) ;
#13643 = CARTESIAN_POINT ( 'NONE',  ( 121.3408766859119794, -9.033780868592240054, -16.85052413769862056 ) ) ;
#13644 = EDGE_CURVE ( 'NONE', #11630, #32081, #45078, .T. ) ;
#13645 = EDGE_CURVE ( 'NONE', #38363, #8089, #785, .T. ) ;
#13646 = ORIENTED_EDGE ( 'NONE', *, *, #18171, .F. ) ;
#13647 = CARTESIAN_POINT ( 'NONE',  ( 87.44708369096657918, -25.99489077589583630, -8.393215200338314474 ) ) ;
#13648 = CIRCLE ( 'NONE', #44962, 1.499999999999998002 ) ;
#13649 = EDGE_LOOP ( 'NONE', ( #13814, #28515, #13097, #18301, #21573 ) ) ;
#13650 = CARTESIAN_POINT ( 'NONE',  ( 120.6812681442452941, -10.30919188438810075, -12.61870101168855918 ) ) ;
#13651 = CARTESIAN_POINT ( 'NONE',  ( 113.7038881442453402, -3.383040157471821630, -19.15922257007629170 ) ) ;
#13652 = CARTESIAN_POINT ( 'NONE',  ( 119.3765548109119834, -10.15424416112533912, -14.75197769757731336 ) ) ;
#13653 = LINE ( 'NONE', #34376, #25721 ) ;
#13654 = CARTESIAN_POINT ( 'NONE',  ( 120.1707281442453166, 0.2603800115204892296, -16.42320221600525088 ) ) ;
#13655 = CARTESIAN_POINT ( 'NONE',  ( 116.4267681442453153, -3.383040157471821630, -19.15922257007629170 ) ) ;
#13656 = CARTESIAN_POINT ( 'NONE',  ( 108.4684265045247997, -2.791137627527939813, -8.388885654883777576 ) ) ;
#13657 = CARTESIAN_POINT ( 'NONE',  ( 111.7751814775786556, -2.084020599724406786, -8.691656652584148546 ) ) ;
#13658 = CARTESIAN_POINT ( 'NONE',  ( 116.5944421295247793, -0.02276961308034231024, -12.14321520033831625 ) ) ;
#13659 = ORIENTED_EDGE ( 'NONE', *, *, #34764, .T. ) ;
#13660 =( BOUNDED_CURVE ( )  B_SPLINE_CURVE ( 2, ( #32726, #19514, #1281, #1499, #15420, #29325, #43239, #12004, #34087, #44824, #23391, #19737, #20427, #40721, #12684, #16785, #26582 ),
 .UNSPECIFIED., .F., .T. ) 
 B_SPLINE_CURVE_WITH_KNOTS ( ( 3, 2, 2, 2, 2, 2, 2, 2, 3 ),
 ( 0.07962824165685890299, 0.08593750000000000000, 0.09375000000000000000, 0.1015625000000000000, 0.1093750000000000000, 0.1171875000000000000, 0.1250000000000000000, 0.1328125000000000000, 0.1391217583431412219 ),
 .UNSPECIFIED. ) 
 CURVE ( )  GEOMETRIC_REPRESENTATION_ITEM ( )  RATIONAL_B_SPLINE_CURVE ( ( 0.9763430640195970289, 0.9385262470928680267, 1.000000000000000000, 0.9238795325112869605, 1.000000000000000000, 0.9238795325112869605, 1.000000000000000000, 0.9238795325112869605, 1.000000000000000000, 0.9238795325112869605, 1.000000000000000000, 0.9238795325112869605, 1.000000000000000000, 0.9238795325112869605, 1.000000000000000000, 0.9385262470928680267, 0.9763430640195970289 ) ) 
 REPRESENTATION_ITEM ( '' )  );
#13661 = CARTESIAN_POINT ( 'NONE',  ( 118.5256548109119876, -0.4660016031367893996, -10.09054647747474043 ) ) ;
#13662 = DIRECTION ( 'NONE',  ( 1.000000000000000000, 0.000000000000000000, -0.000000000000000000 ) ) ;
#13663 = CARTESIAN_POINT ( 'NONE',  ( 114.9518748109119883, -1.834011780172310813, -8.268836392978581529 ) ) ;
#13664 = ORIENTED_EDGE ( 'NONE', *, *, #22270, .T. ) ;
#13665 = CARTESIAN_POINT ( 'NONE',  ( 114.8581140045248361, -10.62599879583958717, -11.00651665394454604 ) ) ;
#13666 = CARTESIAN_POINT ( 'NONE',  ( 124.2550481442452792, -9.988377603198980381, -10.36322818467138518 ) ) ;
#13668 = CARTESIAN_POINT ( 'NONE',  ( 70.19189222814998175, -100.0979043305785581, -53.24182196210380624 ) ) ;
#13667 = CIRCLE ( 'NONE', #22404, 1.500000000000001332 ) ;
#13669 = CARTESIAN_POINT ( 'NONE',  ( 112.1722681442453222, -8.899110576539710493, -16.42337572283490132 ) ) ;
#13670 = CARTESIAN_POINT ( 'NONE',  ( 78.01305443124351768, -57.59686644005601863, -1.019253850192035404 ) ) ;
#13671 = CARTESIAN_POINT ( 'NONE',  ( 117.3911214775786505, -7.894159318335828068, -9.358103419637847864 ) ) ;
#13672 = DIRECTION ( 'NONE',  ( 0.9908103287288504424, -0.1352586133457951700, 0.000000000000000000 ) ) ;
#13673 = CARTESIAN_POINT ( 'NONE',  ( 118.5823814775786360, -7.643976991954077427, -18.09477374809248928 ) ) ;
#13674 = CARTESIAN_POINT ( 'NONE',  ( 105.7294421295247844, -9.051693226400931991, -21.89321520033831447 ) ) ;
#13675 = B_SPLINE_CURVE_WITH_KNOTS ( 'NONE', 3,
 ( #40275, #19525, #16107, #6292 ),
 .UNSPECIFIED., .F., .F.,
 ( 4, 4 ),
 ( 0.0006421114935806760109, 0.0009604418836934789901 ),
 .UNSPECIFIED. ) ;
#13676 = CARTESIAN_POINT ( 'NONE',  ( 114.1577014775786552, -3.505236298600246325, -18.68346056562440793 ) ) ;
#13677 = CARTESIAN_POINT ( 'NONE',  ( 120.5074391859119913, -8.844754642576884152, -8.592115655440050404 ) ) ;
#13678 = CARTESIAN_POINT ( 'NONE',  ( 114.7249681442453237, 0.2603800115204892296, -16.42320221600525088 ) ) ;
#13679 = CARTESIAN_POINT ( 'NONE',  ( 126.1837548109119211, -10.63000616557722466, -14.87417383870573495 ) ) ;
#13680 = CIRCLE ( 'NONE', #41372, 5.132259260909280307 ) ;
#13681 = CARTESIAN_POINT ( 'NONE',  ( 118.6391081442452986, -5.574606645277164318, -18.38911715685844683 ) ) ;
#13682 = ORIENTED_EDGE ( 'NONE', *, *, #43991, .T. ) ;
#13683 = CARTESIAN_POINT ( 'NONE',  ( 118.0718414775786300, -9.261995988541697145, -16.69588392320189030 ) ) ;
#13684 = EDGE_CURVE ( 'NONE', #43772, #11695, #40231, .T. ) ;
#13685 = CARTESIAN_POINT ( 'NONE',  ( 107.4960827545248350, -2.477300249445798297, -19.15521520033831138 ) ) ;
#13686 = CARTESIAN_POINT ( 'NONE',  ( 87.41631446019775353, -25.38011337280982715, -14.88121679464376257 ) ) ;
#13687 = CARTESIAN_POINT ( 'NONE',  ( 106.5931921295248372, -9.868328341294093420, -13.39321520033831447 ) ) ;
#13688 = CARTESIAN_POINT ( 'NONE',  ( 69.69189222814998175, -41.76310523276723785, -47.71602681600972318 ) ) ;
#13689 = CARTESIAN_POINT ( 'NONE',  ( 122.4397948109119767, -9.988377603198976828, -10.36322818467138340 ) ) ;
#13690 = ORIENTED_EDGE ( 'NONE', *, *, #4405, .T. ) ;
#13691 = CARTESIAN_POINT ( 'NONE',  ( 70.19189222814998175, -65.04786711941002864, -39.22192925581976652 ) ) ;
#13692 = CARTESIAN_POINT ( 'NONE',  ( 119.8303681442453126, 0.4262465694468514643, -12.03445270309931736 ) ) ;
#13693 = CARTESIAN_POINT ( 'NONE',  ( 123.5633766859119618, -0.06289925094098414160, -9.412459353600670653 ) ) ;
#13694 = ADVANCED_FACE ( 'NONE', ( #2905 ), #38934, .T. ) ;
#13695 = CARTESIAN_POINT ( 'NONE',  ( 124.0848681442452772, -4.089484607189486809, -7.948022111789456723 ) ) ;
#13696 = CARTESIAN_POINT ( 'NONE',  ( 115.5526452545247622, -9.868328341294098749, -15.46607636864997204 ) ) ;
#13697 = LINE ( 'NONE', #3423, #17022 ) ;
#13698 = VERTEX_POINT ( 'NONE', #14689 ) ;
#13699 = CARTESIAN_POINT ( 'NONE',  ( 112.0588148109119828, 0.5811942927096154232, -14.16772938898807155 ) ) ;
#13700 = CARTESIAN_POINT ( 'NONE',  ( 126.6375681442452930, -10.15424416112533912, -14.75197769757731336 ) ) ;
#13701 = CARTESIAN_POINT ( 'NONE',  ( 123.9714148109119805, -0.4660016031367893996, -10.09054647747474043 ) ) ;
#13702 = AXIS2_PLACEMENT_3D ( 'NONE', #6325, #41225, #44642 ) ;
#13703 = CARTESIAN_POINT ( 'NONE',  ( 117.5613014775786525, -10.15424416112533912, -14.75197769757731336 ) ) ;
#13704 = CARTESIAN_POINT ( 'NONE',  ( 82.57348731610973402, -31.56754274340543986, -22.29195438618578606 ) ) ;
#13705 = CARTESIAN_POINT ( 'NONE',  ( 118.4689281442453392, 0.9020085738987339008, -11.91225656197089222 ) ) ;
#13706 = CARTESIAN_POINT ( 'NONE',  ( 41.72636039845269096, -11.37347657059392070, -19.39321520033831447 ) ) ;
#13707 = ADVANCED_FACE ( 'NONE', ( #22201 ), #21911, .T. ) ;
#13708 = CARTESIAN_POINT ( 'NONE',  ( 123.0637881442452937, -8.899110576539710493, -16.42337572283490132 ) ) ;
#13709 = ORIENTED_EDGE ( 'NONE', *, *, #8890, .F. ) ;
#13710 = LINE ( 'NONE', #3434, #24910 ) ;
#13711 = CARTESIAN_POINT ( 'NONE',  ( 115.9729548109119861, -6.344957434206662583, -7.627207830600332805 ) ) ;
#13712 = CARTESIAN_POINT ( 'NONE',  ( 125.4463081442452932, -4.153390946401325223, -8.397313243818185668 ) ) ;
#13713 = ORIENTED_EDGE ( 'NONE', *, *, #22220, .F. ) ;
#13714 = CARTESIAN_POINT ( 'NONE',  ( 122.3132204359119868, 1.345710702986147034, -13.97328579221134426 ) ) ;
#13715 = CARTESIAN_POINT ( 'NONE',  ( 61.25533248984433499, -12.48000644236081058, -9.603275126499889680 ) ) ;
#13716 = CARTESIAN_POINT ( 'NONE',  ( 121.1918081442452859, 0.9020085738987339008, -11.91225656197089222 ) ) ;
#13717 = CARTESIAN_POINT ( 'NONE',  ( 109.2324108795247923, -8.938348069036489818, -9.318865927141430916 ) ) ;
#13718 = CARTESIAN_POINT ( 'NONE',  ( 118.8092881442453290, -0.1624402480850797581, -16.17319339645315424 ) ) ;
#13719 = ORIENTED_EDGE ( 'NONE', *, *, #32534, .T. ) ;
#13720 = ORIENTED_EDGE ( 'NONE', *, *, #32799, .T. ) ;
#13721 = CARTESIAN_POINT ( 'NONE',  ( 112.7395348109119766, -5.638512984488999180, -18.83840828888717311 ) ) ;
#13722 = CARTESIAN_POINT ( 'NONE',  ( 123.4041481442452834, 0.1319031606808879209, -14.10382304977623669 ) ) ;
#13723 = APPLICATION_CONTEXT ( 'automotive_design' ) ;
#13724 = DIRECTION ( 'NONE',  ( 1.000000000000000000, 0.000000000000000000, -0.000000000000000000 ) ) ;
#13725 = CARTESIAN_POINT ( 'NONE',  ( 59.39246203831174853, -12.83800168394059682, -17.39321520033831447 ) ) ;
#13726 = CARTESIAN_POINT ( 'NONE',  ( 121.7590748109119687, -7.893985811506177619, -18.51759400769804742 ) ) ;
#13727 = CARTESIAN_POINT ( 'NONE',  ( 109.2620651800721845, 0.07459198820006229802, -14.64321520033832691 ) ) ;
#13728 = DIRECTION ( 'NONE',  ( -1.000000000000000000, 0.000000000000000000, 0.000000000000000000 ) ) ;
#13729 = CARTESIAN_POINT ( 'NONE',  ( 118.8660148109119774, -10.30919188438810075, -12.61870101168855918 ) ) ;
#13731 = CARTESIAN_POINT ( 'NONE',  ( 120.0005481442453146, -4.153390946401325223, -8.397313243818185668 ) ) ;
#13730 = CARTESIAN_POINT ( 'NONE',  ( 119.3198281442452924, 0.5811942927096110934, -14.16772938898807510 ) ) ;
#13732 = DIRECTION ( 'NONE',  ( 0.000000000000000000, 0.000000000000000000, 1.000000000000000000 ) ) ;
#13733 = CARTESIAN_POINT ( 'NONE',  ( 114.6115148109119986, -3.383040157471821630, -19.15922257007629170 ) ) ;
#13734 = ORIENTED_EDGE ( 'NONE', *, *, #469, .T. ) ;
#13735 = ADVANCED_FACE ( 'NONE', ( #25407 ), #39079, .T. ) ;
#13736 = CARTESIAN_POINT ( 'NONE',  ( 126.1270281442452870, 0.1319031606808879209, -14.10382304977623669 ) ) ;
#13737 = CARTESIAN_POINT ( 'NONE',  ( 125.4463081442453500, -4.153390946402302220, -8.397313243818043560 ) ) ;
#13738 = CARTESIAN_POINT ( 'NONE',  ( 109.3018640045248304, -10.62599879583958717, -11.00651665394454604 ) ) ;
#13739 = CARTESIAN_POINT ( 'NONE',  ( 110.2047546295247855, -4.863998795839590272, -18.39754474579285315 ) ) ;
#13740 = CARTESIAN_POINT ( 'NONE',  ( 105.9681140045248355, -10.62599879583958717, -11.00651665394454604 ) ) ;
#13741 = CARTESIAN_POINT ( 'NONE',  ( 122.3263414775786373, -6.344957434206665248, -7.627207830600338134 ) ) ;
#13742 = CARTESIAN_POINT ( 'NONE',  ( 126.5808414775786446, -9.859900752359378018, -12.68260735090039759 ) ) ;
#13743 =( BOUNDED_CURVE ( )  B_SPLINE_CURVE ( 2, ( #12037, #1311, #43497, #15223, #22510, #12266, #22731, #9742, #40526, #5848, #13611, #33652, #30255, #20679, #40990, #44181, #44401 ),
 .UNSPECIFIED., .F., .T. ) 
 B_SPLINE_CURVE_WITH_KNOTS ( ( 3, 2, 2, 2, 2, 2, 2, 2, 3 ),
 ( 0.01700466748089215011, 0.02343750000000000000, 0.03125000000000000000, 0.03906250000000000000, 0.04687500000000000000, 0.05468750000000000000, 0.06250000000000000000, 0.07031250000000000000, 0.07674533251905850395 ),
 .UNSPECIFIED. ) 
 CURVE ( )  GEOMETRIC_REPRESENTATION_ITEM ( )  RATIONAL_B_SPLINE_CURVE ( ( 0.9778625265006459788, 0.9373222120152210346, 1.000000000000000000, 0.9238795325112869605, 1.000000000000000000, 0.9238795325112869605, 1.000000000000000000, 0.9238795325112869605, 1.000000000000000000, 0.9238795325112869605, 1.000000000000000000, 0.9238795325112869605, 1.000000000000000000, 0.9238795325112869605, 1.000000000000000000, 0.9373222120157009840, 0.9778625265000240319 ) ) 
 REPRESENTATION_ITEM ( '' )  );
#13744 = ORIENTED_EDGE ( 'NONE', *, *, #39832, .F. ) ;
#13745 = CARTESIAN_POINT ( 'NONE',  ( 126.0703014775786102, -9.988377603198980381, -10.36322818467138518 ) ) ;
#13746 = CARTESIAN_POINT ( 'NONE',  ( 110.4131140045248287, -10.62599879583958717, -11.00651665394454604 ) ) ;
#13747 = CARTESIAN_POINT ( 'NONE',  ( 59.78685257969306122, -14.81377569729345822, -19.38480234211904119 ) ) ;
#13748 = CARTESIAN_POINT ( 'NONE',  ( 125.2761281442453054, -10.63000616557722466, -14.87417383870573495 ) ) ;
#13749 = CARTESIAN_POINT ( 'NONE',  ( 125.6164881442453094, 0.2603800115204892296, -16.42320221600525088 ) ) ;
#13750 = CARTESIAN_POINT ( 'NONE',  ( 120.0875454359120056, -10.25250061710389282, -12.88985647778275911 ) ) ;
#13751 = CARTESIAN_POINT ( 'NONE',  ( 125.9001214775786224, -5.574606645277164318, -18.38911715685844683 ) ) ;
#13752 = CARTESIAN_POINT ( 'NONE',  ( 111.8862721015961483, -1.040089454026968951, -17.23633227186634187 ) ) ;
#13753 = CARTESIAN_POINT ( 'NONE',  ( 105.9681140045248355, -10.62599879583958717, -11.00651665394454604 ) ) ;
#13754 = ORIENTED_EDGE ( 'NONE', *, *, #8059, .F. ) ;
#13755 = DIRECTION ( 'NONE',  ( -1.000000000000000000, 1.040834085586084059E-15, 0.000000000000000000 ) ) ;
#13756 = CARTESIAN_POINT ( 'NONE',  ( 114.2144281442453178, -1.833838273342658809, -17.42832698103878286 ) ) ;
#13757 = CARTESIAN_POINT ( 'NONE',  ( 113.3635281442453504, -9.988377603198976828, -10.36322818467138340 ) ) ;
#13758 = EDGE_CURVE ( 'NONE', #10099, #37706, #32229, .T. ) ;
#13759 = CARTESIAN_POINT ( 'NONE',  ( 109.1629577545248395, -2.791137627527939813, -18.39754474579286025 ) ) ;
#13760 = CARTESIAN_POINT ( 'NONE',  ( 108.6073327545248048, -6.936859964151250502, -8.388885654883777576 ) ) ;
#13761 = CARTESIAN_POINT ( 'NONE',  ( 123.3474214775786209, -0.1624402480850797581, -16.17319339645315424 ) ) ;
#13762 = CARTESIAN_POINT ( 'NONE',  ( 115.0653281442453277, -3.505236298600246325, -18.68346056562440793 ) ) ;
#13763 = CARTESIAN_POINT ( 'NONE',  ( 112.3424481442453384, -3.505236298600246325, -18.68346056562440793 ) ) ;
#13764 = VERTEX_POINT ( 'NONE', #28827 ) ;
#13765 = CARTESIAN_POINT ( 'NONE',  ( 120.4379860609119675, -3.387241619883791355, -18.17469012370385073 ) ) ;
#13766 = CARTESIAN_POINT ( 'NONE',  ( 119.7736414775786358, -10.30919188438810075, -12.61870101168855918 ) ) ;
#13767 = CARTESIAN_POINT ( 'NONE',  ( 115.9294421295247872, 1.035107641088057973, -4.893215200338314474 ) ) ;
#13768 = CARTESIAN_POINT ( 'NONE',  ( 112.5693548109119888, 0.4262465694468514643, -12.03445270309931736 ) ) ;
#13769 = EDGE_LOOP ( 'NONE', ( #26499, #44506, #39321, #12219 ) ) ;
#13770 = FACE_OUTER_BOUND ( 'NONE', #32659, .T. ) ;
#13771 = ORIENTED_EDGE ( 'NONE', *, *, #16530, .T. ) ;
#13772 = CARTESIAN_POINT ( 'NONE',  ( 118.1852948109119836, -4.153390946401325223, -8.397313243818185668 ) ) ;
#13773 = CARTESIAN_POINT ( 'NONE',  ( 115.5191414775786569, -6.222761293078241884, -8.102969835052219238 ) ) ;
#13774 = CARTESIAN_POINT ( 'NONE',  ( 151.2860562277021472, -4.863998795839242995, -13.39321520033831447 ) ) ;
#13775 = CARTESIAN_POINT ( 'NONE',  ( 120.5074391859119913, -8.844754642576884152, -8.592115655440050404 ) ) ;
#13776 = ORIENTED_EDGE ( 'NONE', *, *, #6315, .F. ) ;
#13777 = DIRECTION ( 'NONE',  ( -2.312964634635740689E-15, 0.000000000000000000, 1.000000000000000000 ) ) ;
#13778 = CARTESIAN_POINT ( 'NONE',  ( 125.2512653913870082, 2.257127252030525000, -11.96997911676347393 ) ) ;
#13779 = CARTESIAN_POINT ( 'NONE',  ( 114.0941296295247867, -4.863998795839590272, -19.15521520033831493 ) ) ;
#13780 = CARTESIAN_POINT ( 'NONE',  ( 117.8239502440515452, -2.467220198592778413, -17.83387418641524391 ) ) ;
#13781 = CARTESIAN_POINT ( 'NONE',  ( 121.6456214775786293, 0.4262465694468514643, -12.03445270309931736 ) ) ;
#13782 = CARTESIAN_POINT ( 'NONE',  ( 117.6747548109119919, -7.643976991954077427, -18.09477374809248928 ) ) ;
#13783 = CARTESIAN_POINT ( 'NONE',  ( 120.0940564575754905, -1.016270020561755860, -17.26805140881366896 ) ) ;
#13784 = VERTEX_POINT ( 'NONE', #11503 ) ;
#13785 = DIRECTION ( 'NONE',  ( -1.000000000000000000, 0.000000000000000000, 0.000000000000000000 ) ) ;
#13786 = CARTESIAN_POINT ( 'NONE',  ( 117.5045748109119756, -9.859900752359374465, -12.68260735090039404 ) ) ;
#13787 = CARTESIAN_POINT ( 'NONE',  ( 86.51169734173754478, -25.99489077589583630, -8.393215200338314474 ) ) ;
#13789 = DIRECTION ( 'NONE',  ( 0.7871354856660167654, -0.6167752151498625546, -0.002461946824136807422 ) ) ;
#13788 = DIRECTION ( 'NONE',  ( 1.000000000000000000, 0.000000000000000000, -0.000000000000000000 ) ) ;
#13790 = VECTOR ( 'NONE', #33182, 1000.000000000000000 ) ;
#13791 = CARTESIAN_POINT ( 'NONE',  ( 125.8433948109119456, -7.643976991954077427, -18.09477374809248928 ) ) ;
#13792 = ORIENTED_EDGE ( 'NONE', *, *, #42112, .T. ) ;
#13793 = CARTESIAN_POINT ( 'NONE',  ( 113.5337081442453240, -9.261995988541697145, -16.69588392320189030 ) ) ;
#13794 = AXIS2_PLACEMENT_3D ( 'NONE', #20364, #36981, #44085 ) ;
#13795 = CARTESIAN_POINT ( 'NONE',  ( 75.14134903615895666, -42.50702760616825771, -15.89321520033831447 ) ) ;
#13796 = CARTESIAN_POINT ( 'NONE',  ( 116.5944421295247793, 0.8980012041604618078, -13.39321520033831447 ) ) ;
#13797 = CARTESIAN_POINT ( 'NONE',  ( 112.5693548109119888, -10.63000616557722466, -14.87417383870573495 ) ) ;
#13798 = CARTESIAN_POINT ( 'NONE',  ( 115.5191414775786569, -3.383040157471821630, -19.15922257007629170 ) ) ;
#13799 = CARTESIAN_POINT ( 'NONE',  ( 122.6667014775786413, -2.084020599724406786, -8.691656652584148546 ) ) ;
#13800 = CARTESIAN_POINT ( 'NONE',  ( 77.44400397045842510, -3.459648945705700473, -10.39321520033831625 ) ) ;
#13801 = CARTESIAN_POINT ( 'NONE',  ( 109.5102233795247884, -1.325403438956436419, -9.854619843455211026 ) ) ;
#13802 = CYLINDRICAL_SURFACE ( 'NONE', #44856, 0.8999999999999980238 ) ;
#13803 = LINE ( 'NONE', #23165, #42738 ) ;
#13804 = CARTESIAN_POINT ( 'NONE',  ( 116.8238548109119819, -5.574606645277164318, -18.38911715685844683 ) ) ;
#13805 = ADVANCED_FACE ( 'NONE', ( #39306 ), #42325, .T. ) ;
#13806 = CARTESIAN_POINT ( 'NONE',  ( 108.3989733795248753, -8.938348069036489818, -17.46756447353520159 ) ) ;
#13807 = CARTESIAN_POINT ( 'NONE',  ( 67.37136766119182596, -67.53150897494617766, -41.09057840265009531 ) ) ;
#13808 = CARTESIAN_POINT ( 'NONE',  ( 110.4825671295247815, -10.62599879583958540, -13.39321520033831447 ) ) ;
#13809 = CARTESIAN_POINT ( 'NONE',  ( 124.8223148109119762, 0.9020085738987339008, -11.91225656197089222 ) ) ;
#13810 = CARTESIAN_POINT ( 'NONE',  ( 112.4559014775786778, -0.1624402480850797581, -16.17319339645315424 ) ) ;
#13811 = LINE ( 'NONE', #16791, #2221 ) ;
#13812 = CARTESIAN_POINT ( 'NONE',  ( 118.7525614775786380, -8.166667518702819706, -8.995218007635861213 ) ) ;
#13813 = CARTESIAN_POINT ( 'NONE',  ( 117.2209414775786485, -7.893985811506177619, -18.51759400769804742 ) ) ;
#13814 = ORIENTED_EDGE ( 'NONE', *, *, #45007, .T. ) ;
#13815 = CARTESIAN_POINT ( 'NONE',  ( 113.8173414775786512, -9.565557343593413364, -10.61323700422348004 ) ) ;
#13816 = CARTESIAN_POINT ( 'NONE',  ( 125.2761281442453054, -10.63000616557722466, -14.87417383870573495 ) ) ;
#13817 = CARTESIAN_POINT ( 'NONE',  ( 112.4559014775786494, -9.988377603198976828, -10.36322818467138340 ) ) ;
#13818 = CARTESIAN_POINT ( 'NONE',  ( 114.8951481442453115, -8.899110576539710493, -16.42337572283490132 ) ) ;
#13819 = ORIENTED_EDGE ( 'NONE', *, *, #22778, .T. ) ;
#13820 = CARTESIAN_POINT ( 'NONE',  ( 120.6245414775786458, -0.1624402480850797581, -16.17319339645315424 ) ) ;
#13821 = CARTESIAN_POINT ( 'NONE',  ( 115.9729548109119861, -6.344957434206662583, -7.627207830600332805 ) ) ;
#13822 = CARTESIAN_POINT ( 'NONE',  ( 114.5803015045248117, -2.477300249445798297, -7.631215200338321125 ) ) ;
#13823 = ORIENTED_EDGE ( 'NONE', *, *, #35289, .T. ) ;
#13824 = CARTESIAN_POINT ( 'NONE',  ( 65.82164714941100669, 4.169909004287361221, -19.39321520033831447 ) ) ;
#13825 = CARTESIAN_POINT ( 'NONE',  ( 55.39394582045726168, -26.25884925591183716, -19.39321520033831447 ) ) ;
#13826 = LINE ( 'NONE', #37767, #36432 ) ;
#13827 = CIRCLE ( 'NONE', #31296, 1.500000000000001332 ) ;
#13828 = CARTESIAN_POINT ( 'NONE',  ( 114.7816948109119863, 0.5811942927096154232, -14.16772938898807155 ) ) ;
#13829 = CARTESIAN_POINT ( 'NONE',  ( 135.5837700375960821, -10.80736548491261750, -14.14713708756795540 ) ) ;
#13830 = CARTESIAN_POINT ( 'NONE',  ( 121.4136688928271184, -8.278628333885235335, -17.13983228602121045 ) ) ;
#13831 = CARTESIAN_POINT ( 'NONE',  ( 62.35177615844777677, -12.50551974594107740, -16.84622691350345036 ) ) ;
#13832 = CARTESIAN_POINT ( 'NONE',  ( 115.4776403923315655, -1.063912429576147511, -17.20460841810472985 ) ) ;
#13833 = CARTESIAN_POINT ( 'NONE',  ( 114.0941296295247867, -4.863998795839590272, -8.388885654883775800 ) ) ;
#13834 = CARTESIAN_POINT ( 'NONE',  ( 119.4900081442453086, -1.834011780172310813, -8.268836392978581529 ) ) ;
#13835 = CARTESIAN_POINT ( 'NONE',  ( 137.0130966147668232, -6.718222664625504770, -18.52177234174325804 ) ) ;
#13836 = DIRECTION ( 'NONE',  ( 0.000000000000000000, 0.000000000000000000, -1.000000000000000000 ) ) ;
#13837 = CARTESIAN_POINT ( 'NONE',  ( 90.06246830635160450, -25.99489077589524300, -13.39321520033831625 ) ) ;
#13838 = CARTESIAN_POINT ( 'NONE',  ( 120.6245414775786458, -0.1624402480850797581, -16.17319339645315424 ) ) ;
#13839 = VERTEX_POINT ( 'NONE', #18785 ) ;
#13840 = CARTESIAN_POINT ( 'NONE',  ( 124.9357681442453014, -1.834011780172310813, -8.268836392978581529 ) ) ;
#13841 = CARTESIAN_POINT ( 'NONE',  ( 120.1707281442453166, 0.2603800115204892296, -16.42320221600525088 ) ) ;
#13842 = CARTESIAN_POINT ( 'NONE',  ( 126.0703014775786102, -9.988377603198980381, -10.36322818467138518 ) ) ;
#13843 = CARTESIAN_POINT ( 'NONE',  ( 116.8805814775786445, -3.505236298600246325, -18.68346056562440793 ) ) ;
#13844 = CARTESIAN_POINT ( 'NONE',  ( 112.2289948109119848, -7.643976991954077427, -18.09477374809248928 ) ) ;
#13845 = CARTESIAN_POINT ( 'NONE',  ( 112.1494421295248003, 0.8980012041604618078, -13.39321520033831447 ) ) ;
#13846 = CARTESIAN_POINT ( 'NONE',  ( 105.9681140045248355, 0.1403307496149616695, -15.46607636864997204 ) ) ;
#13847 = CARTESIAN_POINT ( 'NONE',  ( 112.2188952545247531, 0.8980012041604421569, -11.00651665394454071 ) ) ;
#13848 = CARTESIAN_POINT ( 'NONE',  ( 119.4332814775786318, -8.899110576539710493, -16.42337572283490132 ) ) ;
#13849 = CARTESIAN_POINT ( 'NONE',  ( 121.8725281442453223, -6.222761293078241884, -8.102969835052219238 ) ) ;
#13850 = VECTOR ( 'NONE', #16659, 999.9999999999998863 ) ;
#13851 = FACE_OUTER_BOUND ( 'NONE', #39464, .T. ) ;
#13852 = DIRECTION ( 'NONE',  ( -1.000000000000000000, 0.000000000000000000, 0.000000000000000000 ) ) ;
#13853 = CARTESIAN_POINT ( 'NONE',  ( 107.6349890045248401, -9.868328341294098749, -11.32035403202665869 ) ) ;
#13854 = PLANE ( 'NONE',  #24752 ) ;
#13855 = CARTESIAN_POINT ( 'NONE',  ( 113.0798948109119948, -0.4660016031367893996, -10.09054647747474043 ) ) ;
#13856 = CARTESIAN_POINT ( 'NONE',  ( 114.4980614775786592, -7.893985811506177619, -18.51759400769804742 ) ) ;
#13857 = CARTESIAN_POINT ( 'NONE',  ( 143.3676850761856940, -62.82237896425675672, -47.71602681600972318 ) ) ;
#13858 = EDGE_LOOP ( 'NONE', ( #41512, #20507, #10566, #39269 ) ) ;
#13859 = CARTESIAN_POINT ( 'NONE',  ( 123.4666292975675219, -2.827606292292531798, -14.85598063601935870 ) ) ;
#13860 = EDGE_CURVE ( 'NONE', #25860, #2299, #8054, .T. ) ;
#13861 = VERTEX_POINT ( 'NONE', #241 ) ;
#13862 = CARTESIAN_POINT ( 'NONE',  ( 123.6877814775786533, -3.383040157471821630, -19.15922257007629170 ) ) ;
#13863 = CIRCLE ( 'NONE', #29150, 5.999999999999997335 ) ;
#13864 = CARTESIAN_POINT ( 'NONE',  ( 126.4673881442452910, -7.894159318335828068, -9.358103419637847864 ) ) ;
#13865 = CARTESIAN_POINT ( 'NONE',  ( 119.0361948109119652, -2.084020599724406786, -8.691656652584148546 ) ) ;
#13866 = CIRCLE ( 'NONE', #26986, 2.445500000000004448 ) ;
#13867 = FACE_OUTER_BOUND ( 'NONE', #27920, .T. ) ;
#13868 = CARTESIAN_POINT ( 'NONE',  ( 120.3976348109119812, -1.834011780172310813, -8.268836392978581529 ) ) ;
#13869 = CARTESIAN_POINT ( 'NONE',  ( 118.9227414775786400, -10.63000616557722466, -14.87417383870573495 ) ) ;
#13870 = ADVANCED_FACE ( 'NONE', ( #40839 ), #2244, .T. ) ;
#13871 = CARTESIAN_POINT ( 'NONE',  ( 106.8015515045248378, -6.936859964151250502, -18.39754474579286025 ) ) ;
#13872 = CARTESIAN_POINT ( 'NONE',  ( 111.3780948109119890, -5.574606645277164318, -18.38911715685844683 ) ) ;
#13873 = DIRECTION ( 'NONE',  ( 1.000000000000000000, 0.000000000000000000, -0.000000000000000000 ) ) ;
#13874 = ORIENTED_EDGE ( 'NONE', *, *, #13061, .F. ) ;
#13875 = CARTESIAN_POINT ( 'NONE',  ( 118.8660148109119774, -10.30919188438810075, -12.61870101168855918 ) ) ;
#13876 = CARTESIAN_POINT ( 'NONE',  ( 64.69189222814998175, -41.76310523276723785, -19.39321520033831447 ) ) ;
#13877 = CARTESIAN_POINT ( 'NONE',  ( 114.2144281442453178, -8.166667518702817929, -8.995218007635859436 ) ) ;
#13878 = ORIENTED_EDGE ( 'NONE', *, *, #39558, .F. ) ;
#13879 = CARTESIAN_POINT ( 'NONE',  ( 106.5931921295248372, -9.868328341294093420, -13.39321520033831447 ) ) ;
#13880 = CARTESIAN_POINT ( 'NONE',  ( -13.90346623771332801, -4.337920405660049994, -8.734217232838743072 ) ) ;
#13881 = CONICAL_SURFACE ( 'NONE', #34246, 1.610000000000000986, 0.9599310885968765916 ) ;
#13882 = CARTESIAN_POINT ( 'NONE',  ( 119.8748628165343888, -2.324775150319219108, -18.02356106541841996 ) ) ;
#13883 = CYLINDRICAL_SURFACE ( 'NONE', #727, 5.000000000000006217 ) ;
#13884 = EDGE_CURVE ( 'NONE', #27644, #17793, #38070, .T. ) ;
#13885 = CARTESIAN_POINT ( 'NONE',  ( 125.4584548109119737, -9.722663502801697888, -19.87444018218530317 ) ) ;
#13886 = CARTESIAN_POINT ( 'NONE',  ( 119.6034614775786196, -3.505236298600246325, -18.68346056562440793 ) ) ;
#13887 = ADVANCED_FACE ( 'NONE', ( #20309 ), #5925, .T. ) ;
#13888 = EDGE_CURVE ( 'NONE', #8490, #12590, #21165, .T. ) ;
#13889 = CARTESIAN_POINT ( 'NONE',  ( 120.2513676054816045, -2.287189184988711155, -18.07361239780447448 ) ) ;
#13890 = CARTESIAN_POINT ( 'NONE',  ( 119.2063748109119814, -7.894159318335828068, -9.358103419637847864 ) ) ;
#13891 = VECTOR ( 'NONE', #20205, 1000.000000000000114 ) ;
#13892 = CARTESIAN_POINT ( 'NONE',  ( 96.54708369096698561, -23.81115550238859413, -13.04821483042134389 ) ) ;
#13893 = CARTESIAN_POINT ( 'NONE',  ( 118.6958348109119754, -3.505236298600246325, -18.68346056562440793 ) ) ;
#13894 = AXIS2_PLACEMENT_3D ( 'NONE', #8418, #1117, #12070 ) ;
#13895 = CARTESIAN_POINT ( 'NONE',  ( 123.0772048109119652, -7.554583864224885481, -18.48844787311982785 ) ) ;
#13896 = CARTESIAN_POINT ( 'NONE',  ( 115.2922348109119781, -10.63000616557722466, -14.87417383870573495 ) ) ;
#13897 = CARTESIAN_POINT ( 'NONE',  ( 117.6747548109119919, -7.643976991954077427, -18.09477374809248928 ) ) ;
#13898 = VERTEX_POINT ( 'NONE', #20087 ) ;
#13899 = CARTESIAN_POINT ( 'NONE',  ( 118.5823814775786360, -1.834011780172310813, -8.268836392978581529 ) ) ;
#13900 = CARTESIAN_POINT ( 'NONE',  ( 116.0388171295248014, 0.1403307496149613920, -13.39321520033831447 ) ) ;
#13901 = CARTESIAN_POINT ( 'NONE',  ( 115.5758681442453053, -7.894159318335810305, -9.358103419637833653 ) ) ;
#13902 = CARTESIAN_POINT ( 'NONE',  ( 123.0385396737536752, -8.611453504372539314, -17.77011218421760574 ) ) ;
#13903 = CARTESIAN_POINT ( 'NONE',  ( 123.7445081442452874, -1.561330072975668948, -17.79121239304076951 ) ) ;
#13904 = ORIENTED_EDGE ( 'NONE', *, *, #23358, .T. ) ;
#13905 = CARTESIAN_POINT ( 'NONE',  ( 127.7617783745704259, -9.363433729589941024, -9.777713163270945529 ) ) ;
#13906 = CARTESIAN_POINT ( 'NONE',  ( 117.1642148109119859, -0.8288870151387760510, -10.36305467784173118 ) ) ;
#13907 = DIRECTION ( 'NONE',  ( 0.000000000000000000, 0.3713878862591638574, -0.9284778069183724503 ) ) ;
#13908 = DIRECTION ( 'NONE',  ( 0.000000000000000000, 1.000000000000000000, 1.069961080215129965E-32 ) ) ;
#13909 = CARTESIAN_POINT ( 'NONE',  ( 123.6877814775786533, -3.383040157471821630, -19.15922257007629170 ) ) ;
#13910 = CARTESIAN_POINT ( 'NONE',  ( 111.5938171295247940, 0.1403307496149613920, -13.39321520033831447 ) ) ;
#13911 = CARTESIAN_POINT ( 'NONE',  ( 124.1975102976252003, -8.580000213326620440, -17.71054824844518905 ) ) ;
#13912 = EDGE_CURVE ( 'NONE', #27644, #42758, #11051, .T. ) ;
#13913 = ORIENTED_EDGE ( 'NONE', *, *, #1869, .T. ) ;
#13914 = DIRECTION ( 'NONE',  ( 0.000000000000000000, 0.000000000000000000, 1.000000000000000000 ) ) ;
#13915 = CARTESIAN_POINT ( 'NONE',  ( 126.4673881442452910, -7.894159318335828068, -9.358103419637847864 ) ) ;
#13916 = CARTESIAN_POINT ( 'NONE',  ( 122.4965214775786251, -10.30919188438810075, -12.61870101168855918 ) ) ;
#13917 = AXIS2_PLACEMENT_3D ( 'NONE', #7491, #21408, #21856 ) ;
#13918 = CARTESIAN_POINT ( 'NONE',  ( 115.3489614775786407, -0.8288870151387760510, -10.36305467784173118 ) ) ;
#13919 = DIRECTION ( 'NONE',  ( 0.000000000000000000, 0.9284778069183720062, 0.3713878862591650232 ) ) ;
#13920 = CARTESIAN_POINT ( 'NONE',  ( 118.4122014775786340, 0.5811942927096110934, -14.16772938898807510 ) ) ;
#13921 = CARTESIAN_POINT ( 'NONE',  ( 96.46827370896536991, -25.18754255092518335, -13.99861390895580371 ) ) ;
#13922 =( BOUNDED_CURVE ( )  B_SPLINE_CURVE ( 3, ( #25066, #39188, #11161, #21415 ),
 .UNSPECIFIED., .F., .T. ) 
 B_SPLINE_CURVE_WITH_KNOTS ( ( 4, 4 ),
 ( 1.522649623061655300, 1.570796326794896558 ),
 .UNSPECIFIED. ) 
 CURVE ( )  GEOMETRIC_REPRESENTATION_ITEM ( )  RATIONAL_B_SPLINE_CURVE ( ( 1.000000000000000000, 0.9998068339056410680, 0.9998068339056410680, 1.000000000000000000 ) ) 
 REPRESENTATION_ITEM ( '' )  );
#13923 = CARTESIAN_POINT ( 'NONE',  ( 123.5176014775786228, -0.8288870151387760510, -10.36305467784173118 ) ) ;
#13924 = ORIENTED_EDGE ( 'NONE', *, *, #26138, .F. ) ;
#13925 = CARTESIAN_POINT ( 'NONE',  ( 69.69189222814998175, -41.76310523276723785, -24.39321520033831447 ) ) ;
#13926 = CIRCLE ( 'NONE', #32096, 1.610000000000000986 ) ;
#13927 = CARTESIAN_POINT ( 'NONE',  ( 117.7882081442453170, -6.344957434206665248, -7.627207830600338134 ) ) ;
#13928 = CARTESIAN_POINT ( 'NONE',  ( 136.5278073585050720, -8.477255842839500843, -17.84929476442550822 ) ) ;
#13929 = VERTEX_POINT ( 'NONE', #27149 ) ;
#13930 = VECTOR ( 'NONE', #25326, 1000.000000000000000 ) ;
#13931 = CARTESIAN_POINT ( 'NONE',  ( 123.5633766859119760, -0.06289925094097943703, -9.412459353600674206 ) ) ;
#13932 = CARTESIAN_POINT ( 'NONE',  ( 137.2528433483991250, -1.225607619245683511, -9.593372870557891119 ) ) ;
#13933 = CARTESIAN_POINT ( 'NONE',  ( 121.8158014775786171, -5.638512984488999180, -18.83840828888717311 ) ) ;
#13934 = CARTESIAN_POINT ( 'NONE',  ( 109.1629577545248395, -7.250697342233347165, -7.631215200338321125 ) ) ;
#13935 = CARTESIAN_POINT ( 'NONE',  ( 120.3976348109119812, -7.643976991954077427, -18.09477374809248928 ) ) ;
#13936 = ORIENTED_EDGE ( 'NONE', *, *, #5000, .F. ) ;
#13937 = ORIENTED_EDGE ( 'NONE', *, *, #1919, .T. ) ;
#13938 = CARTESIAN_POINT ( 'NONE',  ( 114.3278814775786429, -10.30919188438810075, -12.61870101168855918 ) ) ;
#13939 = CARTESIAN_POINT ( 'NONE',  ( 123.2906948109119867, -1.833838273342659697, -17.42832698103878286 ) ) ;
#13940 = FACE_OUTER_BOUND ( 'NONE', #3547, .T. ) ;
#13941 = EDGE_CURVE ( 'NONE', #35613, #4412, #27066, .T. ) ;
#13942 = CARTESIAN_POINT ( 'NONE',  ( 87.68939540009954214, -25.99489077589524300, -13.39321520033831447 ) ) ;
#13943 = CARTESIAN_POINT ( 'NONE',  ( 120.5678148109119832, -8.166667518702819706, -8.995218007635861213 ) ) ;
#13944 = DIRECTION ( 'NONE',  ( 0.7871354856660198740, 0.4483307682966886643, 0.4235767337848242442 ) ) ;
#13945 = CARTESIAN_POINT ( 'NONE',  ( 123.9584548109119737, -11.97804492312075553, -17.05249760251923163 ) ) ;
#13946 = CARTESIAN_POINT ( 'NONE',  ( 123.3474214775786209, -9.988377603198976828, -10.36322818467138340 ) ) ;
#13948 = CARTESIAN_POINT ( 'NONE',  ( 118.9227414775786542, 0.4262465694468514643, -12.03445270309931736 ) ) ;
#13947 = CARTESIAN_POINT ( 'NONE',  ( 120.5678148109119832, -8.166667518702819706, -8.995218007635861213 ) ) ;
#13949 = EDGE_CURVE ( 'NONE', #22858, #44020, #21228, .T. ) ;
#13950 = CARTESIAN_POINT ( 'NONE',  ( 121.4754414775786131, -1.833838273342659697, -17.42832698103878286 ) ) ;
#13951 = CARTESIAN_POINT ( 'NONE',  ( 61.69189222814998175, -49.76310523276723785, -6.893215200338315363 ) ) ;
#13952 = CARTESIAN_POINT ( 'NONE',  ( 114.5547881442453217, -5.638512984488999180, -18.83840828888717311 ) ) ;
#13953 = ORIENTED_EDGE ( 'NONE', *, *, #26428, .T. ) ;
#13954 = CARTESIAN_POINT ( 'NONE',  ( 116.0837272357735941, -0.01944715230183663435, -12.14321520033831625 ) ) ;
#13955 = CARTESIAN_POINT ( 'NONE',  ( 109.9963952545248134, 0.8980012041604421569, -11.00651665394454071 ) ) ;
#13956 = AXIS2_PLACEMENT_3D ( 'NONE', #20588, #34466, #19671 ) ;
#13957 = CARTESIAN_POINT ( 'NONE',  ( 110.5520202545248054, 0.1403307496149616695, -11.32035403202665336 ) ) ;
#13958 = CARTESIAN_POINT ( 'NONE',  ( 106.5931921295248372, 0.8980012041604618078, -13.39321520033831447 ) ) ;
#13959 = CARTESIAN_POINT ( 'NONE',  ( 70.19189222814998175, -60.40547808481815650, -37.36498982452450690 ) ) ;
#13960 = CARTESIAN_POINT ( 'NONE',  ( 125.6164881442453094, -9.565557343593413364, -10.61323700422348004 ) ) ;
#13961 = VERTEX_POINT ( 'NONE', #41731 ) ;
#13962 = CARTESIAN_POINT ( 'NONE',  ( 123.1772414775786189, -4.089484607189486809, -7.948022111789456723 ) ) ;
#13963 = CARTESIAN_POINT ( 'NONE',  ( 113.6079577545248043, -7.250697342233347165, -7.631215200338321125 ) ) ;
#13964 = CARTESIAN_POINT ( 'NONE',  ( 123.3116793777725064, -1.267766418764731728, -16.93314635290706605 ) ) ;
#13965 = CARTESIAN_POINT ( 'NONE',  ( 123.8579614775786126, 0.5811942927096110934, -14.16772938898807510 ) ) ;
#13966 = CARTESIAN_POINT ( 'NONE',  ( 124.9924948109119924, -4.089484607189486809, -7.948022111789456723 ) ) ;
#13967 = CARTESIAN_POINT ( 'NONE',  ( 119.5350954359119839, 0.5291689781388270175, -13.89700978578772705 ) ) ;
#13968 = CARTESIAN_POINT ( 'NONE',  ( 111.8886348109120092, -3.383040157471821630, -19.15922257007629170 ) ) ;
#13969 = CARTESIAN_POINT ( 'NONE',  ( 115.2053796295247849, -4.863998795839590272, -19.15521520033831493 ) ) ;
#13970 = CARTESIAN_POINT ( 'NONE',  ( 106.8015515045248378, -2.477300249445798297, -7.631215200338321125 ) ) ;
#13971 = ORIENTED_EDGE ( 'NONE', *, *, #23345, .T. ) ;
#13972 = DIRECTION ( 'NONE',  ( 0.9609149988134837450, -0.1028163501681639419, 0.2570431154366518145 ) ) ;
#13973 = CARTESIAN_POINT ( 'NONE',  ( 116.8805814775786445, -3.505236298600246325, -18.68346056562440793 ) ) ;
#13974 = CARTESIAN_POINT ( 'NONE',  ( 112.8529881442453302, -1.561330072975668060, -17.79121239304076596 ) ) ;
#13975 = CARTESIAN_POINT ( 'NONE',  ( 114.6497546295247929, -4.863998795839590272, -7.631215200338315796 ) ) ;
#13976 = CARTESIAN_POINT ( 'NONE',  ( 108.0517077545248696, -2.791137627527939813, -18.39754474579286025 ) ) ;
#13977 = CARTESIAN_POINT ( 'NONE',  ( 121.5321681442453183, -0.1624402480850797581, -16.17319339645315424 ) ) ;
#13978 = CARTESIAN_POINT ( 'NONE',  ( 119.0361948109119652, -2.084020599724406786, -8.691656652584148546 ) ) ;
#13979 = CARTESIAN_POINT ( 'NONE',  ( 112.2857214775786474, -5.574606645277164318, -18.38911715685844683 ) ) ;
#13980 = ORIENTED_EDGE ( 'NONE', *, *, #18106, .F. ) ;
#13981 = CARTESIAN_POINT ( 'NONE',  ( 124.4819548109119722, -2.084020599724406786, -8.691656652584148546 ) ) ;
#13982 = CARTESIAN_POINT ( 'NONE',  ( 83.83554121260367253, -25.23119213852205789, -15.24166438581092109 ) ) ;
#13983 = CARTESIAN_POINT ( 'NONE',  ( 112.6828081442453282, -2.084020599724406786, -8.691656652584148546 ) ) ;
#13984 = ORIENTED_EDGE ( 'NONE', *, *, #38175, .F. ) ;
#13985 = PLANE ( 'NONE',  #9964 ) ;
#13986 = EDGE_CURVE ( 'NONE', #30218, #43475, #43608, .T. ) ;
#13987 = CARTESIAN_POINT ( 'NONE',  ( 112.0799890045248475, -9.868328341294098749, -11.32035403202665869 ) ) ;
#13988 = CIRCLE ( 'NONE', #19814, 1.610000000000000986 ) ;
#13989 = ORIENTED_EDGE ( 'NONE', *, *, #15376, .F. ) ;
#13990 = CARTESIAN_POINT ( 'NONE',  ( 119.2063748109119814, -7.894159318335828068, -9.358103419637847864 ) ) ;
#13991 = CARTESIAN_POINT ( 'NONE',  ( 113.5904348109119866, -2.084020599724406786, -8.691656652584148546 ) ) ;
#13992 = FACE_OUTER_BOUND ( 'NONE', #14099, .T. ) ;
#13993 = CARTESIAN_POINT ( 'NONE',  ( 123.8411891859119862, -1.406689858478933353, -17.56299727309130887 ) ) ;
#13994 = ORIENTED_EDGE ( 'NONE', *, *, #3118, .F. ) ;
#13995 = DIRECTION ( 'NONE',  ( 0.000000000000000000, 0.3818493186865927203, -0.9242245927363029745 ) ) ;
#13996 = CARTESIAN_POINT ( 'NONE',  ( 124.8633137343397692, -2.383538422968402237, -6.106049506750366618 ) ) ;
#13997 = CARTESIAN_POINT ( 'NONE',  ( 114.5108483795247878, -0.7896495226426338832, -9.318865927141430916 ) ) ;
#13998 = EDGE_CURVE ( 'NONE', #17646, #21796, #31408, .T. ) ;
#13999 = EDGE_CURVE ( 'NONE', #38298, #7297, #9803, .T. ) ;
#14000 = CARTESIAN_POINT ( 'NONE',  ( 86.48169505875749508, -24.14644159042263993, -12.62951656296512937 ) ) ;
#14001 = CARTESIAN_POINT ( 'NONE',  ( 121.4754414775786131, -1.833838273342659697, -17.42832698103878286 ) ) ;
#14002 = CARTESIAN_POINT ( 'NONE',  ( 119.0929214775786278, -4.153390946401325223, -8.397313243818185668 ) ) ;
#14003 = DIRECTION ( 'NONE',  ( -1.156482317317869950E-15, -1.000000000000000000, 0.000000000000000000 ) ) ;
#14004 = ORIENTED_EDGE ( 'NONE', *, *, #11080, .F. ) ;
#14005 = DIRECTION ( 'NONE',  ( -0.000000000000000000, -0.9284778069183718952, -0.3713878862591649677 ) ) ;
#14006 = CARTESIAN_POINT ( 'NONE',  ( 115.6325948109119821, -9.565557343593413364, -10.61323700422348004 ) ) ;
#14007 = CIRCLE ( 'NONE', #9749, 1.587499999999998579 ) ;
#14008 = CARTESIAN_POINT ( 'NONE',  ( 125.1626748109119802, -0.1624402480850797581, -16.17319339645315424 ) ) ;
#14009 = VECTOR ( 'NONE', #11321, 1000.000000000000114 ) ;
#14010 = CARTESIAN_POINT ( 'NONE',  ( 72.75524511225664526, -29.99489077589588959, -18.39321520033831803 ) ) ;
#14011 = CARTESIAN_POINT ( 'NONE',  ( 126.0135748109119902, -8.166667518702819706, -8.995218007635861213 ) ) ;
#14012 = CARTESIAN_POINT ( 'NONE',  ( 115.7460481442453357, 0.9020085738987339008, -11.91225656197089222 ) ) ;
#14013 = ORIENTED_EDGE ( 'NONE', *, *, #41209, .T. ) ;
#14014 = CARTESIAN_POINT ( 'NONE',  ( 112.7395348109119766, -5.638512984488999180, -18.83840828888717311 ) ) ;
#14015 = DIRECTION ( 'NONE',  ( 1.000000000000000000, 0.000000000000000000, -0.000000000000000000 ) ) ;
#14016 = CARTESIAN_POINT ( 'NONE',  ( 110.5520202545248054, -10.62599879583958717, -15.77991374673208469 ) ) ;
#14017 = CARTESIAN_POINT ( 'NONE',  ( 112.2857214775786474, -4.089484607189486809, -7.948022111789456723 ) ) ;
#14018 = CARTESIAN_POINT ( 'NONE',  ( 112.1722681442453222, -0.4660016031367893996, -10.09054647747474043 ) ) ;
#14019 = CARTESIAN_POINT ( 'NONE',  ( 124.5954081442453116, -6.222761293078241884, -8.102969835052219238 ) ) ;
#14020 = CYLINDRICAL_SURFACE ( 'NONE', #30804, 10.00000000000000000 ) ;
#14021 = CARTESIAN_POINT ( 'NONE',  ( 108.6073327545248048, -6.936859964151250502, -8.388885654883777576 ) ) ;
#14022 = VECTOR ( 'NONE', #40292, 1000.000000000000000 ) ;
#14023 = CARTESIAN_POINT ( 'NONE',  ( 70.19189222814998175, -65.04786711941001442, -39.22192925582032785 ) ) ;
#14024 = CARTESIAN_POINT ( 'NONE',  ( 109.2294377395977989, -7.996724596857648137, -17.72013350706484047 ) ) ;
#14025 = CARTESIAN_POINT ( 'NONE',  ( 118.0151148109119816, 0.4262465694468514643, -12.03445270309931736 ) ) ;
#14026 = CARTESIAN_POINT ( 'NONE',  ( 105.6903015045248253, -2.477300249445798297, -7.631215200338321125 ) ) ;
#14027 = CARTESIAN_POINT ( 'NONE',  ( 115.0664733795247798, -1.325403438956436419, -9.854619843455211026 ) ) ;
#14028 = CARTESIAN_POINT ( 'NONE',  ( 108.6073327545248048, -2.477300249445798297, -19.15521520033831138 ) ) ;
#14029 = CARTESIAN_POINT ( 'NONE',  ( 96.46827370896536991, -26.99359428275991846, -13.24861209478998170 ) ) ;
#14030 = CARTESIAN_POINT ( 'NONE',  ( 124.0848681442452772, -4.089484607189486809, -7.948022111789456723 ) ) ;
#14031 = CARTESIAN_POINT ( 'NONE',  ( 120.5468302440515203, -2.467220198592777969, -17.83387418641524391 ) ) ;
#14032 = CARTESIAN_POINT ( 'NONE',  ( 121.7590748109119687, -7.893985811506177619, -18.51759400769804742 ) ) ;
#14033 = CARTESIAN_POINT ( 'NONE',  ( 115.1220548109119761, -8.166667518702817929, -8.995218007635861213 ) ) ;
#14034 = EDGE_LOOP ( 'NONE', ( #9053, #44887, #29121, #38334 ) ) ;
#14035 = CARTESIAN_POINT ( 'NONE',  ( 114.1009748109119784, -5.574606645277164318, -18.38911715685844683 ) ) ;
#14036 = CARTESIAN_POINT ( 'NONE',  ( 124.1983214775786166, -8.166667518702819706, -8.995218007635861213 ) ) ;
#14037 = CARTESIAN_POINT ( 'NONE',  ( 119.6601881442453106, -8.166667518702819706, -8.995218007635861213 ) ) ;
#14038 = CARTESIAN_POINT ( 'NONE',  ( 115.3489614775786407, -0.8288870151387760510, -10.36305467784173118 ) ) ;
#14039 = ORIENTED_EDGE ( 'NONE', *, *, #26503, .F. ) ;
#14040 = CARTESIAN_POINT ( 'NONE',  ( 122.0994348109119443, -10.15424416112533912, -14.75197769757731336 ) ) ;
#14041 = AXIS2_PLACEMENT_3D ( 'NONE', #18006, #24629, #38511 ) ;
#14042 = CARTESIAN_POINT ( 'NONE',  ( 117.0507614775786465, -10.30919188438810075, -12.61870101168855918 ) ) ;
#14043 = CARTESIAN_POINT ( 'NONE',  ( 137.5015123043530991, 0.1307850961568663151, -13.82943359837360298 ) ) ;
#14044 = CARTESIAN_POINT ( 'NONE',  ( 114.2330358795247776, -0.7896495226426338832, -17.46756447353520159 ) ) ;
#14045 =( GEOMETRIC_REPRESENTATION_CONTEXT ( 3 ) GLOBAL_UNCERTAINTY_ASSIGNED_CONTEXT ( ( #42019 ) ) GLOBAL_UNIT_ASSIGNED_CONTEXT ( ( #14534, #41472, #41691 ) ) REPRESENTATION_CONTEXT ( 'NONE', 'WORKASPACE' ) );
#14046 = CARTESIAN_POINT ( 'NONE',  ( 70.19189222814998175, -100.0979043305785581, -53.24182196210380624 ) ) ;
#14047 = CARTESIAN_POINT ( 'NONE',  ( 90.48265143217095385, -25.18747534170762492, -13.05962633474799439 ) ) ;
#14048 = CARTESIAN_POINT ( 'NONE',  ( 87.02785693856107230, -25.23119213852205789, -15.24166438581092109 ) ) ;
#14049 = VECTOR ( 'NONE', #11478, 1000.000000000000000 ) ;
#14050 = CARTESIAN_POINT ( 'NONE',  ( 115.1787814775786387, -9.988377603198976828, -10.36322818467138340 ) ) ;
#14051 = EDGE_CURVE ( 'NONE', #22660, #19817, #9587, .T. ) ;
#14052 = DIRECTION ( 'NONE',  ( 0.000000000000000000, 0.000000000000000000, -1.000000000000000000 ) ) ;
#14053 = CARTESIAN_POINT ( 'NONE',  ( 112.5126281442453120, 0.1319031606808879209, -14.10382304977623669 ) ) ;
#14054 = CARTESIAN_POINT ( 'NONE',  ( 111.3661041094426878, 0.3591747506842615789, -12.14321520033830026 ) ) ;
#14055 = CARTESIAN_POINT ( 'NONE',  ( 96.46827370896536991, -26.80223900086530264, -12.78781649172082879 ) ) ;
#14056 = CARTESIAN_POINT ( 'NONE',  ( 112.9828796295247884, -4.863998795839590272, -8.388885654883775800 ) ) ;
#14057 = CARTESIAN_POINT ( 'NONE',  ( 117.1642148109119859, -9.261995988541697145, -16.69588392320189030 ) ) ;
#14058 = CARTESIAN_POINT ( 'NONE',  ( 90.25835095068887881, -11.48803753340849632, -13.24321520033831412 ) ) ;
#14059 = CARTESIAN_POINT ( 'NONE',  ( 96.54708369096698561, -27.29184247633061489, -11.60278472507885894 ) ) ;
#14060 = CARTESIAN_POINT ( 'NONE',  ( 118.8092881442453290, -9.988377603198960841, -10.36322818467135853 ) ) ;
#14061 = CARTESIAN_POINT ( 'NONE',  ( 138.2184548109119930, -5.044325091639137781, -11.90409383958792411 ) ) ;
#14062 = ORIENTED_EDGE ( 'NONE', *, *, #30487, .T. ) ;
#14063 = CARTESIAN_POINT ( 'NONE',  ( 125.6164881442453094, 0.2603800115204892296, -16.42320221600525088 ) ) ;
#14064 = CARTESIAN_POINT ( 'NONE',  ( 123.0637881442452937, -0.4660016031367893996, -10.09054647747474043 ) ) ;
#14065 = DIRECTION ( 'NONE',  ( 0.000000000000000000, 0.3818493186865927203, -0.9242245927363029745 ) ) ;
#14066 = CARTESIAN_POINT ( 'NONE',  ( 115.4624148109119943, -4.153390946401321671, -8.397313243818183892 ) ) ;
#14068 = CARTESIAN_POINT ( 'NONE',  ( 113.0798948109119948, -8.899110576539710493, -16.42337572283490132 ) ) ;
#14067 = CIRCLE ( 'NONE', #16256, 5.000000000000002665 ) ;
#14069 = CARTESIAN_POINT ( 'NONE',  ( 62.01216987384223955, -37.94672044352281404, -5.762757384007758610 ) ) ;
#14070 = CARTESIAN_POINT ( 'NONE',  ( 112.1494421295248003, 0.8980012041604618078, -13.39321520033831447 ) ) ;
#14071 = CARTESIAN_POINT ( 'NONE',  ( 120.3976348109119812, -7.643976991954077427, -18.09477374809248928 ) ) ;
#14072 = AXIS2_PLACEMENT_3D ( 'NONE', #7727, #1333, #4979 ) ;
#14073 = CARTESIAN_POINT ( 'NONE',  ( 119.3765548109119834, -10.15424416112533912, -14.75197769757731336 ) ) ;
#14074 = CARTESIAN_POINT ( 'NONE',  ( 109.2293787433446539, -7.236786641593805136, -8.226045299710833092 ) ) ;
#14075 = CARTESIAN_POINT ( 'NONE',  ( 123.0077516859119839, -9.665098340737509730, -17.37397104707595474 ) ) ;
#14076 = CARTESIAN_POINT ( 'NONE',  ( 109.7185827545247889, -6.936859964151250502, -8.388885654883777576 ) ) ;
#14077 = CARTESIAN_POINT ( 'NONE',  ( 87.41631446019775353, -26.60966817898065884, -11.90521360603286816 ) ) ;
#14078 = CARTESIAN_POINT ( 'NONE',  ( 112.3991748109119868, -8.166667518702817929, -8.995218007635859436 ) ) ;
#14079 = CARTESIAN_POINT ( 'NONE',  ( 114.8951481442453115, -0.4660016031367893996, -10.09054647747474043 ) ) ;
#14080 = CARTESIAN_POINT ( 'NONE',  ( 112.9828796295247884, -4.863998795839590272, -19.15521520033831493 ) ) ;
#14081 = LINE ( 'NONE', #24131, #21356 ) ;
#14082 = ORIENTED_EDGE ( 'NONE', *, *, #39569, .T. ) ;
#14083 = DIRECTION ( 'NONE',  ( 0.1352586133457950590, 0.9908103287288504424, 0.000000000000000000 ) ) ;
#14084 = AXIS2_PLACEMENT_3D ( 'NONE', #23702, #27783, #37591 ) ;
#14085 = CARTESIAN_POINT ( 'NONE',  ( 121.5321681442453183, -9.988377603198976828, -10.36322818467138340 ) ) ;
#14086 = CARTESIAN_POINT ( 'NONE',  ( 112.6828081442453282, -7.893985811506177619, -18.51759400769804742 ) ) ;
#14087 = CARTESIAN_POINT ( 'NONE',  ( 119.2631014775786298, -9.565557343593413364, -10.61323700422348004 ) ) ;
#14088 = CARTESIAN_POINT ( 'NONE',  ( 125.6164881442453094, 0.2603800115204892296, -16.42320221600525088 ) ) ;
#14089 = CARTESIAN_POINT ( 'NONE',  ( 116.9373081442452929, -8.166667518702817929, -8.995218007635861213 ) ) ;
#14090 = CARTESIAN_POINT ( 'NONE',  ( 108.6073327545248048, -6.936859964151250502, -8.388885654883777576 ) ) ;
#14091 = CARTESIAN_POINT ( 'NONE',  ( 112.1722681442453222, -8.899110576539710493, -16.42337572283490132 ) ) ;
#14092 = FACE_OUTER_BOUND ( 'NONE', #42663, .T. ) ;
#14093 = ORIENTED_EDGE ( 'NONE', *, *, #31868, .F. ) ;
#14094 = CARTESIAN_POINT ( 'NONE',  ( 121.2485348109119769, -0.4660016031367893996, -10.09054647747474043 ) ) ;
#14095 = B_SPLINE_CURVE_WITH_KNOTS ( 'NONE', 3,
 ( #43906, #12675, #5580, #12447, #5134, #19283, #2155, #8788, #29989, #19504 ),
 .UNSPECIFIED., .F., .F.,
 ( 4, 3, 3, 4 ),
 ( 0.000000000000000000, 0.0002476487219222810133, 0.0004952974148303710203, 0.0009534114850261840753 ),
 .UNSPECIFIED. ) ;
#14096 = VECTOR ( 'NONE', #11787, 1000.000000000000000 ) ;
#14097 = DIRECTION ( 'NONE',  ( 1.000000000000000000, 0.000000000000000000, -0.000000000000000000 ) ) ;
#14098 = CARTESIAN_POINT ( 'NONE',  ( 117.1642148109119859, -9.261995988541697145, -16.69588392320189030 ) ) ;
#14099 = EDGE_LOOP ( 'NONE', ( #16617, #38695, #17604, #35364, #34348 ) ) ;
#14100 = CARTESIAN_POINT ( 'NONE',  ( 114.3719421295247827, 0.8980012041604618078, -13.39321520033831447 ) ) ;
#14101 = AXIS2_PLACEMENT_3D ( 'NONE', #27659, #6899, #10114 ) ;
#14102 = CARTESIAN_POINT ( 'NONE',  ( 126.1270281442452870, -10.30919188438810075, -12.61870101168855918 ) ) ;
#14103 = DIRECTION ( 'NONE',  ( 1.000000000000000000, 0.000000000000000000, -0.000000000000000000 ) ) ;
#14104 = CARTESIAN_POINT ( 'NONE',  ( 112.6828081442453282, -2.084020599724406786, -8.691656652584148546 ) ) ;
#14105 = LINE ( 'NONE', #35044, #25131 ) ;
#14106 = CARTESIAN_POINT ( 'NONE',  ( 119.2631014775786298, -9.565557343593413364, -10.61323700422348004 ) ) ;
#14107 = FACE_OUTER_BOUND ( 'NONE', #11093, .T. ) ;
#14108 = CARTESIAN_POINT ( 'NONE',  ( 120.1140014775786398, -7.894159318335828068, -9.358103419637847864 ) ) ;
#14109 = CIRCLE ( 'NONE', #9764, 1.499999999999996225 ) ;
#14110 = DIRECTION ( 'NONE',  ( 0.9609149988134837450, -0.1028163501681639419, 0.2570431154366518145 ) ) ;
#14111 = CARTESIAN_POINT ( 'NONE',  ( 117.8449348109119938, -1.833838273342659253, -17.42832698103878286 ) ) ;
#14112 = CARTESIAN_POINT ( 'NONE',  ( 111.7184548109119788, -9.261995988541697145, -16.69588392320189030 ) ) ;
#14113 = CARTESIAN_POINT ( 'NONE',  ( 115.1220548109119761, -8.166667518702817929, -8.995218007635861213 ) ) ;
#14114 = CARTESIAN_POINT ( 'NONE',  ( 123.0070614775786311, 0.9020085738987273505, -11.91225656197088512 ) ) ;
#14115 = CARTESIAN_POINT ( 'NONE',  ( 117.9583881442453048, 0.1319031606808879209, -14.10382304977623669 ) ) ;
#14116 = ORIENTED_EDGE ( 'NONE', *, *, #35623, .F. ) ;
#14117 = CARTESIAN_POINT ( 'NONE',  ( 117.3343948109119737, -3.383040157471821630, -19.15922257007629170 ) ) ;
#14118 = CARTESIAN_POINT ( 'NONE',  ( 106.5931921295248372, 0.8980012041604618078, -13.39321520033831447 ) ) ;
#14119 = DIRECTION ( 'NONE',  ( 0.000000000000000000, 0.3818493186865927203, -0.9242245927363029745 ) ) ;
#14120 = DIRECTION ( 'NONE',  ( 1.000000000000000000, 0.000000000000000000, -0.000000000000000000 ) ) ;
#14121 = CARTESIAN_POINT ( 'NONE',  ( 113.2987212410415765, 0.7607806665037644134, -12.14321520033829493 ) ) ;
#14122 = CARTESIAN_POINT ( 'NONE',  ( 121.8725281442453223, -3.383040157471821630, -19.15922257007629170 ) ) ;
#14123 = ORIENTED_EDGE ( 'NONE', *, *, #11679, .T. ) ;
#14124 = CARTESIAN_POINT ( 'NONE',  ( 118.2795432127138611, -2.191907684172563986, -18.20049396185734025 ) ) ;
#14125 = CARTESIAN_POINT ( 'NONE',  ( 117.9583881442453048, 0.1319031606808879209, -14.10382304977623669 ) ) ;
#14126 = DIRECTION ( 'NONE',  ( 1.387778780781445676E-17, -0.9284778069183720062, -0.3713878862591650232 ) ) ;
#14127 = CARTESIAN_POINT ( 'NONE',  ( 65.38091086278477349, -15.98735439659152036, -17.11731565370446972 ) ) ;
#14128 = LINE ( 'NONE', #24618, #16628 ) ;
#14129 = AXIS2_PLACEMENT_3D ( 'NONE', #22848, #13275, #23545 ) ;
#14130 = CARTESIAN_POINT ( 'NONE',  ( 113.6079577545248043, -2.791137627527939813, -18.39754474579286025 ) ) ;
#14131 = CARTESIAN_POINT ( 'NONE',  ( 89.13407410398241382, -10.42653939434942245, -14.07237609319362193 ) ) ;
#14132 = ORIENTED_EDGE ( 'NONE', *, *, #35159, .T. ) ;
#14133 = CARTESIAN_POINT ( 'NONE',  ( 114.4413348109119823, -9.261995988541697145, -16.69588392320189030 ) ) ;
#14134 = CARTESIAN_POINT ( 'NONE',  ( 125.3895814775786448, -2.084020599724406786, -8.691656652584148546 ) ) ;
#14135 = CARTESIAN_POINT ( 'NONE',  ( 124.6521348109119884, -1.561330072975668948, -17.79121239304076951 ) ) ;
#14136 = CARTESIAN_POINT ( 'NONE',  ( 115.8595014775786609, -7.643976991954077427, -18.09477374809248928 ) ) ;
#14137 = CARTESIAN_POINT ( 'NONE',  ( 83.16394245587648015, -30.76310523276723785, -21.89321520033831447 ) ) ;
#14138 =( LENGTH_UNIT ( ) NAMED_UNIT ( * ) SI_UNIT ( .MILLI., .METRE. ) );
#14139 = CARTESIAN_POINT ( 'NONE',  ( 119.8870948109119752, -9.261995988541697145, -16.69588392320189030 ) ) ;
#14140 = CARTESIAN_POINT ( 'NONE',  ( 90.72400676789006013, -25.38011337280982715, -14.88121679464376257 ) ) ;
#14141 = CARTESIAN_POINT ( 'NONE',  ( 110.0133197905468734, 0.6938714319018670640, -12.14321520033834823 ) ) ;
#14142 = CARTESIAN_POINT ( 'NONE',  ( 124.5954081442453116, -6.222761293078241884, -8.102969835052219238 ) ) ;
#14143 = ORIENTED_EDGE ( 'NONE', *, *, #32555, .F. ) ;
#14144 = ADVANCED_FACE ( 'NONE', ( #42624 ), #19106, .T. ) ;
#14145 = LINE ( 'NONE', #41969, #43100 ) ;
#14146 = CARTESIAN_POINT ( 'NONE',  ( 117.4478481442453131, 0.2603800115204892296, -16.42320221600525088 ) ) ;
#14147 = CARTESIAN_POINT ( 'NONE',  ( 123.1772414775786189, -5.574606645277164318, -18.38911715685844683 ) ) ;
#14148 = ORIENTED_EDGE ( 'NONE', *, *, #12193, .T. ) ;
#14149 = CARTESIAN_POINT ( 'NONE',  ( 136.7741008876067781, -1.264212383164096121, -9.092737378789559344 ) ) ;
#14150 = CARTESIAN_POINT ( 'NONE',  ( 124.0848681442452772, -4.089484607189486809, -7.948022111789456723 ) ) ;
#14151 = CARTESIAN_POINT ( 'NONE',  ( 109.3018640045248304, -10.62599879583958717, -11.00651665394454604 ) ) ;
#14152 = CARTESIAN_POINT ( 'NONE',  ( 121.4754414775786131, -1.833838273342659697, -17.42832698103878286 ) ) ;
#14153 = ORIENTED_EDGE ( 'NONE', *, *, #25608, .F. ) ;
#14154 = ORIENTED_EDGE ( 'NONE', *, *, #37928, .T. ) ;
#14155 = CARTESIAN_POINT ( 'NONE',  ( 113.3635281442453504, -9.988377603198976828, -10.36322818467138340 ) ) ;
#14156 = CARTESIAN_POINT ( 'NONE',  ( 124.6521348109119884, -7.894159318335828068, -9.358103419637847864 ) ) ;
#14157 = CARTESIAN_POINT ( 'NONE',  ( 79.40884336804893451, 5.049947642532015557, -20.47066126174475897 ) ) ;
#14158 = CARTESIAN_POINT ( 'NONE',  ( 121.8725281442453223, -3.383040157471821630, -19.15922257007629170 ) ) ;
#14159 = ADVANCED_FACE ( 'NONE', ( #3851 ), #885, .F. ) ;
#14160 = DIRECTION ( 'NONE',  ( -1.899192652838769965E-30, -3.023161660021630136E-44, -1.000000000000000000 ) ) ;
#14161 = DIRECTION ( 'NONE',  ( -0.000000000000000000, -0.9284778069183720062, -0.3713878862591650232 ) ) ;
#14162 = CARTESIAN_POINT ( 'NONE',  ( 123.1772414775786189, -4.089484607189486809, -7.948022111789456723 ) ) ;
#14164 = CARTESIAN_POINT ( 'NONE',  ( 125.0492214775786266, -3.505236298600246325, -18.68346056562440793 ) ) ;
#14163 = CARTESIAN_POINT ( 'NONE',  ( 120.9081748109119872, -5.638512984488999180, -18.83840828888717311 ) ) ;
#14165 = CARTESIAN_POINT ( 'NONE',  ( 119.5467348109119712, -5.574606645277164318, -18.38911715685844683 ) ) ;
#14166 = CARTESIAN_POINT ( 'NONE',  ( 91.65862616933031859, -25.23119213852205789, -15.24166438581092109 ) ) ;
#14167 = CARTESIAN_POINT ( 'NONE',  ( 114.2711548109119803, -9.988377603198976828, -10.36322818467138340 ) ) ;
#14168 = ADVANCED_FACE ( 'NONE', ( #8637 ), #23794, .F. ) ;
#14169 = ORIENTED_EDGE ( 'NONE', *, *, #2761, .F. ) ;
#14170 = EDGE_CURVE ( 'NONE', #38280, #13961, #39782, .T. ) ;
#14171 = CARTESIAN_POINT ( 'NONE',  ( 125.8328548109119964, -8.862178061931794915, -16.39564131203325559 ) ) ;
#14172 = CARTESIAN_POINT ( 'NONE',  ( 105.6903015045248253, -2.477300249445798297, -7.631215200338321125 ) ) ;
#14173 = CARTESIAN_POINT ( 'NONE',  ( 107.9128015045248219, -6.936859964151250502, -18.39754474579286025 ) ) ;
#14174 = CARTESIAN_POINT ( 'NONE',  ( 115.5526452545247622, -9.868328341294098749, -15.46607636864997204 ) ) ;
#14175 = CARTESIAN_POINT ( 'NONE',  ( 125.3790414775786388, -0.8658195297466895202, -10.39078908864337514 ) ) ;
#14176 = CARTESIAN_POINT ( 'NONE',  ( 125.3328548109119964, -0.8288870151387760510, -10.36305467784173118 ) ) ;
#14177 = VERTEX_POINT ( 'NONE', #5350 ) ;
#14178 = CARTESIAN_POINT ( 'NONE',  ( 113.5337081442453240, -0.8288870151387760510, -10.36305467784173118 ) ) ;
#14179 = CARTESIAN_POINT ( 'NONE',  ( 110.1353015045248469, -2.477300249445798297, -7.631215200338321125 ) ) ;
#14180 = LINE ( 'NONE', #17607, #37978 ) ;
#14181 = CARTESIAN_POINT ( 'NONE',  ( 123.2906948109119867, -8.166667518702819706, -8.995218007635861213 ) ) ;
#14182 =( BOUNDED_CURVE ( )  B_SPLINE_CURVE ( 2, ( #21563, #1259, #18376, #21338, #35450, #4225, #18144, #32264, #1032, #8333, #42988, #35223, #28860, #42772, #8111, #3997, #11755 ),
 .UNSPECIFIED., .F., .T. ) 
 B_SPLINE_CURVE_WITH_KNOTS ( ( 3, 2, 2, 2, 2, 2, 2, 2, 3 ),
 ( 0.3921282416568590001, 0.3984375000000000000, 0.4062500000000000000, 0.4140625000000000000, 0.4218750000000000000, 0.4296875000000000000, 0.4375000000000000000, 0.4453125000000000000, 0.4516217583431409999 ),
 .UNSPECIFIED. ) 
 CURVE ( )  GEOMETRIC_REPRESENTATION_ITEM ( )  RATIONAL_B_SPLINE_CURVE ( ( 0.9763430640195970289, 0.9385262470928680267, 1.000000000000000000, 0.9238795325112869605, 1.000000000000000000, 0.9238795325112869605, 1.000000000000000000, 0.9238795325112869605, 1.000000000000000000, 0.9238795325112869605, 1.000000000000000000, 0.9238795325112869605, 1.000000000000000000, 0.9238795325112869605, 1.000000000000000000, 0.9385262470928680267, 0.9763430640195970289 ) ) 
 REPRESENTATION_ITEM ( '' )  );
#14183 = CARTESIAN_POINT ( 'NONE',  ( 124.9357681442453014, -1.834011780172310813, -8.268836392978581529 ) ) ;
#14184 = DIRECTION ( 'NONE',  ( -0.9609149988134837450, 0.1028163501681639419, -0.2570431154366518145 ) ) ;
#14185 = CARTESIAN_POINT ( 'NONE',  ( 113.7606148109119886, -1.561330072975668060, -17.79121239304076596 ) ) ;
#14186 = EDGE_CURVE ( 'NONE', #13861, #9687, #26558, .T. ) ;
#14187 = CARTESIAN_POINT ( 'NONE',  ( 114.8581140045248361, -10.62599879583958717, -11.00651665394454604 ) ) ;
#14188 = CARTESIAN_POINT ( 'NONE',  ( 114.7192077545248594, -2.791137627527939813, -18.39754474579286025 ) ) ;
#14189 = AXIS2_PLACEMENT_3D ( 'NONE', #20465, #13620, #34346 ) ;
#14190 = VERTEX_POINT ( 'NONE', #40237 ) ;
#14191 = CARTESIAN_POINT ( 'NONE',  ( 109.8889130180080826, 0.7607806665037644134, -14.64321520033833579 ) ) ;
#14192 = CARTESIAN_POINT ( 'NONE',  ( 116.3700414775786527, -4.153390946401321671, -8.397313243818183892 ) ) ;
#14193 = CARTESIAN_POINT ( 'NONE',  ( 113.7606148109119886, -1.561330072975668060, -17.79121239304076596 ) ) ;
#14194 = CARTESIAN_POINT ( 'NONE',  ( 113.3301452545248083, 0.8980012041604421569, -11.00651665394454071 ) ) ;
#14195 = CARTESIAN_POINT ( 'NONE',  ( 105.5513952545248060, -9.868328341294098749, -15.46607636864997204 ) ) ;
#14196 = ADVANCED_FACE ( 'NONE', ( #30203, #26100 ), #9232, .F. ) ;
#14197 = CARTESIAN_POINT ( 'NONE',  ( 120.5110881442453206, -3.505236298600246325, -18.68346056562440793 ) ) ;
#14198 = CARTESIAN_POINT ( 'NONE',  ( 120.9649014775786355, -6.222761293078241884, -8.102969835052219238 ) ) ;
#14199 = CARTESIAN_POINT ( 'NONE',  ( 113.9307948109119764, -10.15424416112533912, -14.75197769757731336 ) ) ;
#14200 = EDGE_LOOP ( 'NONE', ( #5758, #37036, #6814, #30785 ) ) ;
#14201 = EDGE_CURVE ( 'NONE', #6624, #24134, #4892, .T. ) ;
#14202 = EDGE_CURVE ( 'NONE', #37055, #36801, #12486, .T. ) ;
#14203 = VECTOR ( 'NONE', #23146, 1000.000000000000227 ) ;
#14204 = CARTESIAN_POINT ( 'NONE',  ( 124.8223148109119762, -10.15424416112533912, -14.75197769757731336 ) ) ;
#14205 = DIRECTION ( 'NONE',  ( 0.5040994586965589219, 0.8636456077245089347, 0.000000000000000000 ) ) ;
#14206 = CARTESIAN_POINT ( 'NONE',  ( 114.4980614775786734, -2.084020599724406786, -8.691656652584148546 ) ) ;
#14207 = ORIENTED_EDGE ( 'NONE', *, *, #22779, .T. ) ;
#14208 = CARTESIAN_POINT ( 'NONE',  ( 78.75330084444991030, 4.432659906640646241, -5.197052112444285221 ) ) ;
#14209 = CARTESIAN_POINT ( 'NONE',  ( 106.1070202545248407, -10.62599879583958717, -15.77991374673208469 ) ) ;
#14210 = CARTESIAN_POINT ( 'NONE',  ( 108.5378796295247810, -4.863998795839590272, -8.388885654883775800 ) ) ;
#14211 = ORIENTED_EDGE ( 'NONE', *, *, #23080, .T. ) ;
#14212 = CARTESIAN_POINT ( 'NONE',  ( 119.8303681442453126, 0.4262465694468514643, -12.03445270309931736 ) ) ;
#14213 = CARTESIAN_POINT ( 'NONE',  ( 114.3278814775786429, 0.1319031606808879209, -14.10382304977623669 ) ) ;
#14214 = CARTESIAN_POINT ( 'NONE',  ( 124.5837840600787274, -9.794985466449714906, -14.24011022619069600 ) ) ;
#14215 = CARTESIAN_POINT ( 'NONE',  ( 121.4103298109119748, -2.173413727453600508, -8.297982527556802879 ) ) ;
#14216 = ORIENTED_EDGE ( 'NONE', *, *, #3272, .F. ) ;
#14217 = CARTESIAN_POINT ( 'NONE',  ( 121.3000491344827481, -1.149058757900107697, -17.09122335155391781 ) ) ;
#14218 = PLANE ( 'NONE',  #26747 ) ;
#14219 = AXIS2_PLACEMENT_3D ( 'NONE', #7985, #38760, #35788 ) ;
#14220 = CARTESIAN_POINT ( 'NONE',  ( 106.1764733795248219, -1.325403438956436419, -9.854619843455211026 ) ) ;
#14221 = B_SPLINE_CURVE_WITH_KNOTS ( 'NONE', 3,
 ( #27352, #34168, #27794, #41706, #10031, #10472, #24373, #34824, #28020, #31420 ),
 .UNSPECIFIED., .F., .F.,
 ( 4, 2, 2, 2, 4 ),
 ( 0.000000000000000000, 0.2500000000000000000, 0.5000000000000000000, 0.7500000000000000000, 1.000000000000000000 ),
 .UNSPECIFIED. ) ;
#14222 = CARTESIAN_POINT ( 'NONE',  ( 113.3068014775786594, -8.166667518702817929, -8.995218007635859436 ) ) ;
#14223 = CARTESIAN_POINT ( 'NONE',  ( 122.8936081442453059, -9.565557343593413364, -10.61323700422348004 ) ) ;
#14224 = CARTESIAN_POINT ( 'NONE',  ( 116.9940348109119839, -0.1624402480850797581, -16.17319339645315424 ) ) ;
#14225 = CARTESIAN_POINT ( 'NONE',  ( 125.4210411930764337, -6.901805073872763430, -19.97202117700874524 ) ) ;
#14226 = ORIENTED_EDGE ( 'NONE', *, *, #4145, .T. ) ;
#14227 = AXIS2_PLACEMENT_3D ( 'NONE', #34273, #17626, #44786 ) ;
#14228 = CARTESIAN_POINT ( 'NONE',  ( 116.6536748109119941, -10.15424416112533912, -14.75197769757731336 ) ) ;
#14229 = DIRECTION ( 'NONE',  ( 0.000000000000000000, -0.3818493186865927203, 0.9242245927363029745 ) ) ;
#14230 = CARTESIAN_POINT ( 'NONE',  ( 116.9190222310133578, -1.244021962887374544, -16.96476564598603076 ) ) ;
#14231 = CARTESIAN_POINT ( 'NONE',  ( 113.7038881442453402, -3.383040157471821630, -19.15922257007629170 ) ) ;
#14232 = VERTEX_POINT ( 'NONE', #36796 ) ;
#14233 = CARTESIAN_POINT ( 'NONE',  ( 116.2565881442452991, -9.261995988541697145, -16.69588392320189030 ) ) ;
#14234 = CARTESIAN_POINT ( 'NONE',  ( 109.9649712410415816, 0.7607806665038616689, -12.14321520033831625 ) ) ;
#14235 = CARTESIAN_POINT ( 'NONE',  ( 111.1770983795247787, -0.7896495226426338832, -9.318865927141430916 ) ) ;
#14236 = CARTESIAN_POINT ( 'NONE',  ( 113.5337081442453240, -9.261995988541697145, -16.69588392320189030 ) ) ;
#14237 = CARTESIAN_POINT ( 'NONE',  ( 112.7395348109119766, -5.638512984488999180, -18.83840828888717311 ) ) ;
#14238 = CARTESIAN_POINT ( 'NONE',  ( 121.9859814775786333, -9.565557343593413364, -10.61323700422348004 ) ) ;
#14239 = CARTESIAN_POINT ( 'NONE',  ( 63.44904766416654951, -14.80807631840393945, -16.90507154904199538 ) ) ;
#14240 = CARTESIAN_POINT ( 'NONE',  ( 109.7880358795247986, -8.402594152722688392, -9.854619843455216355 ) ) ;
#14241 = EDGE_CURVE ( 'NONE', #33232, #1795, #28440, .T. ) ;
#14242 = VERTEX_POINT ( 'NONE', #29298 ) ;
#14243 = CARTESIAN_POINT ( 'NONE',  ( 112.0593621053768771, 0.3967854368540359999, -16.28112951403851483 ) ) ;
#14244 = CARTESIAN_POINT ( 'NONE',  ( 109.2294467825805526, -3.015950756132280475, -18.14724175160803554 ) ) ;
#14245 = CARTESIAN_POINT ( 'NONE',  ( 114.8951481442453115, -8.899110576539710493, -16.42337572283490132 ) ) ;
#14246 = CARTESIAN_POINT ( 'NONE',  ( 108.6073327545248048, -2.477300249445798297, -19.15521520033831138 ) ) ;
#14247 = CARTESIAN_POINT ( 'NONE',  ( 114.3719421295247827, -9.868328341294093420, -13.39321520033831447 ) ) ;
#14248 = CARTESIAN_POINT ( 'NONE',  ( 107.6349890045248401, 0.8980012041604421569, -15.77991374673208469 ) ) ;
#14249 = CARTESIAN_POINT ( 'NONE',  ( 94.86797725101186529, -26.87133687923154923, -13.19810066433400664 ) ) ;
#14250 = CARTESIAN_POINT ( 'NONE',  ( 125.6164881442453094, 0.2603800115204892296, -16.42320221600525088 ) ) ;
#14251 = DIRECTION ( 'NONE',  ( -1.000000000000000000, 0.000000000000000000, -0.000000000000000000 ) ) ;
#14252 = CARTESIAN_POINT ( 'NONE',  ( 123.6877814775786533, -3.383040157471821630, -19.15922257007629170 ) ) ;
#14253 = CARTESIAN_POINT ( 'NONE',  ( 115.6893214775786447, 0.5811942927096154232, -14.16772938898807155 ) ) ;
#14254 = VERTEX_POINT ( 'NONE', #18809 ) ;
#14255 = CONICAL_SURFACE ( 'NONE', #43352, 2.445500000000004448, 0.9599310885968757034 ) ;
#14256 = CARTESIAN_POINT ( 'NONE',  ( 113.1933481442453058, -5.574606645277164318, -18.38911715685844683 ) ) ;
#14257 = CARTESIAN_POINT ( 'NONE',  ( 113.2500748109119968, -6.344957434206662583, -7.627207830600332805 ) ) ;
#14258 = CARTESIAN_POINT ( 'NONE',  ( 118.0151148109119816, -10.63000616557722466, -14.87417383870573495 ) ) ;
#14259 = CARTESIAN_POINT ( 'NONE',  ( 117.6180281442453150, -8.899110576539710493, -16.42337572283490132 ) ) ;
#14260 = ORIENTED_EDGE ( 'NONE', *, *, #40083, .T. ) ;
#14261 = EDGE_CURVE ( 'NONE', #4162, #8497, #4459, .T. ) ;
#14262 = CARTESIAN_POINT ( 'NONE',  ( 120.7947214775786193, -0.8288870151387760510, -10.36305467784173118 ) ) ;
#14263 = CARTESIAN_POINT ( 'NONE',  ( 117.6747548109119919, -1.834011780172310813, -8.268836392978581529 ) ) ;
#14264 = VECTOR ( 'NONE', #672, 1000.000000000000114 ) ;
#14265 = CARTESIAN_POINT ( 'NONE',  ( 136.9920288091157943, 0.2741831093159626254, -15.27028804600930556 ) ) ;
#14266 = CARTESIAN_POINT ( 'NONE',  ( 107.8433483795247838, -0.7896495226426338832, -9.318865927141430916 ) ) ;
#14267 = PLANE ( 'NONE',  #42472 ) ;
#14268 = CARTESIAN_POINT ( 'NONE',  ( 126.8594690244564731, 0.4528996404656494557, -13.19682093318863814 ) ) ;
#14269 = DIRECTION ( 'NONE',  ( -0.2768435750659241079, -0.3568721902840695792, 0.8921882507333129819 ) ) ;
#14270 = CARTESIAN_POINT ( 'NONE',  ( 114.4980614775786592, -7.893985811506177619, -18.51759400769804742 ) ) ;
#14271 = AXIS2_PLACEMENT_3D ( 'NONE', #22927, #30450, #19291 ) ;
#14272 = DIRECTION ( 'NONE',  ( 1.000000000000000000, 0.000000000000000000, -0.000000000000000000 ) ) ;
#14273 = DIRECTION ( 'NONE',  ( -0.000000000000000000, -0.9284778069183721172, -0.3713878862591650232 ) ) ;
#14274 = CARTESIAN_POINT ( 'NONE',  ( 70.19189222814998175, -53.54563792646638376, -34.62107767336419073 ) ) ;
#14275 = CARTESIAN_POINT ( 'NONE',  ( 114.0246765045248196, -2.791137627527939813, -8.388885654883777576 ) ) ;
#14276 = CARTESIAN_POINT ( 'NONE',  ( 113.9875214775786532, -8.899110576539710493, -16.42337572283490132 ) ) ;
#14277 = CARTESIAN_POINT ( 'NONE',  ( 74.69189222814998175, -41.76310523276723785, -47.71602681600972318 ) ) ;
#14278 = AXIS2_PLACEMENT_3D ( 'NONE', #24874, #22127, #7536 ) ;
#14279 = LINE ( 'NONE', #17476, #27411 ) ;
#14281 = CARTESIAN_POINT ( 'NONE',  ( 114.4413348109119823, -9.261995988541697145, -16.69588392320189030 ) ) ;
#14280 = CARTESIAN_POINT ( 'NONE',  ( 118.5256548109119876, -0.4660016031367711919, -10.09054647747476352 ) ) ;
#14282 = DIRECTION ( 'NONE',  ( 0.000000000000000000, -0.3818493186865927203, 0.9242245927363029745 ) ) ;
#14283 = CARTESIAN_POINT ( 'NONE',  ( 117.4478481442453131, -9.565557343593413364, -10.61323700422348004 ) ) ;
#14284 = ORIENTED_EDGE ( 'NONE', *, *, #18912, .F. ) ;
#14285 = CARTESIAN_POINT ( 'NONE',  ( 121.9272896737536911, -8.611453504372539314, -17.77011218421760574 ) ) ;
#14286 = CARTESIAN_POINT ( 'NONE',  ( 122.4397948109119767, -9.988377603198976828, -10.36322818467138340 ) ) ;
#14287 = CARTESIAN_POINT ( 'NONE',  ( 114.5803015045248117, -6.936859964151250502, -18.39754474579286025 ) ) ;
#14288 = CARTESIAN_POINT ( 'NONE',  ( 116.2565881442453133, -0.8288870151387760510, -10.36305467784173118 ) ) ;
#14289 = AXIS2_PLACEMENT_3D ( 'NONE', #33089, #19210, #2715 ) ;
#14290 = CARTESIAN_POINT ( 'NONE',  ( 112.8529881442453160, -7.894159318335828068, -9.358103419637847864 ) ) ;
#14291 = CARTESIAN_POINT ( 'NONE',  ( 85.37568467414497775, -28.74641635718726462, -9.489634795554785285 ) ) ;
#14292 = CARTESIAN_POINT ( 'NONE',  ( 113.6774108795247997, -8.938348069036489818, -9.318865927141430916 ) ) ;
#14293 = CARTESIAN_POINT ( 'NONE',  ( 119.2063748109119814, -7.894159318335828068, -9.358103419637847864 ) ) ;
#14294 = CARTESIAN_POINT ( 'NONE',  ( 120.2274548109119934, -9.859900752359378018, -12.68260735090039759 ) ) ;
#14295 = CARTESIAN_POINT ( 'NONE',  ( 114.4413348109119823, -0.8288870151387681684, -10.36305467784174184 ) ) ;
#14296 = CARTESIAN_POINT ( 'NONE',  ( 109.2293722400885230, -3.002006214096174297, -8.219031836063955154 ) ) ;
#14297 = CARTESIAN_POINT ( 'NONE',  ( 120.0907204359119760, 1.345710702986147034, -13.97328579221134426 ) ) ;
#14298 = CARTESIAN_POINT ( 'NONE',  ( 110.2047546295247855, -4.863998795839590272, -18.39754474579285315 ) ) ;
#14299 = PRODUCT ( 'Reach Screw', 'Reach Screw', '', ( #44614 ) ) ;
#14300 = CARTESIAN_POINT ( 'NONE',  ( 116.4509667848042369, 2.225913487521071321, -20.42810828536804379 ) ) ;
#14301 = CARTESIAN_POINT ( 'NONE',  ( 115.8595014775786609, -1.834011780172310813, -8.268836392978581529 ) ) ;
#14302 = CARTESIAN_POINT ( 'NONE',  ( 114.4413348109119823, -9.261995988541697145, -16.69588392320189030 ) ) ;
#14303 = CARTESIAN_POINT ( 'NONE',  ( 110.2742077545248094, -7.250697342233347165, -7.631215200338321125 ) ) ;
#14304 = CARTESIAN_POINT ( 'NONE',  ( 114.1009748109119784, -4.089484607189486809, -7.948022111789456723 ) ) ;
#14305 = VERTEX_POINT ( 'NONE', #29974 ) ;
#14306 = CARTESIAN_POINT ( 'NONE',  ( 71.02242295334774269, -58.97436600404279972, -39.89735762937828412 ) ) ;
#14307 = CARTESIAN_POINT ( 'NONE',  ( 120.7379948109119709, -10.63000616557722466, -14.87417383870573495 ) ) ;
#14308 = CARTESIAN_POINT ( 'NONE',  ( 116.5969481442453031, 0.5811942927096154232, -14.16772938898807155 ) ) ;
#14309 = EDGE_CURVE ( 'NONE', #29611, #13251, #3005, .T. ) ;
#14310 = CARTESIAN_POINT ( 'NONE',  ( 121.5321681442453183, -0.1624402480850797581, -16.17319339645315424 ) ) ;
#14311 = CIRCLE ( 'NONE', #1187, 2.445500000000004448 ) ;
#14312 = B_SPLINE_CURVE_WITH_KNOTS ( 'NONE', 3,
 ( #24426, #13505, #13727, #13277 ),
 .UNSPECIFIED., .F., .F.,
 ( 4, 4 ),
 ( 0.000000000000000000, 0.0001702050758941620089 ),
 .UNSPECIFIED. ) ;
#14313 = CARTESIAN_POINT ( 'NONE',  ( 125.5597614775786326, -1.561330072975669392, -17.79121239304076951 ) ) ;
#14314 = CARTESIAN_POINT ( 'NONE',  ( 122.9503348109119827, 0.5811942927096110934, -14.16772938898807510 ) ) ;
#14315 = VECTOR ( 'NONE', #35685, 1000.000000000000000 ) ;
#14316 = CARTESIAN_POINT ( 'NONE',  ( 114.9970202545248412, -10.62599879583958717, -15.77991374673208469 ) ) ;
#14317 = CARTESIAN_POINT ( 'NONE',  ( 115.1220548109119761, -1.833838273342658809, -17.42832698103878286 ) ) ;
#14318 = CARTESIAN_POINT ( 'NONE',  ( 60.53937939559665438, -4.256997083809236138, -17.89321520033831447 ) ) ;
#14319 = ORIENTED_EDGE ( 'NONE', *, *, #44180, .F. ) ;
#14320 = CARTESIAN_POINT ( 'NONE',  ( 122.3830681442452857, -8.166667518702819706, -8.995218007635861213 ) ) ;
#14321 = AXIS2_PLACEMENT_3D ( 'NONE', #29128, #36628, #32755 ) ;
#14322 = CARTESIAN_POINT ( 'NONE',  ( 119.8129079359119942, -5.444069387712269226, -19.60292469916370450 ) ) ;
#14323 = CARTESIAN_POINT ( 'NONE',  ( 118.6958348109119754, -6.344957434206665248, -7.627207830600338134 ) ) ;
#14324 = ORIENTED_EDGE ( 'NONE', *, *, #27018, .F. ) ;
#14325 = CARTESIAN_POINT ( 'NONE',  ( 106.2459265045248173, -2.791137627527939813, -8.388885654883777576 ) ) ;
#14326 = CARTESIAN_POINT ( 'NONE',  ( 124.3685014775786328, -10.63000616557722466, -14.87417383870573495 ) ) ;
#14327 = ADVANCED_FACE ( 'NONE', ( #23141 ), #5791, .T. ) ;
#14328 = CARTESIAN_POINT ( 'NONE',  ( 62.55594166779781773, -34.86283735444163767, -5.893215200338315363 ) ) ;
#14329 = CARTESIAN_POINT ( 'NONE',  ( 115.2922348109119781, 0.4262465694468514643, -12.03445270309931736 ) ) ;
#14330 = CARTESIAN_POINT ( 'NONE',  ( 120.5887993777725029, -1.267766418764730840, -16.93314635290706605 ) ) ;
#14331 = CARTESIAN_POINT ( 'NONE',  ( 121.3619881442452879, -5.574606645277164318, -18.38911715685844683 ) ) ;
#14332 = CARTESIAN_POINT ( 'NONE',  ( 120.3296260002550895, -2.334846009198419559, -18.01015021110789505 ) ) ;
#14333 = CARTESIAN_POINT ( 'NONE',  ( 122.8936081442453059, -9.565557343593413364, -10.61323700422348004 ) ) ;
#14334 = CARTESIAN_POINT ( 'NONE',  ( 124.9063227527182534, -11.00801412892373854, -8.806701716868159835 ) ) ;
#14335 = CARTESIAN_POINT ( 'NONE',  ( 119.0361948109119652, -2.084020599724406786, -8.691656652584148546 ) ) ;
#14336 = CARTESIAN_POINT ( 'NONE',  ( 123.9800954359119771, -11.07370829466463569, -12.81314460846529002 ) ) ;
#14337 = CARTESIAN_POINT ( 'NONE',  ( 116.0864081442453113, -9.988377603198976828, -10.36322818467138340 ) ) ;
#14338 = DIRECTION ( 'NONE',  ( -0.3445294493088594256, -0.9387755102040817867, 0.000000000000000000 ) ) ;
#14339 = CARTESIAN_POINT ( 'NONE',  ( 119.1496481442453046, -6.222761293078241884, -8.102969835052219238 ) ) ;
#14340 = EDGE_LOOP ( 'NONE', ( #37810, #26958, #29429, #7958 ) ) ;
#14341 = CARTESIAN_POINT ( 'NONE',  ( 118.2420214775786320, -3.383040157471821630, -19.15922257007629170 ) ) ;
#14342 = CARTESIAN_POINT ( 'NONE',  ( 115.2053796295247849, -4.863998795839590272, -8.388885654883775800 ) ) ;
#14343 = VECTOR ( 'NONE', #44371, 1000.000000000000114 ) ;
#14344 = DIRECTION ( 'NONE',  ( -0.000000000000000000, -0.9284778069183718952, -0.3713878862591649677 ) ) ;
#14345 = DIRECTION ( 'NONE',  ( 0.9609149988134837450, -0.1028163501681639419, 0.2570431154366518145 ) ) ;
#14346 = DIRECTION ( 'NONE',  ( -0.2768435750659253847, -0.3568721902840677473, 0.8921882507333133150 ) ) ;
#14347 = CARTESIAN_POINT ( 'NONE',  ( 123.8579614775786126, 0.5811942927096110934, -14.16772938898807510 ) ) ;
#14348 = ORIENTED_EDGE ( 'NONE', *, *, #37558, .F. ) ;
#14349 = CARTESIAN_POINT ( 'NONE',  ( 126.5125895482207312, -8.445584708276319574, -9.696654088380508796 ) ) ;
#14350 = CARTESIAN_POINT ( 'NONE',  ( 120.5678148109119832, -1.833838273342659253, -17.42832698103878286 ) ) ;
#14351 = CARTESIAN_POINT ( 'NONE',  ( 115.6432824739652148, 0.3208234527006404435, -15.99825685930877661 ) ) ;
#14352 = CARTESIAN_POINT ( 'NONE',  ( 109.2294421295247844, -1.388378309844742642, -16.99368411936019641 ) ) ;
#14353 = COLOUR_RGB ( '',0.7921568627450980005, 0.8196078431372548767, 0.9333333333333333481 ) ;
#14354 = CARTESIAN_POINT ( 'NONE',  ( 120.4952766009169238, -8.403782945130243931, -17.37684090985457885 ) ) ;
#14355 = CARTESIAN_POINT ( 'NONE',  ( 113.3995983795247895, -8.402594152722688392, -16.93181055722141792 ) ) ;
#14356 = DIRECTION ( 'NONE',  ( -0.9908103287288504424, 0.1352586133457950590, 0.000000000000000000 ) ) ;
#14357 = ORIENTED_EDGE ( 'NONE', *, *, #18088, .F. ) ;
#14358 = CARTESIAN_POINT ( 'NONE',  ( 113.7038881442453402, -3.383040157471821630, -19.15922257007629170 ) ) ;
#14359 = CARTESIAN_POINT ( 'NONE',  ( 124.8223148109119762, -10.15424416112533912, -14.75197769757731336 ) ) ;
#14360 = CARTESIAN_POINT ( 'NONE',  ( 122.0427081442452817, 0.5811942927096110934, -14.16772938898807510 ) ) ;
#14361 = CARTESIAN_POINT ( 'NONE',  ( 117.0507614775786465, 0.1319031606808879209, -14.10382304977623669 ) ) ;
#14362 = DIRECTION ( 'NONE',  ( -0.8636456077245080465, 0.5040994586965603652, 0.000000000000000000 ) ) ;
#14363 = CARTESIAN_POINT ( 'NONE',  ( 123.1772414775786189, -4.089484607189486809, -7.948022111789456723 ) ) ;
#14364 = CARTESIAN_POINT ( 'NONE',  ( 111.7289948109120132, -2.109465145232937378, -8.734689011829464889 ) ) ;
#14365 = CARTESIAN_POINT ( 'NONE',  ( 76.69189222814998175, -49.76310523276720232, -7.393215200338315363 ) ) ;
#14366 = CARTESIAN_POINT ( 'NONE',  ( 116.8928740015602870, 0.2848729546123598966, -14.64321520033831447 ) ) ;
#14367 = CARTESIAN_POINT ( 'NONE',  ( 124.9924948109119924, -5.574606645277164318, -18.38911715685844683 ) ) ;
#14368 = ORIENTED_EDGE ( 'NONE', *, *, #40911, .F. ) ;
#14369 = CARTESIAN_POINT ( 'NONE',  ( 116.5966151941218811, -9.866217395151686276, -13.41088139521056988 ) ) ;
#14370 = AXIS2_PLACEMENT_3D ( 'NONE', #42699, #36509, #4605 ) ;
#14371 = CARTESIAN_POINT ( 'NONE',  ( 120.2274548109119934, 0.5811942927096110934, -14.16772938898807510 ) ) ;
#14372 = CARTESIAN_POINT ( 'NONE',  ( 123.5743281442453139, -2.084020599724406786, -8.691656652584148546 ) ) ;
#14373 = EDGE_LOOP ( 'NONE', ( #33181, #24198, #27696, #39281, #26711 ) ) ;
#14374 = CARTESIAN_POINT ( 'NONE',  ( 137.0596819398274135, 0.02950868989288273417, -11.06250843582902732 ) ) ;
#14375 = CARTESIAN_POINT ( 'NONE',  ( 120.6812681442452941, -10.30919188438810075, -12.61870101168855918 ) ) ;
#14376 = CARTESIAN_POINT ( 'NONE',  ( 110.0658483795247804, -0.7896495226426338832, -9.318865927141430916 ) ) ;
#14377 = CARTESIAN_POINT ( 'NONE',  ( 118.4689281442453392, -10.15424416112533912, -14.75197769757731336 ) ) ;
#14378 = VERTEX_POINT ( 'NONE', #36345 ) ;
#14379 = CARTESIAN_POINT ( 'NONE',  ( 114.8384214775786489, 0.9020085738987339008, -11.91225656197089222 ) ) ;
#14380 = CARTESIAN_POINT ( 'NONE',  ( 117.2294421295248270, 0.7813447578650477565, -4.949553853523854130 ) ) ;
#14381 = CARTESIAN_POINT ( 'NONE',  ( 79.70219085298357697, 5.112903692279886947, -20.02675517807873362 ) ) ;
#14382 = CIRCLE ( 'NONE', #6388, 7.132259260909282084 ) ;
#14383 = LINE ( 'NONE', #10749, #2471 ) ;
#14384 = CARTESIAN_POINT ( 'NONE',  ( 125.7866681442452688, -0.4660016031367893996, -10.09054647747474043 ) ) ;
#14385 = FACE_OUTER_BOUND ( 'NONE', #24266, .T. ) ;
#14386 = CARTESIAN_POINT ( 'NONE',  ( 88.22708560785949317, -3.622631779710408395, -8.143215200338314474 ) ) ;
#14387 = CARTESIAN_POINT ( 'NONE',  ( 125.1059481442452750, -8.166667518702819706, -8.995218007635861213 ) ) ;
#14389 = CARTESIAN_POINT ( 'NONE',  ( 121.5888948109119809, 0.1319031606808879209, -14.10382304977623669 ) ) ;
#14388 = CARTESIAN_POINT ( 'NONE',  ( 122.8936081442453059, 0.2603800115204892296, -16.42320221600525088 ) ) ;
#14390 = CARTESIAN_POINT ( 'NONE',  ( 120.4543614775786295, -5.574606645277164318, -18.38911715685844683 ) ) ;
#14391 = LINE ( 'NONE', #38540, #21097 ) ;
#14392 = CARTESIAN_POINT ( 'NONE',  ( 116.7104014775786425, -0.4660016031367893996, -10.09054647747474043 ) ) ;
#14393 = ADVANCED_FACE ( 'NONE', ( #19033 ), #1696, .F. ) ;
#14394 = ORIENTED_EDGE ( 'NONE', *, *, #31902, .F. ) ;
#14395 = CARTESIAN_POINT ( 'NONE',  ( 122.6710448144346657, -2.280480477428469488, -18.08254604495227014 ) ) ;
#14396 = CARTESIAN_POINT ( 'NONE',  ( 125.4584548109119737, -6.456500312860584678, -19.12873567962219568 ) ) ;
#14397 = CARTESIAN_POINT ( 'NONE',  ( 112.6356140045247827, 0.1403307496149616695, -15.46607636864997204 ) ) ;
#14398 = CARTESIAN_POINT ( 'NONE',  ( 109.8574890045247940, -9.868328341294098749, -11.32035403202665869 ) ) ;
#14399 = CARTESIAN_POINT ( 'NONE',  ( 115.4137390045248566, -9.868328341294098749, -11.32035403202665869 ) ) ;
#14400 = CIRCLE ( 'NONE', #27506, 2.000000000000000444 ) ;
#14401 = FACE_OUTER_BOUND ( 'NONE', #22973, .T. ) ;
#14402 = CARTESIAN_POINT ( 'NONE',  ( 126.5241148109119393, -9.565557343593413364, -10.61323700422348004 ) ) ;
#14403 = VERTEX_POINT ( 'NONE', #40006 ) ;
#14404 = CARTESIAN_POINT ( 'NONE',  ( 113.3635281442453504, -0.1624402480850797581, -16.17319339645315424 ) ) ;
#14405 = CARTESIAN_POINT ( 'NONE',  ( 111.8021765045248372, -7.250697342233347165, -19.15521520033831138 ) ) ;
#14406 = CARTESIAN_POINT ( 'NONE',  ( 122.3620835773848654, -2.467220198592777969, -17.83387418641524391 ) ) ;
#14407 = CARTESIAN_POINT ( 'NONE',  ( 122.7801548109119665, -3.383040157471821630, -19.15922257007629170 ) ) ;
#14408 = CARTESIAN_POINT ( 'NONE',  ( 123.2906948109119867, -8.166667518702819706, -8.995218007635861213 ) ) ;
#14409 = CARTESIAN_POINT ( 'NONE',  ( 79.09431155867233088, 4.843896131125965177, -5.812420978032302621 ) ) ;
#14410 = CARTESIAN_POINT ( 'NONE',  ( 117.0507614775786465, -10.30919188438810075, -12.61870101168855918 ) ) ;
#14411 = CARTESIAN_POINT ( 'NONE',  ( 115.7610046295247912, -4.863998795839590272, -7.631215200338315796 ) ) ;
#14412 = CARTESIAN_POINT ( 'NONE',  ( 112.7745202545247878, 0.1403307496149616695, -11.32035403202665336 ) ) ;
#14413 = ORIENTED_EDGE ( 'NONE', *, *, #17762, .T. ) ;
#14414 = CARTESIAN_POINT ( 'NONE',  ( 126.3509913982132105, -7.545821528410036727, -9.094723512232105733 ) ) ;
#14415 = CARTESIAN_POINT ( 'NONE',  ( 117.1074881442453233, 0.4262465694468514643, -12.03445270309931736 ) ) ;
#14416 = CARTESIAN_POINT ( 'NONE',  ( 111.7751814775786556, -7.893985811506177619, -18.51759400769804742 ) ) ;
#14417 = CARTESIAN_POINT ( 'NONE',  ( 114.4413952545248350, 0.8980012041604421569, -11.00651665394454071 ) ) ;
#14418 = CARTESIAN_POINT ( 'NONE',  ( 3.060777270043529619, -5.064559853354640317, -19.39321520033831447 ) ) ;
#14419 = DIRECTION ( 'NONE',  ( 1.000000000000000000, 0.000000000000000000, -0.000000000000000000 ) ) ;
#14420 = CARTESIAN_POINT ( 'NONE',  ( 118.4122014775786340, -9.859900752359374465, -12.68260735090039404 ) ) ;
#14421 = CARTESIAN_POINT ( 'NONE',  ( 112.5126281442453120, 0.1319031606808879209, -14.10382304977623669 ) ) ;
#14422 = ORIENTED_EDGE ( 'NONE', *, *, #13758, .T. ) ;
#14423 = EDGE_CURVE ( 'NONE', #37456, #26292, #18303, .T. ) ;
#14424 = DIRECTION ( 'NONE',  ( -0.9908103287288504424, 0.1352586133457950590, 0.000000000000000000 ) ) ;
#14425 = CARTESIAN_POINT ( 'NONE',  ( 125.6164881442453094, -9.565557343593413364, -10.61323700422348004 ) ) ;
#14426 = CARTESIAN_POINT ( 'NONE',  ( 114.3846081442453197, 0.4262465694468514643, -12.03445270309931736 ) ) ;
#14427 = ORIENTED_EDGE ( 'NONE', *, *, #33918, .F. ) ;
#14428 = CARTESIAN_POINT ( 'NONE',  ( 126.2940345447972277, -9.080993302305092385, -16.14937674896652098 ) ) ;
#14429 = ADVANCED_FACE ( 'NONE', ( #87 ), #41608, .T. ) ;
#14430 = CARTESIAN_POINT ( 'NONE',  ( 112.8529881442453302, -1.561330072975668060, -17.79121239304076596 ) ) ;
#14431 = EDGE_CURVE ( 'NONE', #14958, #32925, #6659, .T. ) ;
#14432 = CARTESIAN_POINT ( 'NONE',  ( 108.6767858795247861, -8.402594152722688392, -9.854619843455216355 ) ) ;
#14433 = CARTESIAN_POINT ( 'NONE',  ( 125.0492214775786266, -3.505236298600246325, -18.68346056562440793 ) ) ;
#14434 = VERTEX_POINT ( 'NONE', #14000 ) ;
#14435 = CARTESIAN_POINT ( 'NONE',  ( 116.8805814775786445, -3.505236298600246325, -18.68346056562440793 ) ) ;
#14436 = CIRCLE ( 'NONE', #21005, 2.541999999999999371 ) ;
#14437 = CARTESIAN_POINT ( 'NONE',  ( 112.6828081442453282, -2.084020599724406786, -8.691656652584148546 ) ) ;
#14438 = CARTESIAN_POINT ( 'NONE',  ( 124.5950401870421445, -9.726016666192203175, -14.57860129224645540 ) ) ;
#14439 = CARTESIAN_POINT ( 'NONE',  ( 121.2019704359119743, 1.345710702986147034, -13.97328579221134426 ) ) ;
#14440 = ORIENTED_EDGE ( 'NONE', *, *, #30730, .T. ) ;
#14441 = LINE ( 'NONE', #10802, #33936 ) ;
#14442 = CARTESIAN_POINT ( 'NONE',  ( 124.3741441133359160, 0.01270242874617801519, -7.107006293821772402 ) ) ;
#14443 = CARTESIAN_POINT ( 'NONE',  ( 109.5102233795247884, -8.938348069036489818, -17.46756447353520159 ) ) ;
#14444 = CARTESIAN_POINT ( 'NONE',  ( 112.9664414775786412, 0.5811942927096154232, -14.16772938898807155 ) ) ;
#14445 = EDGE_CURVE ( 'NONE', #40322, #32536, #39664, .T. ) ;
#14446 = CARTESIAN_POINT ( 'NONE',  ( 125.3328548109119964, -0.8288870151387760510, -10.36305467784173118 ) ) ;
#14447 =( BOUNDED_CURVE ( )  B_SPLINE_CURVE ( 3, ( #1067, #38909, #7911, #18174 ),
 .UNSPECIFIED., .F., .F. ) 
 B_SPLINE_CURVE_WITH_KNOTS ( ( 4, 4 ),
 ( 0.9676049211852268961, 1.570796326794895004 ),
 .UNSPECIFIED. ) 
 CURVE ( )  GEOMETRIC_REPRESENTATION_ITEM ( )  RATIONAL_B_SPLINE_CURVE ( ( 1.000000000000000000, 0.9699091404214869039, 0.9699091404214869039, 1.000000000000000000 ) ) 
 REPRESENTATION_ITEM ( '' )  );
#14448 = CARTESIAN_POINT ( 'NONE',  ( 118.9794681442453026, -0.8288870151387760510, -10.36305467784173118 ) ) ;
#14449 = FACE_OUTER_BOUND ( 'NONE', #24712, .T. ) ;
#14450 = EDGE_CURVE ( 'NONE', #3542, #33593, #17588, .T. ) ;
#14451 = VERTEX_POINT ( 'NONE', #44799 ) ;
#14452 = CARTESIAN_POINT ( 'NONE',  ( 116.1431348109119881, 0.1319031606808879209, -14.10382304977623669 ) ) ;
#14453 = LINE ( 'NONE', #35852, #1498 ) ;
#14454 = CARTESIAN_POINT ( 'NONE',  ( 86.07942216836008242, -27.04188231690493538, -8.497324495144606971 ) ) ;
#14455 = CARTESIAN_POINT ( 'NONE',  ( 83.75466360696344736, -7.807702403958562520, -9.893215200338316251 ) ) ;
#14456 = CARTESIAN_POINT ( 'NONE',  ( 113.3635281442453504, -9.988377603198976828, -10.36322818467138340 ) ) ;
#14457 = ORIENTED_EDGE ( 'NONE', *, *, #45139, .F. ) ;
#14458 = CARTESIAN_POINT ( 'NONE',  ( 118.8092881442453290, -9.988377603198976828, -10.36322818467138340 ) ) ;
#14459 = LINE ( 'NONE', #25175, #30543 ) ;
#14460 = CARTESIAN_POINT ( 'NONE',  ( 113.1217858795247935, -0.7896495226426338832, -17.46756447353520159 ) ) ;
#14461 = CARTESIAN_POINT ( 'NONE',  ( 113.6471614775786492, -5.638512984488999180, -18.83840828888717311 ) ) ;
#14462 = CARTESIAN_POINT ( 'NONE',  ( 115.0086014775786509, -4.089484607189486809, -7.948022111789456723 ) ) ;
#14463 = PLANE ( 'NONE',  #41749 ) ;
#14464 = CARTESIAN_POINT ( 'NONE',  ( 84.10862215250544693, -25.99489077589524300, -13.39321520033831625 ) ) ;
#14465 = CARTESIAN_POINT ( 'NONE',  ( 110.2742077545248094, -2.791137627527939813, -18.39754474579286025 ) ) ;
#14466 = ORIENTED_EDGE ( 'NONE', *, *, #28469, .F. ) ;
#14467 = CARTESIAN_POINT ( 'NONE',  ( 112.0827276054816366, -2.287189184988692947, -18.07361239780447448 ) ) ;
#14468 = CARTESIAN_POINT ( 'NONE',  ( 109.2294421130689130, -4.116351054653907049, -18.49425727697660804 ) ) ;
#14469 = CARTESIAN_POINT ( 'NONE',  ( 117.5613014775786525, -10.15424416112533912, -14.75197769757731336 ) ) ;
#14470 = CARTESIAN_POINT ( 'NONE',  ( 75.95778847736514194, -3.256761025687008537, -12.39321520033831447 ) ) ;
#14471 = CARTESIAN_POINT ( 'NONE',  ( 122.4040527111058339, -1.267766418764731728, -16.93314635290706605 ) ) ;
#14472 = CARTESIAN_POINT ( 'NONE',  ( 111.7327233795247849, -8.938348069036489818, -17.46756447353520159 ) ) ;
#14473 = DIRECTION ( 'NONE',  ( 1.000000000000000000, 0.000000000000000000, -0.000000000000000000 ) ) ;
#14474 = CARTESIAN_POINT ( 'NONE',  ( 125.0492214775786266, -6.344957434206665248, -7.627207830600338134 ) ) ;
#14475 = CARTESIAN_POINT ( 'NONE',  ( 120.2841814775786276, -10.15424416112534622, -14.75197769757730448 ) ) ;
#14476 = CARTESIAN_POINT ( 'NONE',  ( 125.5597614775786326, -1.561330072975669392, -17.79121239304076951 ) ) ;
#14477 = CARTESIAN_POINT ( 'NONE',  ( 114.8951481442453115, -0.4660016031367893996, -10.09054647747474043 ) ) ;
#14478 = ORIENTED_EDGE ( 'NONE', *, *, #19256, .F. ) ;
#14479 = CARTESIAN_POINT ( 'NONE',  ( 113.6471614775786492, -4.153390946401321671, -8.397313243818183892 ) ) ;
#14480 = DIRECTION ( 'NONE',  ( 0.000000000000000000, 0.000000000000000000, 1.000000000000000000 ) ) ;
#14481 = CARTESIAN_POINT ( 'NONE',  ( 116.2565881442452991, -9.261995988541697145, -16.69588392320189030 ) ) ;
#14482 = CARTESIAN_POINT ( 'NONE',  ( 114.6682414775786469, -7.894159318335828068, -9.358103419637847864 ) ) ;
#14483 = ORIENTED_EDGE ( 'NONE', *, *, #24720, .T. ) ;
#14484 = CARTESIAN_POINT ( 'NONE',  ( 121.8158014775786171, -4.153390946401325223, -8.397313243818185668 ) ) ;
#14485 = EDGE_CURVE ( 'NONE', #25316, #38354, #33067, .T. ) ;
#14486 = CARTESIAN_POINT ( 'NONE',  ( 115.0653281442453277, -6.344957434206662583, -7.627207830600332805 ) ) ;
#14487 = CARTESIAN_POINT ( 'NONE',  ( 137.2645862585842451, 0.3856499210305354142, -13.29373647331895114 ) ) ;
#14488 = CARTESIAN_POINT ( 'NONE',  ( 108.1906140045248463, -10.62599879583958717, -11.00651665394454604 ) ) ;
#14489 = CARTESIAN_POINT ( 'NONE',  ( 114.4526169549021830, -1.135392229370321582, -17.10942237759953954 ) ) ;
#14490 = CARTESIAN_POINT ( 'NONE',  ( 127.1470196510598782, 0.5883225706286522305, -13.03016238292672213 ) ) ;
#14491 = CARTESIAN_POINT ( 'NONE',  ( 76.69189222814998175, -46.76310523276723785, -6.893215200338315363 ) ) ;
#14492 = CARTESIAN_POINT ( 'NONE',  ( 114.6682414775786469, -1.561330072975668060, -17.79121239304076596 ) ) ;
#14493 = AXIS2_PLACEMENT_3D ( 'NONE', #43925, #29109, #43476 ) ;
#14494 = CYLINDRICAL_SURFACE ( 'NONE', #14966, 8.000000000000001776 ) ;
#14495 = CARTESIAN_POINT ( 'NONE',  ( 115.2355081442453155, 0.1319031606808879209, -14.10382304977623669 ) ) ;
#14496 = CARTESIAN_POINT ( 'NONE',  ( 87.68939540009954214, -25.99489077589524300, -13.39321520033831447 ) ) ;
#14497 = EDGE_CURVE ( 'NONE', #34165, #10687, #2276, .T. ) ;
#14498 = CARTESIAN_POINT ( 'NONE',  ( 112.7491510812576934, -0.01829820670803256055, -12.14321520033831625 ) ) ;
#14499 = CARTESIAN_POINT ( 'NONE',  ( 115.7610046295247912, -4.863998795839590272, -18.39754474579285315 ) ) ;
#14500 = CARTESIAN_POINT ( 'NONE',  ( 113.1366214775786432, -7.643976991954077427, -18.09477374809248928 ) ) ;
#14501 = EDGE_CURVE ( 'NONE', #34659, #40637, #37759, .T. ) ;
#14502 = DIRECTION ( 'NONE',  ( 9.108669703179767173E-16, 0.7876185884367603585, -0.6161630946014904353 ) ) ;
#14504 = CARTESIAN_POINT ( 'NONE',  ( 118.8092881442453290, -9.988377603198976828, -10.36322818467138340 ) ) ;
#14503 = CARTESIAN_POINT ( 'NONE',  ( 118.6958348109119754, -6.344957434206651037, -7.627207830600339911 ) ) ;
#14505 = CARTESIAN_POINT ( 'NONE',  ( 124.7088614775786226, -9.565557343593413364, -10.61323700422348004 ) ) ;
#14506 = CARTESIAN_POINT ( 'NONE',  ( 118.6391081442452986, -5.574606645277164318, -18.38911715685844683 ) ) ;
#14507 = CARTESIAN_POINT ( 'NONE',  ( 125.6164881442453094, 0.2603800115204892296, -16.42320221600525088 ) ) ;
#14508 = VERTEX_POINT ( 'NONE', #30429 ) ;
#14509 = CARTESIAN_POINT ( 'NONE',  ( 137.2865145795256865, -8.609599717022557996, -9.742863212004273521 ) ) ;
#14510 = EDGE_CURVE ( 'NONE', #16083, #3126, #21946, .T. ) ;
#14511 = CARTESIAN_POINT ( 'NONE',  ( 121.2485348109119769, -0.4660016031367893996, -10.09054647747474043 ) ) ;
#14512 = CARTESIAN_POINT ( 'NONE',  ( 115.2748327545248657, -6.936859964151250502, -8.388885654883777576 ) ) ;
#14513 = CARTESIAN_POINT ( 'NONE',  ( 118.4122014775786340, -9.859900752359374465, -12.68260735090039404 ) ) ;
#14514 = CARTESIAN_POINT ( 'NONE',  ( 126.1837548109119211, -10.63000616557722466, -14.87417383870573495 ) ) ;
#14515 = DIRECTION ( 'NONE',  ( 0.9609149988134843001, -0.1028163501681632064, 0.2570431154366505933 ) ) ;
#14516 = CARTESIAN_POINT ( 'NONE',  ( 114.9970202545248412, -10.62599879583958717, -15.77991374673208469 ) ) ;
#14517 = CARTESIAN_POINT ( 'NONE',  ( 119.7169148109119874, -0.1624402480850797581, -16.17319339645315424 ) ) ;
#14518 = CARTESIAN_POINT ( 'NONE',  ( 124.0848681442452772, -5.574606645277164318, -18.38911715685844683 ) ) ;
#14519 = CARTESIAN_POINT ( 'NONE',  ( 115.9947331777918862, -0.01829820670803256055, -14.64321520033831447 ) ) ;
#14520 = CARTESIAN_POINT ( 'NONE',  ( 109.2294422733754828, -3.494069591452107382, -8.049094117091842193 ) ) ;
#14521 = CARTESIAN_POINT ( 'NONE',  ( 122.1048610609119720, -3.163656168406935087, -18.89861972220014508 ) ) ;
#14522 = CARTESIAN_POINT ( 'NONE',  ( 113.8857702545248003, -10.62599879583958717, -15.77991374673208469 ) ) ;
#14523 = CARTESIAN_POINT ( 'NONE',  ( 122.4040527111058339, -1.267766418764731728, -16.93314635290706605 ) ) ;
#14524 = CARTESIAN_POINT ( 'NONE',  ( 115.7460481442453357, 0.9020085738987339008, -11.91225656197089222 ) ) ;
#14525 = CARTESIAN_POINT ( 'NONE',  ( 113.6471614775786492, -5.638512984488999180, -18.83840828888717311 ) ) ;
#14526 = CARTESIAN_POINT ( 'NONE',  ( 113.1912390045248031, 0.8980012041604421569, -15.77991374673208469 ) ) ;
#14527 = CARTESIAN_POINT ( 'NONE',  ( 111.9453614775786434, -1.561330072975668060, -17.79121239304076596 ) ) ;
#14528 = ORIENTED_EDGE ( 'NONE', *, *, #23091, .F. ) ;
#14529 = CARTESIAN_POINT ( 'NONE',  ( 113.1314091344827659, -1.149058757900096595, -17.09122335155389649 ) ) ;
#14530 = CARTESIAN_POINT ( 'NONE',  ( 124.2550481442452792, -9.988377603198980381, -10.36322818467138518 ) ) ;
#14531 = CARTESIAN_POINT ( 'NONE',  ( 117.1074881442453233, -10.63000616557722466, -14.87417383870573495 ) ) ;
#14532 = VECTOR ( 'NONE', #35656, 1000.000000000000114 ) ;
#14533 = CARTESIAN_POINT ( 'NONE',  ( 123.0070614775786169, -10.15424416112533912, -14.75197769757731336 ) ) ;
#14534 =( LENGTH_UNIT ( ) NAMED_UNIT ( * ) SI_UNIT ( .MILLI., .METRE. ) );
#14535 = CARTESIAN_POINT ( 'NONE',  ( 112.1722681442453222, -8.899110576539710493, -16.42337572283490132 ) ) ;
#14536 = CARTESIAN_POINT ( 'NONE',  ( 120.9649014775786355, -3.383040157471821630, -19.15922257007629170 ) ) ;
#14537 = CARTESIAN_POINT ( 'NONE',  ( 112.6356140045247827, -10.62599879583958717, -11.00651665394454604 ) ) ;
#14538 = CARTESIAN_POINT ( 'NONE',  ( 115.8027748109119841, -8.899110576539710493, -16.42337572283490132 ) ) ;
#14539 = DIRECTION ( 'NONE',  ( 1.000000000000000000, 0.000000000000000000, -0.000000000000000000 ) ) ;
#14540 = ORIENTED_EDGE ( 'NONE', *, *, #27375, .F. ) ;
#14541 = CARTESIAN_POINT ( 'NONE',  ( 123.1772414775786189, -4.089484607189486809, -7.948022111789456723 ) ) ;
#14542 = EDGE_CURVE ( 'NONE', #16121, #25152, #1561, .T. ) ;
#14543 = CARTESIAN_POINT ( 'NONE',  ( 121.6881423109119709, -9.959231468620755479, -10.70263013195267199 ) ) ;
#14544 = CARTESIAN_POINT ( 'NONE',  ( 118.5256548109119876, -0.4660016031367893996, -10.09054647747474043 ) ) ;
#14545 = ORIENTED_EDGE ( 'NONE', *, *, #12048, .F. ) ;
#14546 = CARTESIAN_POINT ( 'NONE',  ( 107.4266296295248821, -4.863998795839590272, -8.388885654883775800 ) ) ;
#14547 = CARTESIAN_POINT ( 'NONE',  ( -13.43406623181752124, -4.955740180368149339, -8.622168566727538064 ) ) ;
#14548 = CARTESIAN_POINT ( 'NONE',  ( 122.4965214775786251, -10.30919188438810075, -12.61870101168855918 ) ) ;
#14549 = CARTESIAN_POINT ( 'NONE',  ( 115.6893214775786447, -9.859900752359374465, -12.68260735090039404 ) ) ;
#14550 = CARTESIAN_POINT ( 'NONE',  ( 71.02242295334774269, -58.04588819712443382, -39.52596974311911993 ) ) ;
#14551 = CARTESIAN_POINT ( 'NONE',  ( 121.2485348109119769, -8.899110576539710493, -16.42337572283490132 ) ) ;
#14552 = CARTESIAN_POINT ( 'NONE',  ( -1.145390592550948883, -14.88589425535891841, -19.39321520033831447 ) ) ;
#14553 = CARTESIAN_POINT ( 'NONE',  ( 120.3976348109119812, -7.643976991954077427, -18.09477374809248928 ) ) ;
#14554 = EDGE_CURVE ( 'NONE', #39376, #6119, #22687, .T. ) ;
#14555 = CIRCLE ( 'NONE', #40847, 2.000000000000000444 ) ;
#14556 = CARTESIAN_POINT ( 'NONE',  ( 125.1589444732352234, -10.92313641483920250, -9.146039627217522394 ) ) ;
#14557 = CARTESIAN_POINT ( 'NONE',  ( 118.2420214775786320, -6.222761293078241884, -8.102969835052219238 ) ) ;
#14558 = CARTESIAN_POINT ( 'NONE',  ( 113.1366214775786432, -1.834011780172310813, -8.268836392978581529 ) ) ;
#14559 = CARTESIAN_POINT ( 'NONE',  ( 118.5823814775786360, -1.834011780172310813, -8.268836392978581529 ) ) ;
#14560 = CARTESIAN_POINT ( 'NONE',  ( 125.3328548109119964, -0.8288870151387760510, -10.36305467784173118 ) ) ;
#14561 = CARTESIAN_POINT ( 'NONE',  ( 128.2184548109119930, -7.067465109756605912, -7.812468278694988832 ) ) ;
#14562 = CARTESIAN_POINT ( 'NONE',  ( 120.6812681442452941, 0.1319031606808879209, -14.10382304977623669 ) ) ;
#14563 = ORIENTED_EDGE ( 'NONE', *, *, #28153, .F. ) ;
#14564 = CARTESIAN_POINT ( 'NONE',  ( 117.8449348109119938, -8.166667518702817929, -8.995218007635861213 ) ) ;
#14565 = CARTESIAN_POINT ( 'NONE',  ( 115.0664733795247798, -1.325403438956436419, -9.854619843455211026 ) ) ;
#14566 = DIRECTION ( 'NONE',  ( 0.000000000000000000, -0.3818493186865936084, 0.9242245927363024194 ) ) ;
#14567 = CARTESIAN_POINT ( 'NONE',  ( 114.8834831777918879, -0.01829820670803256055, -14.64321520033831447 ) ) ;
#14568 = CIRCLE ( 'NONE', #31321, 2.000000000000000444 ) ;
#14569 = CARTESIAN_POINT ( 'NONE',  ( 127.8631586617352838, -4.391174868859571312, -15.27166827963823614 ) ) ;
#14570 = CARTESIAN_POINT ( 'NONE',  ( 122.6099748109119929, -9.261995988541697145, -16.69588392320189030 ) ) ;
#14571 = ORIENTED_EDGE ( 'NONE', *, *, #40533, .T. ) ;
#14572 = AXIS2_PLACEMENT_3D ( 'NONE', #14491, #6985, #45067 ) ;
#14573 = CARTESIAN_POINT ( 'NONE',  ( 128.2184548109119930, -9.609004340414083245, -9.721032963308941177 ) ) ;
#14574 = CARTESIAN_POINT ( 'NONE',  ( 121.7590748109119687, -2.084020599724406786, -8.691656652584148546 ) ) ;
#14575 = DIRECTION ( 'NONE',  ( -0.000000000000000000, -0.9284778069183721172, -0.3713878862591650232 ) ) ;
#14576 = DIRECTION ( 'NONE',  ( -0.8636456077245080465, 0.5040994586965603652, 0.000000000000000000 ) ) ;
#14577 = CARTESIAN_POINT ( 'NONE',  ( 111.5588148109119828, 0.08617673920517221475, -14.09731900820172967 ) ) ;
#14578 = CARTESIAN_POINT ( 'NONE',  ( 111.3160046295247838, -4.863998795839590272, -18.39754474579285315 ) ) ;
#14579 = ORIENTED_EDGE ( 'NONE', *, *, #36467, .T. ) ;
#14580 = CARTESIAN_POINT ( 'NONE',  ( 113.5904348109119866, -7.893985811506177619, -18.51759400769804742 ) ) ;
#14581 = CARTESIAN_POINT ( 'NONE',  ( 126.3539348109119800, -4.153390946401325223, -8.397313243818185668 ) ) ;
#14582 = CARTESIAN_POINT ( 'NONE',  ( 73.01241679510815175, -68.13509210538408922, -39.58160742654554554 ) ) ;
#14583 = CARTESIAN_POINT ( 'NONE',  ( 120.6812681442452941, 0.1319031606808879209, -14.10382304977623669 ) ) ;
#14584 = DIRECTION ( 'NONE',  ( 0.000000000000000000, -0.3818493186865927203, 0.9242245927363029745 ) ) ;
#14585 = FILL_AREA_STYLE_COLOUR ( '', #16014 ) ;
#14586 = CARTESIAN_POINT ( 'NONE',  ( 121.4187148109119789, -6.344957434206665248, -7.627207830600338134 ) ) ;
#14587 = FACE_OUTER_BOUND ( 'NONE', #9914, .T. ) ;
#14588 = DIRECTION ( 'NONE',  ( -0.5040994586965589219, -0.8636456077245089347, 0.000000000000000000 ) ) ;
#14589 = CARTESIAN_POINT ( 'NONE',  ( 62.77214489637164263, -64.71164127777572617, -45.95359936387812638 ) ) ;
#14590 = CARTESIAN_POINT ( 'NONE',  ( 112.3991748109119868, -8.166667518702817929, -8.995218007635859436 ) ) ;
#14591 = ORIENTED_EDGE ( 'NONE', *, *, #16104, .T. ) ;
#14592 = FACE_OUTER_BOUND ( 'NONE', #7543, .T. ) ;
#14593 = CIRCLE ( 'NONE', #30644, 1.199999999999999512 ) ;
#14594 = CARTESIAN_POINT ( 'NONE',  ( 119.6034614775786196, -6.344957434206665248, -7.627207830600338134 ) ) ;
#14595 = CARTESIAN_POINT ( 'NONE',  ( 136.9012041053437088, -9.901132554421634424, -15.67648283907295159 ) ) ;
#14596 = VERTEX_POINT ( 'NONE', #3060 ) ;
#14597 = CARTESIAN_POINT ( 'NONE',  ( 112.0020881442453344, 0.2603800115204892296, -16.42320221600525088 ) ) ;
#14598 = CARTESIAN_POINT ( 'NONE',  ( 121.4187148109119789, -6.344957434206665248, -7.627207830600338134 ) ) ;
#14599 = CARTESIAN_POINT ( 'NONE',  ( 105.4819421295248247, 0.8980012041604618078, -13.39321520033831447 ) ) ;
#14600 = CARTESIAN_POINT ( 'NONE',  ( 122.0427081442452817, -9.859900752359378018, -12.68260735090039759 ) ) ;
#14601 = ORIENTED_EDGE ( 'NONE', *, *, #18077, .F. ) ;
#14602 = VECTOR ( 'NONE', #39090, 1000.000000000000000 ) ;
#14603 = CARTESIAN_POINT ( 'NONE',  ( 114.4413348109119823, -9.261995988541697145, -16.69588392320189030 ) ) ;
#14604 = CARTESIAN_POINT ( 'NONE',  ( 110.2184548109119788, -4.863998795839242995, -13.39321520033831447 ) ) ;
#14605 = AXIS2_PLACEMENT_3D ( 'NONE', #20347, #6658, #20568 ) ;
#14606 = DIRECTION ( 'NONE',  ( 0.9498278979187093629, 0.3127730236694430954, 0.000000000000000000 ) ) ;
#14607 = CARTESIAN_POINT ( 'NONE',  ( 111.4401632144035403, -2.485602189585009114, -17.80939581708303621 ) ) ;
#14608 = CARTESIAN_POINT ( 'NONE',  ( 111.8886348109120092, -6.222761293078241884, -8.102969835052219238 ) ) ;
#14609 = CARTESIAN_POINT ( 'NONE',  ( 70.19189222814998175, -57.05206236706784040, -36.02363522683400276 ) ) ;
#14610 = EDGE_CURVE ( 'NONE', #8725, #33098, #31313, .T. ) ;
#14611 = DIRECTION ( 'NONE',  ( 0.1352586133457954198, 0.9908103287288503314, 0.000000000000000000 ) ) ;
#14612 = CARTESIAN_POINT ( 'NONE',  ( 123.0637881442452937, -0.4660016031367893996, -10.09054647747474043 ) ) ;
#14614 = CARTESIAN_POINT ( 'NONE',  ( 122.7801548109119665, -6.222761293078241884, -8.102969835052219238 ) ) ;
#14613 = CARTESIAN_POINT ( 'NONE',  ( 120.9649014775786355, -3.383040157471821630, -19.15922257007629170 ) ) ;
#14615 = CARTESIAN_POINT ( 'NONE',  ( 119.0929214775786278, -4.153390946401325223, -8.397313243818185668 ) ) ;
#14616 = CARTESIAN_POINT ( 'NONE',  ( 125.4357681442453440, -2.109465145233854422, -8.734689011828928429 ) ) ;
#14617 = CARTESIAN_POINT ( 'NONE',  ( 118.7525614775786380, -8.166667518702819706, -8.995218007635861213 ) ) ;
#14618 = ORIENTED_EDGE ( 'NONE', *, *, #10088, .F. ) ;
#14619 = VERTEX_POINT ( 'NONE', #44573 ) ;
#14620 = CARTESIAN_POINT ( 'NONE',  ( 112.0991384760652920, 0.6362173239733635022, -12.14321520033831625 ) ) ;
#14621 = CARTESIAN_POINT ( 'NONE',  ( 115.4137390045248566, 0.8980012041604421569, -15.77991374673208469 ) ) ;
#14622 = CARTESIAN_POINT ( 'NONE',  ( 114.3024890045248156, -9.868328341294098749, -11.32035403202665869 ) ) ;
#14623 = CARTESIAN_POINT ( 'NONE',  ( 112.2188952545247531, -9.868328341294098749, -15.46607636864997204 ) ) ;
#14624 = VECTOR ( 'NONE', #14344, 1000.000000000000227 ) ;
#14625 = CARTESIAN_POINT ( 'NONE',  ( 125.0492214775786266, -6.344957434206665248, -7.627207830600338134 ) ) ;
#14626 = CARTESIAN_POINT ( 'NONE',  ( 125.0492214775786266, -3.505236298600246325, -18.68346056562440793 ) ) ;
#14627 = EDGE_LOOP ( 'NONE', ( #19503, #43879, #7818, #42255 ) ) ;
#14628 = CARTESIAN_POINT ( 'NONE',  ( 112.5693548109119888, 0.4262465694468514643, -12.03445270309931736 ) ) ;
#14629 = CARTESIAN_POINT ( 'NONE',  ( 108.8156921295247912, 0.8980012041604618078, -13.39321520033831447 ) ) ;
#14630 = DIRECTION ( 'NONE',  ( 0.000000000000000000, -1.000000000000000000, 0.000000000000000000 ) ) ;
#14631 = CARTESIAN_POINT ( 'NONE',  ( 119.7821199480702603, -6.365377317481695663, -18.95617363400926081 ) ) ;
#14632 = CARTESIAN_POINT ( 'NONE',  ( 125.5030348109119558, -3.383040157471821630, -19.15922257007629170 ) ) ;
#14633 = CARTESIAN_POINT ( 'NONE',  ( 63.98210704970577467, -13.60563849168870121, -18.23844916413033701 ) ) ;
#14634 = CARTESIAN_POINT ( 'NONE',  ( 114.4413348109119823, -9.261995988541697145, -16.69588392320189030 ) ) ;
#14635 = CARTESIAN_POINT ( 'NONE',  ( 114.5108483795247878, -0.7896495226426338832, -9.318865927141430916 ) ) ;
#14636 = CARTESIAN_POINT ( 'NONE',  ( 112.7050671295247923, 0.1403307496149613920, -13.39321520033831447 ) ) ;
#14637 = ORIENTED_EDGE ( 'NONE', *, *, #28259, .F. ) ;
#14638 = CARTESIAN_POINT ( 'NONE',  ( 126.9932531981167756, -7.212978846078887507, -8.544877725673300617 ) ) ;
#14639 = CIRCLE ( 'NONE', #6640, 2.000000000000000444 ) ;
#14640 = CARTESIAN_POINT ( 'NONE',  ( 115.9729548109119861, -3.505236298600246325, -18.68346056562440793 ) ) ;
#14641 = CARTESIAN_POINT ( 'NONE',  ( 113.1366214775786432, -1.834011780172310813, -8.268836392978581529 ) ) ;
#14642 = CARTESIAN_POINT ( 'NONE',  ( 113.3068014775786594, -8.166667518702817929, -8.995218007635859436 ) ) ;
#14643 = VECTOR ( 'NONE', #43327, 1000.000000000000114 ) ;
#14644 = CARTESIAN_POINT ( 'NONE',  ( 118.5823814775786502, -7.643976991954101408, -18.09477374809246797 ) ) ;
#14645 = UNCERTAINTY_MEASURE_WITH_UNIT (LENGTH_MEASURE( 1.000000000000000082E-05 ), #31677, 'distance_accuracy_value', 'NONE');
#14646 = CARTESIAN_POINT ( 'NONE',  ( 120.1140014775786398, -7.894159318335828068, -9.358103419637847864 ) ) ;
#14647 = CARTESIAN_POINT ( 'NONE',  ( 115.2922348109119781, 0.4262465694468514643, -12.03445270309931736 ) ) ;
#14648 = ORIENTED_EDGE ( 'NONE', *, *, #4136, .F. ) ;
#14649 = CARTESIAN_POINT ( 'NONE',  ( 123.7717360609119623, -3.387241619883791355, -18.17469012370385073 ) ) ;
#14650 = LINE ( 'NONE', #4602, #1099 ) ;
#14651 = CARTESIAN_POINT ( 'NONE',  ( 112.9664414775786412, -9.859900752359374465, -12.68260735090039404 ) ) ;
#14652 = ORIENTED_EDGE ( 'NONE', *, *, #6085, .F. ) ;
#14653 = CARTESIAN_POINT ( 'NONE',  ( 79.05243529145373316, 4.793396140045460108, -5.736853407927685389 ) ) ;
#14654 = CARTESIAN_POINT ( 'NONE',  ( 123.9714148109119805, -8.899110576539726480, -16.42337572283488001 ) ) ;
#14655 = CARTESIAN_POINT ( 'NONE',  ( 110.6214733795247867, -1.325403438956436419, -9.854619843455211026 ) ) ;
#14656 = CARTESIAN_POINT ( 'NONE',  ( 112.4559014775786778, -0.1624402480850797581, -16.17319339645315424 ) ) ;
#14657 = VERTEX_POINT ( 'NONE', #18621 ) ;
#14658 = EDGE_LOOP ( 'NONE', ( #29678, #5936, #43033, #1019, #3286, #25358 ) ) ;
#14659 = VECTOR ( 'NONE', #36574, 1000.000000000000000 ) ;
#14660 = CARTESIAN_POINT ( 'NONE',  ( 118.5256548109119876, -8.899110576539710493, -16.42337572283490132 ) ) ;
#14661 = CARTESIAN_POINT ( 'NONE',  ( 118.7525614775786380, -1.833838273342659253, -17.42832698103878286 ) ) ;
#14662 = CARTESIAN_POINT ( 'NONE',  ( 124.5550616865675693, -9.865623858367307264, -13.39908528032752955 ) ) ;
#14663 = CARTESIAN_POINT ( 'NONE',  ( 120.8547048109119686, -7.554583864224885481, -18.48844787311982785 ) ) ;
#14664 = VERTEX_POINT ( 'NONE', #29102 ) ;
#14665 = CARTESIAN_POINT ( 'NONE',  ( 91.77400275106518279, -26.75858941326842810, -11.54476601486570964 ) ) ;
#14666 = CARTESIAN_POINT ( 'NONE',  ( 125.3563494635854880, -1.799223464854087018, -7.045947544758777603 ) ) ;
#14667 = CARTESIAN_POINT ( 'NONE',  ( 112.7050671295247923, -10.62599879583958540, -13.39321520033831447 ) ) ;
#14668 = VECTOR ( 'NONE', #28098, 1000.000000000000000 ) ;
#14669 = CARTESIAN_POINT ( 'NONE',  ( 112.5126281442453120, -10.30919188438810075, -12.61870101168855918 ) ) ;
#14670 = PRODUCT_DEFINITION_SHAPE ( 'NONE', 'NONE',  #10357 ) ;
#14671 = CARTESIAN_POINT ( 'NONE',  ( 125.0492214775786266, -3.505236298600246325, -18.68346056562440793 ) ) ;
#14672 = CARTESIAN_POINT ( 'NONE',  ( 118.0151148109119816, 0.4262465694468514643, -12.03445270309931736 ) ) ;
#14673 = CARTESIAN_POINT ( 'NONE',  ( 27.78057335388972504, -13.48551096636548330, -8.893215200338314474 ) ) ;
#14674 = ORIENTED_EDGE ( 'NONE', *, *, #39803, .T. ) ;
#14675 = CARTESIAN_POINT ( 'NONE',  ( 117.9583881442453048, 0.1319031606808879209, -14.10382304977623669 ) ) ;
#14676 = CARTESIAN_POINT ( 'NONE',  ( 115.0664733795247798, -8.938348069036489818, -17.46756447353520159 ) ) ;
#14677 = CARTESIAN_POINT ( 'NONE',  ( 125.1653261673649524, -1.290981801452376843, -16.90223159988300594 ) ) ;
#14678 = CARTESIAN_POINT ( 'NONE',  ( 88.35093386163799778, -25.99489077589524300, -13.39321520033831447 ) ) ;
#14679 = CARTESIAN_POINT ( 'NONE',  ( 116.4267681442453153, -3.383040157471821630, -19.15922257007629170 ) ) ;
#14680 = ORIENTED_EDGE ( 'NONE', *, *, #29792, .F. ) ;
#14681 = CARTESIAN_POINT ( 'NONE',  ( 118.9227414775786400, -10.63000616557722466, -14.87417383870573495 ) ) ;
#14682 = CARTESIAN_POINT ( 'NONE',  ( 113.8280291406318838, 0.3208234527006404435, -15.99825685930877661 ) ) ;
#14683 = CARTESIAN_POINT ( 'NONE',  ( 110.8298327545248299, -2.477300249445798297, -19.15521520033831138 ) ) ;
#14684 = CARTESIAN_POINT ( 'NONE',  ( 114.8384214775786489, 0.9020085738987339008, -11.91225656197089222 ) ) ;
#14685 = CARTESIAN_POINT ( 'NONE',  ( 112.6828081442453282, -7.893985811506177619, -18.51759400769804742 ) ) ;
#14686 = CARTESIAN_POINT ( 'NONE',  ( 61.93251787845459688, -3.724979762910209935, -19.30861058678017272 ) ) ;
#14687 = ADVANCED_FACE ( 'NONE', ( #28887 ), #42153, .T. ) ;
#14688 = DIRECTION ( 'NONE',  ( 0.000000000000000000, 0.000000000000000000, -1.000000000000000000 ) ) ;
#14689 = CARTESIAN_POINT ( 'NONE',  ( 70.19189222814998175, -66.20485342690169261, -45.06987807991856698 ) ) ;
#14690 = ORIENTED_EDGE ( 'NONE', *, *, #31421, .F. ) ;
#14691 = CARTESIAN_POINT ( 'NONE',  ( 85.15861813568058380, -25.99489077589524300, -13.39321520033831625 ) ) ;
#14692 = CARTESIAN_POINT ( 'NONE',  ( 109.2294433289797126, -3.066010384757168250, -18.16908882001265368 ) ) ;
#14693 = AXIS2_PLACEMENT_3D ( 'NONE', #10735, #37862, #17135 ) ;
#14694 = CARTESIAN_POINT ( 'NONE',  ( 114.9518748109119883, -7.643976991954077427, -18.09477374809248928 ) ) ;
#14695 = CARTESIAN_POINT ( 'NONE',  ( 64.15128094833310968, -12.93337738546650861, -10.94975984855463835 ) ) ;
#14696 = CARTESIAN_POINT ( 'NONE',  ( 116.1777233795247781, -1.325403438956436419, -9.854619843455211026 ) ) ;
#14697 = CARTESIAN_POINT ( 'NONE',  ( 106.1764733795248219, -8.938348069036489818, -17.46756447353520159 ) ) ;
#14698 = DIRECTION ( 'NONE',  ( 0.000000000000000000, 0.000000000000000000, -1.000000000000000000 ) ) ;
#14699 = CARTESIAN_POINT ( 'NONE',  ( 114.4980614775786734, -2.084020599724406786, -8.691656652584148546 ) ) ;
#14700 = CARTESIAN_POINT ( 'NONE',  ( 136.2937225531903778, 0.9357610074967241953, -12.72675860691893490 ) ) ;
#14701 = CARTESIAN_POINT ( 'NONE',  ( 123.6310548109119765, -5.638512984488999180, -18.83840828888717311 ) ) ;
#14702 = CARTESIAN_POINT ( 'NONE',  ( 120.9081748109119872, -5.638512984488999180, -18.83840828888717311 ) ) ;
#14703 = VERTEX_POINT ( 'NONE', #39816 ) ;
#14704 = CARTESIAN_POINT ( 'NONE',  ( 115.5191414775786569, -6.222761293078241884, -8.102969835052219238 ) ) ;
#14705 = AXIS2_PLACEMENT_3D ( 'NONE', #37438, #9635, #6209 ) ;
#14706 = CARTESIAN_POINT ( 'NONE',  ( 61.69189222814998175, -49.76310523276723785, -19.39321520033831447 ) ) ;
#14707 = CARTESIAN_POINT ( 'NONE',  ( 117.7882081442453170, -6.344957434206665248, -7.627207830600338134 ) ) ;
#14708 = CARTESIAN_POINT ( 'NONE',  ( 120.0005481442453146, -4.153390946401325223, -8.397313243818185668 ) ) ;
#14709 = VERTEX_POINT ( 'NONE', #43469 ) ;
#14710 = EDGE_CURVE ( 'NONE', #36696, #20709, #15922, .T. ) ;
#14711 = CARTESIAN_POINT ( 'NONE',  ( 122.2128881442453263, -7.643976991954077427, -18.09477374809248928 ) ) ;
#14712 = EDGE_CURVE ( 'NONE', #15181, #32644, #43243, .T. ) ;
#14713 = ADVANCED_FACE ( 'NONE', ( #25467 ), #20590, .T. ) ;
#14714 = CARTESIAN_POINT ( 'NONE',  ( 119.9438214775786378, -7.893985811506177619, -18.51759400769804742 ) ) ;
#14715 = DIRECTION ( 'NONE',  ( -0.000000000000000000, -0.9284778069183721172, -0.3713878862591650232 ) ) ;
#14716 = CARTESIAN_POINT ( 'NONE',  ( 110.3436608795247764, -8.938348069036489818, -9.318865927141430916 ) ) ;
#14717 = CARTESIAN_POINT ( 'NONE',  ( 62.93082072131119276, -14.63772337390263978, -9.513022489315044794 ) ) ;
#14718 = CARTESIAN_POINT ( 'NONE',  ( 116.8449686807541781, 0.3528313838059640717, -14.64321520033831447 ) ) ;
#14719 = CARTESIAN_POINT ( 'NONE',  ( 112.9828796295247884, -4.863998795839590272, -8.388885654883775800 ) ) ;
#14720 = CARTESIAN_POINT ( 'NONE',  ( 113.5904348109119866, -7.893985811506177619, -18.51759400769804742 ) ) ;
#14721 = CARTESIAN_POINT ( 'NONE',  ( 75.95778847736514194, -3.256761025687008537, -7.147228641687434880 ) ) ;
#14722 = CARTESIAN_POINT ( 'NONE',  ( 116.9373081442452929, -1.833838273342659253, -17.42832698103878286 ) ) ;
#14723 = DIRECTION ( 'NONE',  ( -0.000000000000000000, -0.9284778069183721172, -0.3713878862591650232 ) ) ;
#14724 = DIRECTION ( 'NONE',  ( 1.000000000000000000, 0.000000000000000000, 0.000000000000000000 ) ) ;
#14725 = CARTESIAN_POINT ( 'NONE',  ( 112.2883483795247770, -8.402594152722688392, -16.93181055722141792 ) ) ;
#14726 = CARTESIAN_POINT ( 'NONE',  ( 113.3635281442453504, -0.1624402480850797581, -16.17319339645315424 ) ) ;
#14727 = CARTESIAN_POINT ( 'NONE',  ( 35.67453213195965134, -67.60842401891365228, -18.19321520033831519 ) ) ;
#14728 = ADVANCED_FACE ( 'NONE', ( #35141 ), #31737, .F. ) ;
#14729 = VECTOR ( 'NONE', #29627, 1000.000000000000000 ) ;
#14730 = LINE ( 'NONE', #7652, #35474 ) ;
#14732 = CARTESIAN_POINT ( 'NONE',  ( 119.8870948109119752, -9.261995988541697145, -16.69588392320189030 ) ) ;
#14731 = CARTESIAN_POINT ( 'NONE',  ( 63.78489101950506068, -13.55204749033676848, -8.443300631150968627 ) ) ;
#14733 = CARTESIAN_POINT ( 'NONE',  ( 119.3198281442452924, -9.859900752359374465, -12.68260735090039404 ) ) ;
#14734 = CARTESIAN_POINT ( 'NONE',  ( 111.2646414775786496, -8.899110576539710493, -16.42337572283490132 ) ) ;
#14735 = VERTEX_POINT ( 'NONE', #28559 ) ;
#14736 = CARTESIAN_POINT ( 'NONE',  ( 136.9012041053403834, -7.147266434572221883, -8.356081441750150773 ) ) ;
#14737 = CARTESIAN_POINT ( 'NONE',  ( 124.1983214775786166, -8.166667518702819706, -8.995218007635861213 ) ) ;
#14738 = CARTESIAN_POINT ( 'NONE',  ( 112.9828796295247884, -4.863998795839590272, -8.388885654883775800 ) ) ;
#14739 = CARTESIAN_POINT ( 'NONE',  ( 120.7379948109119709, 0.4262465694468514643, -12.03445270309931736 ) ) ;
#14740 = ADVANCED_FACE ( 'NONE', ( #7802 ), #18516, .F. ) ;
#14741 = CARTESIAN_POINT ( 'NONE',  ( 117.8449348109119938, -1.833838273342659253, -17.42832698103878286 ) ) ;
#14742 = ADVANCED_FACE ( 'NONE', ( #11229 ), #32407, .F. ) ;
#14743 = CARTESIAN_POINT ( 'NONE',  ( 85.09674465308115998, -29.42238801905354251, -10.32662417038046954 ) ) ;
#14744 = CARTESIAN_POINT ( 'NONE',  ( 113.5385046295247804, -4.863998795839590272, -7.631215200338315796 ) ) ;
#14745 = CARTESIAN_POINT ( 'NONE',  ( 120.1707281442453166, -9.565557343593413364, -10.61323700422348004 ) ) ;
#14746 = CARTESIAN_POINT ( 'NONE',  ( 123.6877814775786533, -6.222761293078241884, -8.102969835052219238 ) ) ;
#14747 = DIRECTION ( 'NONE',  ( 1.000000000000000000, 0.000000000000000000, -0.000000000000000000 ) ) ;
#14748 = CARTESIAN_POINT ( 'NONE',  ( 109.2294401788930998, -1.084644456222203290, -9.551446960330030933 ) ) ;
#14749 = CARTESIAN_POINT ( 'NONE',  ( 123.0772048109119652, -7.554583864224885481, -18.48844787311982785 ) ) ;
#14750 = CARTESIAN_POINT ( 'NONE',  ( 106.8015515045248378, -6.936859964151250502, -18.39754474579286025 ) ) ;
#14751 = DIRECTION ( 'NONE',  ( 0.9659258262890689783, 0.2588190451025180194, 0.000000000000000000 ) ) ;
#14752 = CARTESIAN_POINT ( 'NONE',  ( 117.6747548109119919, -1.834011780172310813, -8.268836392978581529 ) ) ;
#14753 = CARTESIAN_POINT ( 'NONE',  ( 119.3198281442452924, 0.5811942927096110934, -14.16772938898807510 ) ) ;
#14754 = CARTESIAN_POINT ( 'NONE',  ( 110.0658483795247804, -0.7896495226426338832, -9.318865927141430916 ) ) ;
#14755 = CARTESIAN_POINT ( 'NONE',  ( 113.5904348109119866, -7.893985811506177619, -18.51759400769804742 ) ) ;
#14756 = VERTEX_POINT ( 'NONE', #32631 ) ;
#14757 = CARTESIAN_POINT ( 'NONE',  ( 113.2885155643466817, -1.244021962887382315, -16.96476564598603787 ) ) ;
#14758 = CARTESIAN_POINT ( 'NONE',  ( 116.3700414775786527, -5.638512984488999180, -18.83840828888717311 ) ) ;
#14759 = CARTESIAN_POINT ( 'NONE',  ( 120.9649014775786355, -6.222761293078241884, -8.102969835052219238 ) ) ;
#14760 = DIRECTION ( 'NONE',  ( 1.000000000000000000, 0.000000000000000000, 0.000000000000000000 ) ) ;
#14761 = EDGE_CURVE ( 'NONE', #30697, #11967, #29900, .T. ) ;
#14762 = CARTESIAN_POINT ( 'NONE',  ( 125.9001214775786224, -4.089484607189486809, -7.948022111789456723 ) ) ;
#14763 = CARTESIAN_POINT ( 'NONE',  ( 121.5321681442453183, -9.988377603198976828, -10.36322818467138340 ) ) ;
#14764 = EDGE_CURVE ( 'NONE', #27606, #25132, #25599, .T. ) ;
#14765 = EDGE_CURVE ( 'NONE', #27202, #16955, #26316, .T. ) ;
#14766 = MECHANICAL_DESIGN_GEOMETRIC_PRESENTATION_REPRESENTATION (  '', ( #35147 ), #43897 ) ;
#14767 = CARTESIAN_POINT ( 'NONE',  ( 115.2748327545248657, -2.477300249445798297, -19.15521520033831138 ) ) ;
#14768 = CARTESIAN_POINT ( 'NONE',  ( 115.5758681442453053, -7.894159318335828068, -9.358103419637847864 ) ) ;
#14769 = CARTESIAN_POINT ( 'NONE',  ( 121.0630641859119976, -0.8832429491016019485, -18.19431474523657855 ) ) ;
#14770 = EDGE_LOOP ( 'NONE', ( #23221, #31978, #21629, #7018, #29437 ) ) ;
#14771 = CARTESIAN_POINT ( 'NONE',  ( 124.1884548109119777, -7.554583864224885481, -18.48844787311982785 ) ) ;
#14772 = CARTESIAN_POINT ( 'NONE',  ( 120.5678148109119832, -8.166667518702819706, -8.995218007635861213 ) ) ;
#14773 = ORIENTED_EDGE ( 'NONE', *, *, #902, .F. ) ;
#14774 = DIRECTION ( 'NONE',  ( -0.000000000000000000, -0.9284778069183718952, -0.3713878862591649677 ) ) ;
#14775 = CARTESIAN_POINT ( 'NONE',  ( 46.47434218039879283, -17.93412427487546523, -8.593215200338315540 ) ) ;
#14776 = CARTESIAN_POINT ( 'NONE',  ( 121.9484597424434043, -0.9924539043446216624, -17.29976612834909133 ) ) ;
#14777 = CARTESIAN_POINT ( 'NONE',  ( 117.4478481442453131, -9.565557343593413364, -10.61323700422348004 ) ) ;
#14778 = DIRECTION ( 'NONE',  ( 0.1352586133457925055, 0.9908103287288507754, 0.000000000000000000 ) ) ;
#14779 = CARTESIAN_POINT ( 'NONE',  ( 124.1049594150595823, -2.423081321603731908, -17.89265170041263175 ) ) ;
#14780 = CARTESIAN_POINT ( 'NONE',  ( 119.9438214775786378, -2.084020599724406786, -8.691656652584148546 ) ) ;
#14781 = DIRECTION ( 'NONE',  ( -0.9609149988134837450, 0.1028163501681645109, -0.2570431154366520921 ) ) ;
#14782 = AXIS2_PLACEMENT_3D ( 'NONE', #2288, #16442, #44266 ) ;
#14783 = CARTESIAN_POINT ( 'NONE',  ( 123.1205148109119563, -7.643976991954077427, -18.09477374809248928 ) ) ;
#14784 = AXIS2_PLACEMENT_3D ( 'NONE', #27817, #20754, #17335 ) ;
#14785 = CARTESIAN_POINT ( 'NONE',  ( 123.9584548109119737, -11.17722486020181627, -8.479644537342501565 ) ) ;
#14786 = CARTESIAN_POINT ( 'NONE',  ( 119.8303681442453126, 0.4262465694468514643, -12.03445270309931736 ) ) ;
#14787 = CARTESIAN_POINT ( 'NONE',  ( 114.8951481442453115, -0.4660016031367893996, -10.09054647747474043 ) ) ;
#14788 = CARTESIAN_POINT ( 'NONE',  ( 119.8870948109119752, -9.261995988541697145, -16.69588392320189030 ) ) ;
#14789 = CARTESIAN_POINT ( 'NONE',  ( 126.6942948109119840, -8.899110576539710493, -16.42337572283490132 ) ) ;
#14790 = DIRECTION ( 'NONE',  ( 1.000000000000000000, 0.000000000000000000, 0.000000000000000000 ) ) ;
#14791 = CARTESIAN_POINT ( 'NONE',  ( 122.0427081442452817, -9.859900752359378018, -12.68260735090039759 ) ) ;
#14792 = ORIENTED_EDGE ( 'NONE', *, *, #8059, .T. ) ;
#14793 = CARTESIAN_POINT ( 'NONE',  ( 119.2631014775786298, 0.2603800115204892296, -16.42320221600525088 ) ) ;
#14794 = CARTESIAN_POINT ( 'NONE',  ( 113.9552233795247815, -1.325403438956436419, -9.854619843455211026 ) ) ;
#14795 = CARTESIAN_POINT ( 'NONE',  ( 69.36136150295220659, -101.1685209014307674, -50.56525720990386219 ) ) ;
#14796 = AXIS2_PLACEMENT_3D ( 'NONE', #13824, #30930, #13606 ) ;
#14797 = DIRECTION ( 'NONE',  ( -0.000000000000000000, -0.9284778069183721172, -0.3713878862591650232 ) ) ;
#14798 = DIRECTION ( 'NONE',  ( 0.000000000000000000, -0.3818493186865927203, 0.9242245927363029745 ) ) ;
#14799 = CARTESIAN_POINT ( 'NONE',  ( 125.9568481442452850, -6.344957434206665248, -7.627207830600338134 ) ) ;
#14800 = ORIENTED_EDGE ( 'NONE', *, *, #22250, .T. ) ;
#14801 = CARTESIAN_POINT ( 'NONE',  ( 82.31000308962319423, -13.76004065658516673, -18.64321520033831803 ) ) ;
#14802 = CARTESIAN_POINT ( 'NONE',  ( 123.3474214775786209, -0.1624402480850797581, -16.17319339645315424 ) ) ;
#14803 = CARTESIAN_POINT ( 'NONE',  ( 120.9936110609119737, -3.163656168406935087, -18.89861972220014508 ) ) ;
#14804 = CARTESIAN_POINT ( 'NONE',  ( 65.55333354794366585, -16.16208837894097883, -16.95583544328367154 ) ) ;
#14805 = EDGE_CURVE ( 'NONE', #14242, #35800, #13239, .T. ) ;
#14806 = CARTESIAN_POINT ( 'NONE',  ( 70.19189222814998175, -49.76310523276723785, -36.33917278160906505 ) ) ;
#14807 = CARTESIAN_POINT ( 'NONE',  ( 114.3024890045248156, -9.868328341294098749, -11.32035403202665869 ) ) ;
#14808 = EDGE_LOOP ( 'NONE', ( #33730, #23733, #6585, #293 ) ) ;
#14809 = CARTESIAN_POINT ( 'NONE',  ( 114.5547881442453217, -5.638512984488999180, -18.83840828888717311 ) ) ;
#14810 = CARTESIAN_POINT ( 'NONE',  ( 113.1933481442453058, -4.089484607189486809, -7.948022111789456723 ) ) ;
#14811 = CARTESIAN_POINT ( 'NONE',  ( 125.6732148109119862, 0.5811942927096110934, -14.16772938898807510 ) ) ;
#14812 = CARTESIAN_POINT ( 'NONE',  ( 119.3198281442452924, -9.859900752359374465, -12.68260735090039404 ) ) ;
#14813 = CARTESIAN_POINT ( 'NONE',  ( 126.2597653975865200, -3.915316323808516685, -8.462872152827413785 ) ) ;
#14814 = PRESENTATION_STYLE_ASSIGNMENT (( #39433 ) ) ;
#14815 = CARTESIAN_POINT ( 'NONE',  ( 124.1415948109119540, -6.344957434206665248, -7.627207830600338134 ) ) ;
#14816 = CARTESIAN_POINT ( 'NONE',  ( 123.5743281442453139, -2.084020599724360601, -8.691656652584175191 ) ) ;
#14817 = DIRECTION ( 'NONE',  ( 0.9908103287288505534, -0.1352586133457945317, 0.000000000000000000 ) ) ;
#14818 = CARTESIAN_POINT ( 'NONE',  ( 63.38258667102197563, -64.24438017783141674, -46.60357888607674681 ) ) ;
#14819 = CARTESIAN_POINT ( 'NONE',  ( 112.5693548109119888, -10.63000616557722466, -14.87417383870573495 ) ) ;
#14820 = ORIENTED_EDGE ( 'NONE', *, *, #26999, .F. ) ;
#14821 = CARTESIAN_POINT ( 'NONE',  ( 80.91184012100937650, -3.933054092416038650, -15.89321520033831447 ) ) ;
#14822 = CIRCLE ( 'NONE', #3871, 2.000000000000000444 ) ;
#14823 = ADVANCED_FACE ( 'NONE', ( #43130 ), #12725, .T. ) ;
#14824 = CARTESIAN_POINT ( 'NONE',  ( 121.1350814775786233, 0.5811942927096110934, -14.16772938898807510 ) ) ;
#14825 = CARTESIAN_POINT ( 'NONE',  ( 62.38855081628511101, -1.739798814707631980, -17.65581714534172519 ) ) ;
#14826 = ORIENTED_EDGE ( 'NONE', *, *, #3062, .F. ) ;
#14827 = EDGE_CURVE ( 'NONE', #30504, #11410, #3046, .T. ) ;
#14828 = DIRECTION ( 'NONE',  ( -0.000000000000000000, -0.9284778069183721172, -0.3713878862591650232 ) ) ;
#14829 = CARTESIAN_POINT ( 'NONE',  ( 124.5386814775786206, -5.638512984488999180, -18.83840828888717311 ) ) ;
#14830 = CARTESIAN_POINT ( 'NONE',  ( 127.7617783745703974, -4.238963850480659268, -19.13134216130518794 ) ) ;
#14831 = CARTESIAN_POINT ( 'NONE',  ( 122.7234281442452755, -4.153390946401325223, -8.397313243818185668 ) ) ;
#14832 = CONICAL_SURFACE ( 'NONE', #22089, 2.000000000000000444, 0.9599310885968830309 ) ;
#14833 = ORIENTED_EDGE ( 'NONE', *, *, #31713, .F. ) ;
#14834 = CARTESIAN_POINT ( 'NONE',  ( 116.9373081442452929, -8.166667518702817929, -8.995218007635861213 ) ) ;
#14835 = CARTESIAN_POINT ( 'NONE',  ( 69.69189222814998175, -41.76310523276723785, -24.89321520033831447 ) ) ;
#14836 = CARTESIAN_POINT ( 'NONE',  ( 120.5110881442453064, -6.344957434206645708, -7.627207830600334582 ) ) ;
#14837 = CARTESIAN_POINT ( 'NONE',  ( 136.7741008876058402, -5.359462442573635244, -7.806884787152266192 ) ) ;
#14838 = CARTESIAN_POINT ( 'NONE',  ( 111.9453614775786434, -7.894159318335828068, -9.358103419637847864 ) ) ;
#14839 = FACE_OUTER_BOUND ( 'NONE', #7353, .T. ) ;
#14840 = CARTESIAN_POINT ( 'NONE',  ( 70.19189222814998175, -49.76310523276723785, -29.87698278062876511 ) ) ;
#14841 = CARTESIAN_POINT ( 'NONE',  ( 122.0427081442452817, 0.5811942927096110934, -14.16772938898807510 ) ) ;
#14843 = CARTESIAN_POINT ( 'NONE',  ( 122.7234281442452755, -4.153390946401325223, -8.397313243818185668 ) ) ;
#14842 = CARTESIAN_POINT ( 'NONE',  ( 124.1415948109119540, -6.344957434206665248, -7.627207830600338134 ) ) ;
#14844 = CARTESIAN_POINT ( 'NONE',  ( 116.6769462226555163, -8.438241265790122014, -17.00663296034464267 ) ) ;
#14845 = CARTESIAN_POINT ( 'NONE',  ( 124.6521348109119884, -7.894159318335828068, -9.358103419637847864 ) ) ;
#14846 = CARTESIAN_POINT ( 'NONE',  ( 90.99708770779186295, -25.99489077589524300, -13.39321520033831447 ) ) ;
#14847 = CARTESIAN_POINT ( 'NONE',  ( 121.3619881442452879, -4.089484607189486809, -7.948022111789456723 ) ) ;
#14848 = ORIENTED_EDGE ( 'NONE', *, *, #11927, .T. ) ;
#14849 = AXIS2_PLACEMENT_3D ( 'NONE', #33773, #16470, #41983 ) ;
#14850 = ORIENTED_EDGE ( 'NONE', *, *, #2037, .F. ) ;
#14851 = DIRECTION ( 'NONE',  ( 0.000000000000000000, 0.000000000000000000, -1.000000000000000000 ) ) ;
#14852 = DIRECTION ( 'NONE',  ( 0.5040994586965589219, 0.8636456077245088236, 0.000000000000000000 ) ) ;
#14853 = CARTESIAN_POINT ( 'NONE',  ( 105.5513952545248060, 0.8980012041604421569, -11.00651665394454071 ) ) ;
#14854 = CARTESIAN_POINT ( 'NONE',  ( 111.5243640045248412, 0.1403307496149616695, -15.46607636864997204 ) ) ;
#14855 = DIRECTION ( 'NONE',  ( -0.000000000000000000, -0.9284778069183720062, -0.3713878862591650232 ) ) ;
#14856 = CARTESIAN_POINT ( 'NONE',  ( 116.8805814775786445, -6.344957434206662583, -7.627207830600332805 ) ) ;
#14857 = EDGE_LOOP ( 'NONE', ( #26723, #38142 ) ) ;
#14858 = CARTESIAN_POINT ( 'NONE',  ( 111.9453614775786434, -7.894159318335828068, -9.358103419637847864 ) ) ;
#14859 = CARTESIAN_POINT ( 'NONE',  ( 105.6208483795248299, -0.7896495226426338832, -9.318865927141430916 ) ) ;
#14860 = DIRECTION ( 'NONE',  ( 0.8636456077245088236, -0.5040994586965589219, 0.000000000000000000 ) ) ;
#14861 = DIRECTION ( 'NONE',  ( 0.000000000000000000, 0.000000000000000000, -1.000000000000000000 ) ) ;
#14862 = CARTESIAN_POINT ( 'NONE',  ( 122.5532481442453019, 0.4262465694468476896, -12.03445270309931381 ) ) ;
#14863 = CARTESIAN_POINT ( 'NONE',  ( 62.23965954364709319, -13.31694178448660004, -18.96568801859871911 ) ) ;
#14864 = CARTESIAN_POINT ( 'NONE',  ( 116.0296814775786345, -8.166667518702817929, -8.995218007635861213 ) ) ;
#14865 = CARTESIAN_POINT ( 'NONE',  ( 113.8857702545248003, -10.62599879583958717, -15.77991374673208469 ) ) ;
#14866 = CARTESIAN_POINT ( 'NONE',  ( 111.1770983795247787, -8.402594152722688392, -16.93181055722141792 ) ) ;
#14867 = ORIENTED_EDGE ( 'NONE', *, *, #8324, .F. ) ;
#14868 = CARTESIAN_POINT ( 'NONE',  ( 126.2471382750679822, -7.710119271726137313, -9.264776471331988006 ) ) ;
#14869 = CARTESIAN_POINT ( 'NONE',  ( 119.4332814775786318, -8.899110576539710493, -16.42337572283490132 ) ) ;
#14870 = CARTESIAN_POINT ( 'NONE',  ( 117.1074881442453233, -10.63000616557722466, -14.87417383870573495 ) ) ;
#14871 = CARTESIAN_POINT ( 'NONE',  ( 70.19189222814998175, -54.47411573338475677, -34.99246555962335492 ) ) ;
#14872 = CARTESIAN_POINT ( 'NONE',  ( 125.3895814775786448, -2.084020599724406786, -8.691656652584148546 ) ) ;
#14873 = CARTESIAN_POINT ( 'NONE',  ( 118.9794681442453026, -0.8288870151387760510, -10.36305467784173118 ) ) ;
#14874 = CARTESIAN_POINT ( 'NONE',  ( 115.2355081442453155, 0.1319031606808879209, -14.10382304977623669 ) ) ;
#14875 = ORIENTED_EDGE ( 'NONE', *, *, #29390, .T. ) ;
#14876 = CARTESIAN_POINT ( 'NONE',  ( 122.5910329359119970, -5.367793381288652910, -18.78638297431638904 ) ) ;
#14877 = EDGE_CURVE ( 'NONE', #19823, #44794, #28333, .T. ) ;
#14878 = CARTESIAN_POINT ( 'NONE',  ( 121.9470836909669913, -24.14644159042263993, -12.62951656296512937 ) ) ;
#14879 = CARTESIAN_POINT ( 'NONE',  ( 116.5969481442453031, -9.859900752359374465, -12.68260735090039404 ) ) ;
#14880 = ORIENTED_EDGE ( 'NONE', *, *, #7203, .F. ) ;
#14881 = CARTESIAN_POINT ( 'NONE',  ( 65.04066262153794753, -15.49774765191802750, -10.45160382476714922 ) ) ;
#14882 = CARTESIAN_POINT ( 'NONE',  ( 114.4980614775786592, -7.893985811506177619, -18.51759400769804742 ) ) ;
#14883 = CONICAL_SURFACE ( 'NONE', #19994, 2.445500000000004448, 0.9599310885968757034 ) ;
#14884 = CARTESIAN_POINT ( 'NONE',  ( 116.3860827545247787, -2.477300249445798297, -19.15521520033831138 ) ) ;
#14885 = CARTESIAN_POINT ( 'NONE',  ( 114.2711548109119803, -0.1624402480850797581, -16.17319339645315424 ) ) ;
#14886 = ORIENTED_EDGE ( 'NONE', *, *, #27820, .F. ) ;
#14887 = EDGE_LOOP ( 'NONE', ( #20491, #23827, #27687, #34249 ) ) ;
#14888 = CARTESIAN_POINT ( 'NONE',  ( 123.0070614775786169, -10.15424416112533912, -14.75197769757731336 ) ) ;
#14889 = CARTESIAN_POINT ( 'NONE',  ( 116.3133148109120043, -2.084020599724406786, -8.691656652584148546 ) ) ;
#14890 = CARTESIAN_POINT ( 'NONE',  ( 86.48169505875749508, -26.75858941326842810, -11.54476601486570964 ) ) ;
#14891 = CARTESIAN_POINT ( 'NONE',  ( 123.2161110609119561, -3.163656168406935087, -18.89861972220014508 ) ) ;
#14892 = ORIENTED_EDGE ( 'NONE', *, *, #31399, .F. ) ;
#14893 = DIRECTION ( 'NONE',  ( 0.1352586133457954198, 0.9908103287288503314, 0.000000000000000000 ) ) ;
#14894 = CARTESIAN_POINT ( 'NONE',  ( 124.4646854081442626, -2.418452363927385385, -5.864561580288276232 ) ) ;
#14895 = CARTESIAN_POINT ( 'NONE',  ( 110.8298327545248299, -2.477300249445798297, -19.15521520033831138 ) ) ;
#14896 = ADVANCED_FACE ( 'NONE', ( #45005 ), #30827, .F. ) ;
#14897 = DIRECTION ( 'NONE',  ( 0.000000000000000000, 0.000000000000000000, -1.000000000000000000 ) ) ;
#14898 = CARTESIAN_POINT ( 'NONE',  ( 112.9097148109120070, 0.2603800115204892296, -16.42320221600525088 ) ) ;
#14899 = CARTESIAN_POINT ( 'NONE',  ( 122.7234281442452755, -4.153390946401325223, -8.397313243818185668 ) ) ;
#14900 = CARTESIAN_POINT ( 'NONE',  ( 143.3676850761856940, -55.76310523276723785, -40.89321520033831092 ) ) ;
#14901 = EDGE_LOOP ( 'NONE', ( #19416, #663, #20033, #1853, #37146, #993 ) ) ;
#14902 = CARTESIAN_POINT ( 'NONE',  ( 121.0783548109119749, -9.565557343593413364, -10.61323700422348004 ) ) ;
#14903 = CIRCLE ( 'NONE', #4710, 2.000000000000000444 ) ;
#14904 = DIRECTION ( 'NONE',  ( -0.000000000000000000, -0.9284778069183718952, -0.3713878862591649677 ) ) ;
#14905 = DIRECTION ( 'NONE',  ( 0.5040994586965589219, 0.8636456077245088236, 0.000000000000000000 ) ) ;
#14906 = CARTESIAN_POINT ( 'NONE',  ( 115.6220983795247861, -0.7896495226426338832, -9.318865927141430916 ) ) ;
#14907 = CARTESIAN_POINT ( 'NONE',  ( 114.5547881442453217, -5.638512984488999180, -18.83840828888717311 ) ) ;
#14908 = ORIENTED_EDGE ( 'NONE', *, *, #40368, .T. ) ;
#14909 = CARTESIAN_POINT ( 'NONE',  ( 119.0361948109119652, -7.893985811506177619, -18.51759400769804742 ) ) ;
#14910 = DIRECTION ( 'NONE',  ( 1.000000000000000000, 0.000000000000000000, -0.000000000000000000 ) ) ;
#14911 = CARTESIAN_POINT ( 'NONE',  ( 112.5661608795247872, -8.938348069036489818, -9.318865927141430916 ) ) ;
#14912 = CARTESIAN_POINT ( 'NONE',  ( 116.8805814775786445, -6.344957434206662583, -7.627207830600332805 ) ) ;
#14913 = CARTESIAN_POINT ( 'NONE',  ( 117.9583881442453048, -10.30919188438810075, -12.61870101168855918 ) ) ;
#14915 = AXIS2_PLACEMENT_3D ( 'NONE', #38431, #13169, #16590 ) ;
#14914 = CARTESIAN_POINT ( 'NONE',  ( 62.09114116458580668, -3.664294667776160974, -19.28739984847905831 ) ) ;
#14916 = DIRECTION ( 'NONE',  ( 1.000000000000000000, 0.000000000000000000, -0.000000000000000000 ) ) ;
#14917 = DIRECTION ( 'NONE',  ( 0.000000000000000000, 0.000000000000000000, -1.000000000000000000 ) ) ;
#14918 = VERTEX_POINT ( 'NONE', #15998 ) ;
#14919 = CARTESIAN_POINT ( 'NONE',  ( 116.3166296295247832, -4.863998795839590272, -19.15521520033831493 ) ) ;
#14920 = CARTESIAN_POINT ( 'NONE',  ( 109.2295328744424125, -6.711379979716183719, -18.33685733204155355 ) ) ;
#14921 = CARTESIAN_POINT ( 'NONE',  ( 120.3409081442453044, -8.899110576539710493, -16.42337572283490132 ) ) ;
#14922 = DIRECTION ( 'NONE',  ( -0.7071067811865480168, 0.5654279342907823080, 0.4246071727180995570 ) ) ;
#14923 = CARTESIAN_POINT ( 'NONE',  ( 114.9275671295247889, 0.1403307496149613920, -13.39321520033831447 ) ) ;
#14924 = CARTESIAN_POINT ( 'NONE',  ( 106.6626452545248611, 0.8980012041604421569, -11.00651665394454071 ) ) ;
#14925 = CARTESIAN_POINT ( 'NONE',  ( 126.6211808763662248, -4.885409866343571217, -8.191703873976955208 ) ) ;
#14926 = CARTESIAN_POINT ( 'NONE',  ( 113.7038881442453402, -6.222761293078241884, -8.102969835052219238 ) ) ;
#14927 = DIRECTION ( 'NONE',  ( -0.9908103287288502203, 0.1352586133457974182, 0.000000000000000000 ) ) ;
#14928 = CARTESIAN_POINT ( 'NONE',  ( 124.0848681442452772, -4.089484607189486809, -7.948022111789456723 ) ) ;
#14929 = CARTESIAN_POINT ( 'NONE',  ( 120.3976348109119812, -1.834011780172310813, -8.268836392978581529 ) ) ;
#14930 = EDGE_LOOP ( 'NONE', ( #27169, #23457, #44051, #39026, #40927 ) ) ;
#14931 = CARTESIAN_POINT ( 'NONE',  ( 118.4122014775786340, -9.859900752359374465, -12.68260735090039404 ) ) ;
#14932 = CARTESIAN_POINT ( 'NONE',  ( 126.1837548109119211, -10.63000616557722466, -14.87417383870573495 ) ) ;
#14933 = CARTESIAN_POINT ( 'NONE',  ( 116.5402214775786405, 0.2603800115204892296, -16.42320221600525088 ) ) ;
#14934 = CARTESIAN_POINT ( 'NONE',  ( 120.2841814775786276, -10.15424416112533912, -14.75197769757731336 ) ) ;
#14935 = ORIENTED_EDGE ( 'NONE', *, *, #4943, .T. ) ;
#14936 = CARTESIAN_POINT ( 'NONE',  ( 116.5026997424434114, -0.9924539043446216624, -17.29976612834909133 ) ) ;
#14937 = VECTOR ( 'NONE', #15502, 1000.000000000000000 ) ;
#14938 = CARTESIAN_POINT ( 'NONE',  ( 118.7525614775786380, -8.166667518702819706, -8.995218007635861213 ) ) ;
#14939 = CARTESIAN_POINT ( 'NONE',  ( 135.3184548109119874, -4.863998795839242995, -13.39321520033831447 ) ) ;
#14940 = CARTESIAN_POINT ( 'NONE',  ( 108.0517077545248696, -7.250697342233347165, -7.631215200338321125 ) ) ;
#14941 = AXIS2_PLACEMENT_3D ( 'NONE', #27586, #42159, #10920 ) ;
#14942 = CARTESIAN_POINT ( 'NONE',  ( 63.92618626572875229, -15.01321783771896534, -10.28494218876606858 ) ) ;
#14943 = CARTESIAN_POINT ( 'NONE',  ( 116.5564130180080866, 0.7607806665037644134, -14.64321520033833401 ) ) ;
#14944 = CARTESIAN_POINT ( 'NONE',  ( 114.4413952545248350, -9.868328341294098749, -15.46607636864997204 ) ) ;
#14945 = CARTESIAN_POINT ( 'NONE',  ( 117.3911214775786505, -1.561330072975668504, -17.79121239304076951 ) ) ;
#14946 = DIRECTION ( 'NONE',  ( 1.000000000000000000, 0.000000000000000000, 0.000000000000000000 ) ) ;
#14947 = CARTESIAN_POINT ( 'NONE',  ( 117.3911214775786505, -7.894159318335828068, -9.358103419637847864 ) ) ;
#14948 = CARTESIAN_POINT ( 'NONE',  ( 112.1234697116520920, -8.918491192341182483, -16.31914947962552631 ) ) ;
#14949 = CARTESIAN_POINT ( 'NONE',  ( 112.1874712410415924, 0.7607806665037644134, -12.14321520033829493 ) ) ;
#14950 = CARTESIAN_POINT ( 'NONE',  ( 108.7462390045248242, -9.868328341294098749, -11.32035403202665869 ) ) ;
#14951 = CARTESIAN_POINT ( 'NONE',  ( 113.3068014775786594, -1.833838273342658809, -17.42832698103878286 ) ) ;
#14952 = DIRECTION ( 'NONE',  ( 1.000000000000000000, 0.000000000000000000, 0.000000000000000000 ) ) ;
#14953 = CARTESIAN_POINT ( 'NONE',  ( 71.57611010347959279, -68.55582966742440476, -45.79978146116413029 ) ) ;
#14955 = CARTESIAN_POINT ( 'NONE',  ( 117.5045748109119756, 0.5811942927096110934, -14.16772938898807510 ) ) ;
#14954 = CARTESIAN_POINT ( 'NONE',  ( 60.99435512697144190, -13.32931833351154793, -7.514629966800860927 ) ) ;
#14956 = CARTESIAN_POINT ( 'NONE',  ( 117.3911214775786505, -7.894159318335828068, -9.358103419637847864 ) ) ;
#14957 = CARTESIAN_POINT ( 'NONE',  ( 111.9453614775786434, -7.894159318335828068, -9.358103419637847864 ) ) ;
#14958 = VERTEX_POINT ( 'NONE', #36726 ) ;
#14959 = CARTESIAN_POINT ( 'NONE',  ( 78.69189222814998175, -69.76310523276724496, -32.79321520033831661 ) ) ;
#14960 = CARTESIAN_POINT ( 'NONE',  ( 121.9292548109119849, -1.561330072975668948, -17.79121239304076951 ) ) ;
#14961 = CARTESIAN_POINT ( 'NONE',  ( 113.9552233795247815, -1.325403438956436419, -9.854619843455211026 ) ) ;
#14962 = CARTESIAN_POINT ( 'NONE',  ( 119.5467348109119712, -5.574606645277164318, -18.38911715685844683 ) ) ;
#14963 = CARTESIAN_POINT ( 'NONE',  ( 115.6893214775786447, -9.859900752359374465, -12.68260735090039404 ) ) ;
#14964 = CARTESIAN_POINT ( 'NONE',  ( 85.35964865273379587, -28.78522156022691547, -9.527126118789240650 ) ) ;
#14965 = CARTESIAN_POINT ( 'NONE',  ( 109.3713171295247832, -10.62599879583958540, -13.39321520033831447 ) ) ;
#14966 = AXIS2_PLACEMENT_3D ( 'NONE', #34556, #21107, #45069 ) ;
#14967 = CARTESIAN_POINT ( 'NONE',  ( 123.3474214775786209, -0.1624402480850797581, -16.17319339645315424 ) ) ;
#14968 = CARTESIAN_POINT ( 'NONE',  ( 122.5532481442453019, 0.4262465694468514643, -12.03445270309931736 ) ) ;
#14969 = CARTESIAN_POINT ( 'NONE',  ( 114.9518748109119883, -7.643976991954099631, -18.09477374809247152 ) ) ;
#14970 = CARTESIAN_POINT ( 'NONE',  ( 109.2294452810045300, -4.985890647812309062, -7.812765507842175161 ) ) ;
#14971 = CARTESIAN_POINT ( 'NONE',  ( 123.7717360609119623, -6.564341423271550902, -7.887810678476487425 ) ) ;
#14972 = CARTESIAN_POINT ( 'NONE',  ( 106.3848327545248651, -6.936859964151250502, -8.388885654883777576 ) ) ;
#14973 = CARTESIAN_POINT ( 'NONE',  ( 117.0710753504221060, 1.661863614013754153, -21.31253633978158035 ) ) ;
#14974 = CARTESIAN_POINT ( 'NONE',  ( 82.66491059565053945, -31.44298744622023989, -22.15403020929251454 ) ) ;
#14975 = CARTESIAN_POINT ( 'NONE',  ( 116.3700414775786527, -5.638512984488999180, -18.83840828888717311 ) ) ;
#14976 = CARTESIAN_POINT ( 'NONE',  ( 118.9794681442453026, -9.261995988541697145, -16.69588392320189030 ) ) ;
#14977 = CARTESIAN_POINT ( 'NONE',  ( 110.3436608795247764, -8.938348069036489818, -9.318865927141430916 ) ) ;
#14978 = CARTESIAN_POINT ( 'NONE',  ( 112.1155414775786454, 0.9020085738987339008, -11.91225656197089222 ) ) ;
#14979 = VERTEX_POINT ( 'NONE', #22831 ) ;
#14980 = CARTESIAN_POINT ( 'NONE',  ( 117.1754969549021723, -1.135392229370316031, -17.10942237759952533 ) ) ;
#14981 = CONICAL_SURFACE ( 'NONE', #20102, 2.445500000000004448, 0.9599310885968757034 ) ;
#14982 = CARTESIAN_POINT ( 'NONE',  ( 116.9373081442452929, -8.166667518702817929, -8.995218007635861213 ) ) ;
#14983 = CARTESIAN_POINT ( 'NONE',  ( 122.4965214775786251, 0.1319031606808879209, -14.10382304977623669 ) ) ;
#14984 = CARTESIAN_POINT ( 'NONE',  ( 124.2550481442452792, -9.988377603198980381, -10.36322818467138518 ) ) ;
#14985 = CARTESIAN_POINT ( 'NONE',  ( 121.3052614775786111, -1.834011780172310813, -8.268836392978581529 ) ) ;
#14986 = EDGE_CURVE ( 'NONE', #24500, #408, #23062, .T. ) ;
#14987 = CARTESIAN_POINT ( 'NONE',  ( 112.7050671295247923, -10.62599879583958540, -13.39321520033831447 ) ) ;
#14988 = CARTESIAN_POINT ( 'NONE',  ( 117.9583881442453048, 0.1319031606808879209, -14.10382304977623669 ) ) ;
#14989 = CARTESIAN_POINT ( 'NONE',  ( 121.2019704359119743, 1.345710702986147034, -13.97328579221134426 ) ) ;
#14990 = CARTESIAN_POINT ( 'NONE',  ( 83.84865386347668448, -25.99489077589588604, -11.39321520033831447 ) ) ;
#14991 = ORIENTED_EDGE ( 'NONE', *, *, #30873, .T. ) ;
#14992 = EDGE_CURVE ( 'NONE', #40981, #29459, #15112, .T. ) ;
#14993 = CARTESIAN_POINT ( 'NONE',  ( 119.2572829359120021, -5.367793381288652910, -18.78638297431638904 ) ) ;
#14994 = EDGE_CURVE ( 'NONE', #16741, #36562, #37257, .T. ) ;
#14995 = CARTESIAN_POINT ( 'NONE',  ( 120.4543614775786295, -4.089484607189486809, -7.948022111789456723 ) ) ;
#14996 = EDGE_LOOP ( 'NONE', ( #888, #3637, #10956, #43405 ) ) ;
#14997 = DIRECTION ( 'NONE',  ( -0.2768435750659243300, -0.3568721902840689131, 0.8921882507333129819 ) ) ;
#14998 = CARTESIAN_POINT ( 'NONE',  ( 63.54424027483572246, -3.108909839411367226, -7.798187301296191976 ) ) ;
#14999 = CARTESIAN_POINT ( 'NONE',  ( 70.19189222814998175, -58.18802696105826300, -36.47801710466001879 ) ) ;
#15000 = CARTESIAN_POINT ( 'NONE',  ( 115.8027748109119841, -8.899110576539710493, -16.42337572283490132 ) ) ;
#15001 = CARTESIAN_POINT ( 'NONE',  ( 66.59991520736690518, -0.05656289534533872482, -16.39321520033831092 ) ) ;
#15002 = CARTESIAN_POINT ( 'NONE',  ( 64.09723185476896390, -35.12832872366021775, -5.893215200338315363 ) ) ;
#15003 = CARTESIAN_POINT ( 'NONE',  ( 123.4608748109119745, 0.4262465694468514643, -12.03445270309931736 ) ) ;
#15004 = CARTESIAN_POINT ( 'NONE',  ( 121.7023481442452777, -9.261995988541729119, -16.69588392320184767 ) ) ;
#15005 = AXIS2_PLACEMENT_3D ( 'NONE', #33945, #5294, #29690 ) ;
#15006 = EDGE_CURVE ( 'NONE', #31353, #39217, #14145, .T. ) ;
#15007 = CARTESIAN_POINT ( 'NONE',  ( 121.8725281442453223, -6.222761293078241884, -8.102969835052219238 ) ) ;
#15008 = CARTESIAN_POINT ( 'NONE',  ( 124.8633137343444446, -12.15116448942433713, -10.91275482746690706 ) ) ;
#15009 = CARTESIAN_POINT ( 'NONE',  ( 124.2550481442452792, -0.1624402480850797581, -16.17319339645315424 ) ) ;
#15010 = EDGE_CURVE ( 'NONE', #38595, #10687, #5237, .T. ) ;
#15011 = CARTESIAN_POINT ( 'NONE',  ( 112.7395348109119766, -5.638512984488999180, -18.83840828888717311 ) ) ;
#15012 = CARTESIAN_POINT ( 'NONE',  ( 117.8449348109119938, -8.166667518702817929, -8.995218007635861213 ) ) ;
#15013 = CARTESIAN_POINT ( 'NONE',  ( 126.0703014775786102, -0.1624402480850797581, -16.17319339645315424 ) ) ;
#15014 = LINE ( 'NONE', #35283, #8907 ) ;
#15015 = EDGE_CURVE ( 'NONE', #28999, #8854, #42391, .T. ) ;
#15016 = ADVANCED_FACE ( 'NONE', ( #16911 ), #31686, .T. ) ;
#15017 = CARTESIAN_POINT ( 'NONE',  ( 119.6034614775786196, -3.505236298600246325, -18.68346056562440793 ) ) ;
#15018 = ORIENTED_EDGE ( 'NONE', *, *, #1715, .F. ) ;
#15019 = CARTESIAN_POINT ( 'NONE',  ( 118.8660148109119774, -10.30919188438810075, -12.61870101168855918 ) ) ;
#15020 = CARTESIAN_POINT ( 'NONE',  ( 115.1359265045248605, -2.791137627527939813, -8.388885654883777576 ) ) ;
#15021 = DIRECTION ( 'NONE',  ( 0.000000000000000000, -0.3818493186865927203, 0.9242245927363029745 ) ) ;
#15022 = LINE ( 'NONE', #38953, #15179 ) ;
#15023 = CARTESIAN_POINT ( 'NONE',  ( 120.3685329359119862, -4.283928203966213211, -7.183505701512924446 ) ) ;
#15024 = AXIS2_PLACEMENT_3D ( 'NONE', #27214, #41132, #24454 ) ;
#15025 = CARTESIAN_POINT ( 'NONE',  ( 117.0111608795247946, -1.325403438956436419, -16.93181055722141792 ) ) ;
#15026 = ORIENTED_EDGE ( 'NONE', *, *, #7534, .F. ) ;
#15027 = CARTESIAN_POINT ( 'NONE',  ( 121.7023481442452919, -0.8288870151387760510, -10.36305467784173118 ) ) ;
#15028 = LINE ( 'NONE', #4531, #25004 ) ;
#15029 = CARTESIAN_POINT ( 'NONE',  ( 62.28500519901574251, -13.31919971779094070, -18.95210956505300715 ) ) ;
#15030 = CARTESIAN_POINT ( 'NONE',  ( 125.5030348109119558, -3.383040157471821630, -19.15922257007629170 ) ) ;
#15031 = CARTESIAN_POINT ( 'NONE',  ( 106.5237390045248418, -9.868328341294098749, -11.32035403202665869 ) ) ;
#15032 = AXIS2_PLACEMENT_3D ( 'NONE', #27304, #23202, #3123 ) ;
#15033 = VERTEX_POINT ( 'NONE', #27617 ) ;
#15034 = CARTESIAN_POINT ( 'NONE',  ( 115.2355081442453155, -10.30919188438810075, -12.61870101168855918 ) ) ;
#15035 = CARTESIAN_POINT ( 'NONE',  ( 88.85502916797432249, -10.96495313371121050, -14.14321520033831625 ) ) ;
#15036 = CARTESIAN_POINT ( 'NONE',  ( 120.1140014775786398, -7.894159318335828068, -9.358103419637847864 ) ) ;
#15037 = CARTESIAN_POINT ( 'NONE',  ( 112.5693548109119888, 0.4262465694468514643, -12.03445270309931736 ) ) ;
#15038 = SURFACE_SIDE_STYLE ('',( #32354 ) ) ;
#15039 = DIRECTION ( 'NONE',  ( -1.000000000000000000, 0.000000000000000000, -0.000000000000000000 ) ) ;
#15040 = LINE ( 'NONE', #28950, #23780 ) ;
#15041 = CARTESIAN_POINT ( 'NONE',  ( 65.10287265247758626, -0.4742552606671335269, -10.39321520033831625 ) ) ;
#15042 = FILL_AREA_STYLE ('',( #4317 ) ) ;
#15043 = EDGE_LOOP ( 'NONE', ( #3717, #42836, #40307, #33289, #6255, #20225, #16914, #16002, #7150, #24443, #32494, #36937, #6024, #13541, #37183, #28177, #32770, #40042, #7834, #33763, #3150, #3152 ) ) ;
#15044 = AXIS2_PLACEMENT_3D ( 'NONE', #35543, #4315, #898 ) ;
#15045 = CARTESIAN_POINT ( 'NONE',  ( 121.9470836909669913, -27.84333996136784961, -14.15691383771150136 ) ) ;
#15046 = CARTESIAN_POINT ( 'NONE',  ( 121.3052614775786111, -1.834011780172310813, -8.268836392978581529 ) ) ;
#15047 = CARTESIAN_POINT ( 'NONE',  ( 67.93051324133456603, 0.8441227859799155242, -16.93281709690001335 ) ) ;
#15048 = ORIENTED_EDGE ( 'NONE', *, *, #8299, .T. ) ;
#15049 = PRODUCT_DEFINITION_SHAPE ( 'NONE', 'NONE',  #45153 ) ;
#15050 = CARTESIAN_POINT ( 'NONE',  ( 121.2372526669217478, -2.334846009198419559, -18.01015021110789505 ) ) ;
#15051 = CARTESIAN_POINT ( 'NONE',  ( 112.3424481442453384, -3.505236298600246325, -18.68346056562440793 ) ) ;
#15052 = CARTESIAN_POINT ( 'NONE',  ( 127.0298367773230126, -4.565043486894647451, -18.79063384679673376 ) ) ;
#15053 = EDGE_CURVE ( 'NONE', #8854, #28999, #35063, .T. ) ;
#15054 = CARTESIAN_POINT ( 'NONE',  ( 124.1983214775786166, -1.833838273342659697, -17.42832698103878286 ) ) ;
#15055 = ORIENTED_EDGE ( 'NONE', *, *, #1346, .T. ) ;
#15056 = CARTESIAN_POINT ( 'NONE',  ( 118.2420214775786320, -3.383040157471821630, -19.15922257007629170 ) ) ;
#15057 = AXIS2_PLACEMENT_3D ( 'NONE', #43880, #2588, #34051 ) ;
#15058 = LINE ( 'NONE', #42431, #19275 ) ;
#15059 = CARTESIAN_POINT ( 'NONE',  ( 112.1155414775786454, -10.15424416112533912, -14.75197769757731336 ) ) ;
#15060 = AXIS2_PLACEMENT_3D ( 'NONE', #43465, #43238, #40264 ) ;
#15061 = DIRECTION ( 'NONE',  ( -0.9908103287288503314, 0.1352586133457956419, 0.000000000000000000 ) ) ;
#15062 = FACE_BOUND ( 'NONE', #32230, .T. ) ;
#15063 = CARTESIAN_POINT ( 'NONE',  ( 112.6260814775786514, -0.8288870151387760510, -10.36305467784173118 ) ) ;
#15064 = CARTESIAN_POINT ( 'NONE',  ( 126.3539348109119800, -4.153390946401325223, -8.397313243818185668 ) ) ;
#15065 = CARTESIAN_POINT ( 'NONE',  ( 116.6776094670037622, -8.413751147702754452, -17.03160569075142305 ) ) ;
#15066 = CARTESIAN_POINT ( 'NONE',  ( 124.8790414775786246, -8.899110576539710493, -16.42337572283490132 ) ) ;
#15067 = CARTESIAN_POINT ( 'NONE',  ( 86.50830818076254047, -21.65036132658698520, -20.89321520033831447 ) ) ;
#15068 = CARTESIAN_POINT ( 'NONE',  ( 120.6245414775786458, -9.988377603198976828, -10.36322818467138340 ) ) ;
#15069 = EDGE_CURVE ( 'NONE', #42332, #14596, #19806, .T. ) ;
#15070 = VERTEX_POINT ( 'NONE', #24195 ) ;
#15071 = CARTESIAN_POINT ( 'NONE',  ( 126.9115046738447887, -8.477094959678533215, -17.33456804528672635 ) ) ;
#15072 = CARTESIAN_POINT ( 'NONE',  ( 115.7610046295247912, -4.863998795839590272, -7.631215200338315796 ) ) ;
#15073 = CARTESIAN_POINT ( 'NONE',  ( 114.2330358795247776, -8.402594152722688392, -9.854619843455216355 ) ) ;
#15074 = CARTESIAN_POINT ( 'NONE',  ( 115.2053796295247849, -4.863998795839590272, -8.388885654883775800 ) ) ;
#15075 = CARTESIAN_POINT ( 'NONE',  ( 125.3895814775786590, -2.084020599725330491, -8.691656652583604981 ) ) ;
#15076 = CARTESIAN_POINT ( 'NONE',  ( 114.1577014775786552, -6.344957434206662583, -7.627207830600332805 ) ) ;
#15077 = EDGE_LOOP ( 'NONE', ( #14579, #5946, #35987, #24705 ) ) ;
#15078 = CARTESIAN_POINT ( 'NONE',  ( 112.9664414775786412, -9.859900752359374465, -12.68260735090039404 ) ) ;
#15079 = CARTESIAN_POINT ( 'NONE',  ( 106.5931921295248372, 0.8980012041604618078, -13.39321520033831447 ) ) ;
#15080 = FACE_OUTER_BOUND ( 'NONE', #7981, .T. ) ;
#15081 = EDGE_CURVE ( 'NONE', #3603, #7036, #22216, .T. ) ;
#15082 = CARTESIAN_POINT ( 'NONE',  ( 112.5693548109119888, 0.4262465694468514643, -12.03445270309931736 ) ) ;
#15083 = CARTESIAN_POINT ( 'NONE',  ( 123.2697102440515238, -2.467220198592778413, -17.83387418641524391 ) ) ;
#15084 = CARTESIAN_POINT ( 'NONE',  ( 66.12481753886987690, -14.57890275351189402, -16.60867411372743518 ) ) ;
#15085 = CARTESIAN_POINT ( 'NONE',  ( 115.1220548109119761, -8.166667518702817929, -8.995218007635861213 ) ) ;
#15086 = CARTESIAN_POINT ( 'NONE',  ( 110.4131140045248287, -10.62599879583958717, -11.00651665394454604 ) ) ;
#15087 = CARTESIAN_POINT ( 'NONE',  ( 109.9963952545248134, -9.868328341294098749, -15.46607636864997204 ) ) ;
#15088 = EDGE_LOOP ( 'NONE', ( #5221, #11208, #30982, #7103 ) ) ;
#15089 = DIRECTION ( 'NONE',  ( 1.000000000000000000, 0.000000000000000000, 0.000000000000000000 ) ) ;
#15090 = CARTESIAN_POINT ( 'NONE',  ( 120.4543614775786295, -5.574606645277164318, -18.38911715685844683 ) ) ;
#15091 = CARTESIAN_POINT ( 'NONE',  ( 116.8238548109119819, -4.089484607189486809, -7.948022111789456723 ) ) ;
#15092 = AXIS2_PLACEMENT_3D ( 'NONE', #16808, #20449, #9963 ) ;
#15093 = CARTESIAN_POINT ( 'NONE',  ( 111.8319081442453182, -5.638512984488999180, -18.83840828888717311 ) ) ;
#15094 = CARTESIAN_POINT ( 'NONE',  ( 125.3328548109119964, -0.8288870151387760510, -10.36305467784173118 ) ) ;
#15095 = PRODUCT_DEFINITION_CONTEXT ( 'detailed design', #18372, 'design' ) ;
#15096 = CARTESIAN_POINT ( 'NONE',  ( 123.5743281442453139, -2.084020599724406786, -8.691656652584148546 ) ) ;
#15097 = CARTESIAN_POINT ( 'NONE',  ( 115.0086014775786509, -5.574606645277164318, -18.38911715685844683 ) ) ;
#15098 = ORIENTED_EDGE ( 'NONE', *, *, #32283, .F. ) ;
#15099 = CARTESIAN_POINT ( 'NONE',  ( 120.9936110609119737, -3.163656168406935087, -18.89861972220014508 ) ) ;
#15100 = DIRECTION ( 'NONE',  ( 0.000000000000000000, -0.3818493186865927203, 0.9242245927363029745 ) ) ;
#15101 = CARTESIAN_POINT ( 'NONE',  ( 118.1852948109119836, -4.153390946401325223, -8.397313243818185668 ) ) ;
#15102 = VERTEX_POINT ( 'NONE', #20988 ) ;
#15103 = CARTESIAN_POINT ( 'NONE',  ( 94.20708369096698220, -25.14343533174585943, -14.10537061818067883 ) ) ;
#15104 = CARTESIAN_POINT ( 'NONE',  ( 113.4769814775786330, -10.63000616557722466, -14.87417383870573495 ) ) ;
#15105 = CIRCLE ( 'NONE', #20937, 1.499999999999999334 ) ;
#15106 = CARTESIAN_POINT ( 'NONE',  ( 116.1777233795247781, -8.938348069036489818, -17.46756447353520159 ) ) ;
#15107 = CARTESIAN_POINT ( 'NONE',  ( 118.7735460444391862, -1.267766418764730840, -16.93314635290706605 ) ) ;
#15108 = EDGE_LOOP ( 'NONE', ( #10127, #13234, #20910, #11013, #14680 ) ) ;
#15109 = ORIENTED_EDGE ( 'NONE', *, *, #3676, .T. ) ;
#15110 = CARTESIAN_POINT ( 'NONE',  ( 122.4397948109119767, -0.1624402480850797581, -16.17319339645315424 ) ) ;
#15111 = CARTESIAN_POINT ( 'NONE',  ( 116.7104014775786425, -8.899110576539710493, -16.42337572283490132 ) ) ;
#15112 =( BOUNDED_CURVE ( )  B_SPLINE_CURVE ( 2, ( #33299, #19636, #44048, #37412, #30133, #20103, #9379, #33520, #2300, #16230, #12812, #23288, #37172, #26932, #33988, #2528, #3649 ),
 .UNSPECIFIED., .F., .T. ) 
 B_SPLINE_CURVE_WITH_KNOTS ( ( 3, 2, 2, 2, 2, 2, 2, 2, 3 ),
 ( 0.5170046674808920217, 0.5234375000000000000, 0.5312500000000000000, 0.5390625000000000000, 0.5468750000000000000, 0.5546875000000000000, 0.5625000000000000000, 0.5703125000000000000, 0.5767453325190590174 ),
 .UNSPECIFIED. ) 
 CURVE ( )  GEOMETRIC_REPRESENTATION_ITEM ( )  RATIONAL_B_SPLINE_CURVE ( ( 0.9778625265006459788, 0.9373222120152210346, 1.000000000000000000, 0.9238795325112869605, 1.000000000000000000, 0.9238795325112869605, 1.000000000000000000, 0.9238795325112869605, 1.000000000000000000, 0.9238795325112869605, 1.000000000000000000, 0.9238795325112869605, 1.000000000000000000, 0.9238795325112869605, 1.000000000000000000, 0.9373222120157009840, 0.9778625265000250311 ) ) 
 REPRESENTATION_ITEM ( '' )  );
#15113 = CARTESIAN_POINT ( 'NONE',  ( 74.69189222814998175, -41.76310523276723785, -23.89321520033831803 ) ) ;
#15114 = ADVANCED_FACE ( 'NONE', ( #38516 ), #43831, .F. ) ;
#15115 = CARTESIAN_POINT ( 'NONE',  ( 123.0772048109119652, -7.554583864224885481, -18.48844787311982785 ) ) ;
#15116 = ORIENTED_EDGE ( 'NONE', *, *, #19193, .F. ) ;
#15117 = DIRECTION ( 'NONE',  ( -0.000000000000000000, -0.9284778069183721172, -0.3713878862591650232 ) ) ;
#15118 = CARTESIAN_POINT ( 'NONE',  ( 62.08082402252009757, -65.39425684394153393, -44.66980955559895961 ) ) ;
#15119 = CARTESIAN_POINT ( 'NONE',  ( 110.9687390045248350, 0.8980012041604421569, -15.77991374673208469 ) ) ;
#15120 = CIRCLE ( 'NONE', #6410, 1.587499999999998579 ) ;
#15121 = CARTESIAN_POINT ( 'NONE',  ( 114.2144281442453178, -8.166667518702817929, -8.995218007635859436 ) ) ;
#15122 = CARTESIAN_POINT ( 'NONE',  ( 125.2194014775786286, 0.1319031606808879209, -14.10382304977623669 ) ) ;
#15123 = CARTESIAN_POINT ( 'NONE',  ( 121.1350814775786233, -9.859900752359378018, -12.68260735090039759 ) ) ;
#15124 = LINE ( 'NONE', #18769, #15283 ) ;
#15125 = ORIENTED_EDGE ( 'NONE', *, *, #36224, .F. ) ;
#15126 = CARTESIAN_POINT ( 'NONE',  ( 119.5467348109119712, -5.574606645277164318, -18.38911715685844683 ) ) ;
#15127 = CARTESIAN_POINT ( 'NONE',  ( 116.3166296295247832, -4.863998795839590272, -19.15521520033831493 ) ) ;
#15128 = DIRECTION ( 'NONE',  ( 0.9609149988134837450, -0.1028163501681639419, 0.2570431154366518145 ) ) ;
#15129 = CARTESIAN_POINT ( 'NONE',  ( 114.5108483795247878, -0.7896495226426338832, -9.318865927141430916 ) ) ;
#15130 = EDGE_CURVE ( 'NONE', #34894, #37401, #38748, .T. ) ;
#15131 = CARTESIAN_POINT ( 'NONE',  ( 119.4900081442453086, -1.834011780172310813, -8.268836392978581529 ) ) ;
#15132 = ORIENTED_EDGE ( 'NONE', *, *, #32799, .F. ) ;
#15133 = CARTESIAN_POINT ( 'NONE',  ( 115.5758681442453053, -1.561330072975668060, -17.79121239304076951 ) ) ;
#15134 = CARTESIAN_POINT ( 'NONE',  ( 115.4100314811013561, -2.280480477428491248, -18.08254604495227724 ) ) ;
#15135 = CARTESIAN_POINT ( 'NONE',  ( 105.6903015045248253, -2.477300249445798297, -7.631215200338321125 ) ) ;
#15136 = CARTESIAN_POINT ( 'NONE',  ( 117.5045748109119756, 0.5811942927096110934, -14.16772938898807510 ) ) ;
#15137 = CARTESIAN_POINT ( 'NONE',  ( 116.3133148109119759, -7.893985811506177619, -18.51759400769804742 ) ) ;
#15138 = CARTESIAN_POINT ( 'NONE',  ( 126.2184548109108135, -9.830300164702144627, -12.80248346511802104 ) ) ;
#15139 = CARTESIAN_POINT ( 'NONE',  ( 117.1464118195297601, -11.22028320508336563, -5.522660250078516242 ) ) ;
#15140 = DIRECTION ( 'NONE',  ( 0.9609149988134843001, -0.1028163501681632064, 0.2570431154366505933 ) ) ;
#15141 = EDGE_LOOP ( 'NONE', ( #3043, #37982, #44866, #21265 ) ) ;
#15142 = CARTESIAN_POINT ( 'NONE',  ( 112.1218600025837304, -2.311015703046748193, -18.04188382666269064 ) ) ;
#15143 = CARTESIAN_POINT ( 'NONE',  ( 109.2292946956953159, -9.680038410784433722, -10.31160768788000937 ) ) ;
#15144 = CARTESIAN_POINT ( 'NONE',  ( 119.3765548109119834, -10.15424416112533912, -14.75197769757731336 ) ) ;
#15145 = CARTESIAN_POINT ( 'NONE',  ( 112.9828796295247884, -4.863998795839590272, -8.388885654883775800 ) ) ;
#15146 = CARTESIAN_POINT ( 'NONE',  ( 106.4542858795248179, -0.7896495226426338832, -17.46756447353520159 ) ) ;
#15147 = CARTESIAN_POINT ( 'NONE',  ( 112.7962614775786676, -6.222761293078241884, -8.102969835052219238 ) ) ;
#15148 = CARTESIAN_POINT ( 'NONE',  ( 115.0086014775786509, -5.574606645277164318, -18.38911715685844683 ) ) ;
#15149 = DIRECTION ( 'NONE',  ( 1.000000000000000000, 0.000000000000000000, -0.000000000000000000 ) ) ;
#15150 = CARTESIAN_POINT ( 'NONE',  ( 124.1983214775786166, -8.166667518702819706, -8.995218007635861213 ) ) ;
#15151 = CARTESIAN_POINT ( 'NONE',  ( 121.1918081442452859, 0.9020085738987339008, -11.91225656197089222 ) ) ;
#15152 = ORIENTED_EDGE ( 'NONE', *, *, #15652, .F. ) ;
#15153 = CARTESIAN_POINT ( 'NONE',  ( 119.6034614775786196, -3.505236298600246325, -18.68346056562440793 ) ) ;
#15154 = CARTESIAN_POINT ( 'NONE',  ( 126.2404814775786264, -9.261995988541697145, -16.69588392320189030 ) ) ;
#15156 = EDGE_CURVE ( 'NONE', #37616, #36955, #13271, .T. ) ;
#15155 = CARTESIAN_POINT ( 'NONE',  ( 122.2128881442453263, -1.834011780172310813, -8.268836392978581529 ) ) ;
#15157 = CARTESIAN_POINT ( 'NONE',  ( 119.6034614775786196, -3.505236298600246325, -18.68346056562440793 ) ) ;
#15158 = EDGE_LOOP ( 'NONE', ( #17802, #41972, #13980, #41905 ) ) ;
#15159 = CARTESIAN_POINT ( 'NONE',  ( 116.0506660444391969, -1.267766418764730840, -16.93314635290706605 ) ) ;
#15160 = CARTESIAN_POINT ( 'NONE',  ( 121.5888948109119809, -10.30919188438810075, -12.61870101168855918 ) ) ;
#15161 = CARTESIAN_POINT ( 'NONE',  ( 116.9163235773848726, -2.467220198592778413, -17.83387418641524391 ) ) ;
#15162 = DIRECTION ( 'NONE',  ( 0.000000000000000000, 0.000000000000000000, 1.000000000000000000 ) ) ;
#15163 = CARTESIAN_POINT ( 'NONE',  ( 126.4144288373559846, 0.2303623831909507591, -13.58551579586932156 ) ) ;
#15164 = CARTESIAN_POINT ( 'NONE',  ( 113.9552233795247815, -1.325403438956436419, -9.854619843455211026 ) ) ;
#15165 = CARTESIAN_POINT ( 'NONE',  ( 116.7104014775786425, -0.4660016031367893996, -10.09054647747474043 ) ) ;
#15166 = DIRECTION ( 'NONE',  ( -0.9970811988817435134, 0.07634843047859724008, 0.000000000000000000 ) ) ;
#15167 = CARTESIAN_POINT ( 'NONE',  ( 117.1642148109119859, -0.8288870151387760510, -10.36305467784173118 ) ) ;
#15168 = CARTESIAN_POINT ( 'NONE',  ( 124.8790414775786246, -0.4660016031367893996, -10.09054647747474043 ) ) ;
#15169 = CARTESIAN_POINT ( 'NONE',  ( 126.2184548109105435, -0.8658195297460520301, -10.39078908864422246 ) ) ;
#15170 = CARTESIAN_POINT ( 'NONE',  ( -13.60420442504482175, -3.877746523608537554, -8.129294934689871965 ) ) ;
#15171 = CARTESIAN_POINT ( 'NONE',  ( 112.0799890045248475, -9.868328341294098749, -11.32035403202665869 ) ) ;
#15172 = CARTESIAN_POINT ( 'NONE',  ( 112.8529881442453302, -7.894159318335828068, -9.358103419637847864 ) ) ;
#15173 = DIRECTION ( 'NONE',  ( 1.000000000000000000, 0.000000000000000000, -0.000000000000000000 ) ) ;
#15174 = CARTESIAN_POINT ( 'NONE',  ( 94.20708369096698220, -24.88943055980569241, -13.49371108670732333 ) ) ;
#15176 = CARTESIAN_POINT ( 'NONE',  ( 118.1852948109119836, -5.638512984488999180, -18.83840828888717311 ) ) ;
#15175 = CARTESIAN_POINT ( 'NONE',  ( 64.18188758151919160, -15.10253999624987742, -8.768039431438440445 ) ) ;
#15177 = B_SPLINE_CURVE_WITH_KNOTS ( 'NONE', 3,
 ( #27498, #41418, #23397, #10172, #37972, #34534, #40502, #3312, #31126, #34094 ),
 .UNSPECIFIED., .F., .F.,
 ( 4, 3, 3, 4 ),
 ( 0.000000000000000000, 0.0002476486447138720221, 0.0004952972925464089841, 0.0009604418836934709670 ),
 .UNSPECIFIED. ) ;
#15178 = EDGE_CURVE ( 'NONE', #16620, #15181, #31463, .T. ) ;
#15179 = VECTOR ( 'NONE', #3624, 1000.000000000000000 ) ;
#15180 = CARTESIAN_POINT ( 'NONE',  ( 122.7801548109119665, -6.222761293078241884, -8.102969835052219238 ) ) ;
#15181 = VERTEX_POINT ( 'NONE', #31022 ) ;
#15182 = DIRECTION ( 'NONE',  ( 0.000000000000000000, 0.000000000000000000, -1.000000000000000000 ) ) ;
#15183 = CARTESIAN_POINT ( 'NONE',  ( 126.2184548109119788, 0.08617673920515746266, -14.09731900820182915 ) ) ;
#15184 = CARTESIAN_POINT ( 'NONE',  ( 112.2883483795247770, -8.402594152722688392, -16.93181055722141792 ) ) ;
#15185 = CARTESIAN_POINT ( 'NONE',  ( 120.6245414775786458, -0.1624402480850797581, -16.17319339645315424 ) ) ;
#15186 = CARTESIAN_POINT ( 'NONE',  ( 120.5110881442453206, -3.505236298600246325, -18.68346056562440793 ) ) ;
#15187 = CARTESIAN_POINT ( 'NONE',  ( 115.6325948109119821, -9.565557343593413364, -10.61323700422348004 ) ) ;
#15188 = CARTESIAN_POINT ( 'NONE',  ( 85.68405335838919257, -28.00027651839989318, -8.921533853845815543 ) ) ;
#15189 = CARTESIAN_POINT ( 'NONE',  ( 109.2324108795247923, -8.938348069036489818, -9.318865927141430916 ) ) ;
#15190 = CARTESIAN_POINT ( 'NONE',  ( 122.9503348109119827, -9.859900752359378018, -12.68260735090039759 ) ) ;
#15191 = CARTESIAN_POINT ( 'NONE',  ( 124.4819548109119722, -2.084020599724406786, -8.691656652584148546 ) ) ;
#15192 = DIRECTION ( 'NONE',  ( -0.7298031939408690105, -0.6836572958096084340, 0.000000000000000000 ) ) ;
#15193 = FACE_OUTER_BOUND ( 'NONE', #8017, .T. ) ;
#15194 = CARTESIAN_POINT ( 'NONE',  ( 123.8411891859119862, -8.844754642576884152, -8.592115655440050404 ) ) ;
#15195 = CARTESIAN_POINT ( 'NONE',  ( 114.1635827545248389, -2.477300249445798297, -19.15521520033831138 ) ) ;
#15196 =( BOUNDED_SURFACE ( )  B_SPLINE_SURFACE ( 3, 2, ( 
 ( #30025, #24534, #27963 ),
 ( #3548, #41433, #3110 ),
 ( #10630, #20675, #2883 ),
 ( #41207, #41653, #34979 ),
 ( #37765, #40984, #16812 ),
 ( #17463, #21100, #34552 ) ),
 .UNSPECIFIED., .F., .F., .F. ) 
 B_SPLINE_SURFACE_WITH_KNOTS ( ( 4, 2, 4 ),
 ( 3, 3 ),
 ( 3.899122207871039691, 4.305755594127865571, 4.712388980384689674 ),
 ( 0.000000000000000000, 1.000000000000000000 ),
 .UNSPECIFIED. ) 
 GEOMETRIC_REPRESENTATION_ITEM ( )  RATIONAL_B_SPLINE_SURFACE ( (
 ( 1.000000000000000000, 0.5507912154400889104, 1.000000000000000000),
 ( 1.000000000000000000, 0.5736970358664340575, 1.000000000000000000),
 ( 1.000000000000000000, 0.5999889691994200192, 1.000000000000000000),
 ( 1.000000000000000000, 0.6537365690953489406, 1.000000000000000000),
 ( 1.000000000000000000, 0.6811922875906900599, 1.000000000000000000),
 ( 1.000000000000000000, 0.7071067811865480168, 1.000000000000000000) ) ) 
 REPRESENTATION_ITEM ( '' )  SURFACE ( )  );
#15197 = CARTESIAN_POINT ( 'NONE',  ( -13.42620672024982476, -3.955390967436159588, -18.90065854372406662 ) ) ;
#15198 = CARTESIAN_POINT ( 'NONE',  ( 82.47484345711939113, -31.70193537549793916, -22.53651891743845681 ) ) ;
#15199 = CARTESIAN_POINT ( 'NONE',  ( 117.3911214775786505, -1.561330072975668504, -17.79121239304076951 ) ) ;
#15200 = CARTESIAN_POINT ( 'NONE',  ( 118.6391081442452986, -4.089484607189486809, -7.948022111789456723 ) ) ;
#15201 = CARTESIAN_POINT ( 'NONE',  ( 107.8433483795247838, -0.7896495226426338832, -9.318865927141430916 ) ) ;
#15202 = DIRECTION ( 'NONE',  ( -0.000000000000000000, -0.9284778069183721172, -0.3713878862591650232 ) ) ;
#15203 = CARTESIAN_POINT ( 'NONE',  ( 90.45092582798827152, -25.99489077589524300, -13.39321520033831625 ) ) ;
#15204 = EDGE_LOOP ( 'NONE', ( #41744, #6704, #33473, #35807 ) ) ;
#15205 = DIRECTION ( 'NONE',  ( -0.9908103287288497762, 0.1352586133458010265, 0.000000000000000000 ) ) ;
#15206 = CARTESIAN_POINT ( 'NONE',  ( 118.1852948109119836, -5.638512984488999180, -18.83840828888717311 ) ) ;
#15207 = CARTESIAN_POINT ( 'NONE',  ( 122.6099748109119929, -0.8288870151387760510, -10.36305467784173118 ) ) ;
#15208 = APPLICATION_PROTOCOL_DEFINITION ( 'draft international standard', 'automotive_design', 1998, #25371 ) ;
#15209 = CARTESIAN_POINT ( 'NONE',  ( 115.1220548109119761, -1.833838273342658809, -17.42832698103878286 ) ) ;
#15210 = CARTESIAN_POINT ( 'NONE',  ( 120.0572748109119772, -3.383040157471821630, -19.15922257007629170 ) ) ;
#15211 = CARTESIAN_POINT ( 'NONE',  ( 112.7745202545247878, -10.62599879583958717, -15.77991374673208469 ) ) ;
#15212 = CARTESIAN_POINT ( 'NONE',  ( 114.8384214775786489, -10.15424416112533912, -14.75197769757731336 ) ) ;
#15213 = CARTESIAN_POINT ( 'NONE',  ( 116.8234308633710441, -1.692850972744459392, -17.55092091510499230 ) ) ;
#15214 = DIRECTION ( 'NONE',  ( 0.8636456077245088236, -0.5040994586965589219, 0.000000000000000000 ) ) ;
#15215 = VERTEX_POINT ( 'NONE', #231 ) ;
#15216 = CARTESIAN_POINT ( 'NONE',  ( 120.8547048109119686, -2.527210466738041728, -8.967976844669124148 ) ) ;
#15217 = CARTESIAN_POINT ( 'NONE',  ( 117.8449348109119938, -8.166667518702817929, -8.995218007635861213 ) ) ;
#15218 = ORIENTED_EDGE ( 'NONE', *, *, #33363, .F. ) ;
#15219 = DIRECTION ( 'NONE',  ( -0.3445294493088594256, -0.9387755102040817867, 0.000000000000000000 ) ) ;
#15220 = LINE ( 'NONE', #29127, #34022 ) ;
#15221 = CARTESIAN_POINT ( 'NONE',  ( 64.91709923316010133, -47.16693275175630617, -12.39321520033831447 ) ) ;
#15222 = CARTESIAN_POINT ( 'NONE',  ( 114.1577014775786552, -3.505236298600246325, -18.68346056562440793 ) ) ;
#15223 = CARTESIAN_POINT ( 'NONE',  ( 112.1155414775786596, 0.9020085738987339008, -11.91225656197089222 ) ) ;
#15224 = CARTESIAN_POINT ( 'NONE',  ( 64.01282776924010420, -34.86145050234441811, -5.893215200338315363 ) ) ;
#15225 = CARTESIAN_POINT ( 'NONE',  ( 123.6877814775786533, -6.222761293078241884, -8.102969835052219238 ) ) ;
#15226 = DIRECTION ( 'NONE',  ( 1.000000000000000000, 0.000000000000000000, -0.000000000000000000 ) ) ;
#15227 = DIRECTION ( 'NONE',  ( 0.1352586133457954198, 0.9908103287288503314, 0.000000000000000000 ) ) ;
#15228 = CARTESIAN_POINT ( 'NONE',  ( 124.1188183746285887, -11.97333064901767763, -17.04775611777621336 ) ) ;
#15229 = CARTESIAN_POINT ( 'NONE',  ( 124.5954081442453116, -6.222761293078241884, -8.102969835052219238 ) ) ;
#15230 = CARTESIAN_POINT ( 'NONE',  ( 113.4769814775786330, -10.63000616557722466, -14.87417383870573495 ) ) ;
#15231 = CARTESIAN_POINT ( 'NONE',  ( 118.1285681442453068, -7.893985811506177619, -18.51759400769804742 ) ) ;
#15232 = CARTESIAN_POINT ( 'NONE',  ( 112.9097148109120070, 0.2603800115204892296, -16.42320221600525088 ) ) ;
#15233 = CARTESIAN_POINT ( 'NONE',  ( 92.32016463086877422, -25.99489077589524300, -13.39321520033831447 ) ) ;
#15234 = CARTESIAN_POINT ( 'NONE',  ( 120.2841814775786276, -10.15424416112533912, -14.75197769757731336 ) ) ;
#15235 = ORIENTED_EDGE ( 'NONE', *, *, #34761, .T. ) ;
#15236 = CARTESIAN_POINT ( 'NONE',  ( 120.0005481442453146, -5.638512984488999180, -18.83840828888717311 ) ) ;
#15237 = CARTESIAN_POINT ( 'NONE',  ( 109.1629577545248395, -2.791137627527939813, -18.39754474579286025 ) ) ;
#15238 = CARTESIAN_POINT ( 'NONE',  ( 114.8581140045248361, 0.1403307496149616695, -15.46607636864997204 ) ) ;
#15239 = EDGE_CURVE ( 'NONE', #12976, #41351, #30803, .T. ) ;
#15240 = CARTESIAN_POINT ( 'NONE',  ( 83.48413635955418499, -32.78863198505981558, -23.89321520033831803 ) ) ;
#15241 = CARTESIAN_POINT ( 'NONE',  ( 113.9307948109119764, -10.15424416112533912, -14.75197769757731336 ) ) ;
#15242 = CARTESIAN_POINT ( 'NONE',  ( 120.7157985609119635, -10.36940331770106916, -15.09355782777062061 ) ) ;
#15243 = CARTESIAN_POINT ( 'NONE',  ( 116.3860827545247787, -6.936859964151250502, -8.388885654883777576 ) ) ;
#15244 = VERTEX_POINT ( 'NONE', #10953 ) ;
#15245 = VECTOR ( 'NONE', #41839, 1000.000000000000000 ) ;
#15246 = CARTESIAN_POINT ( 'NONE',  ( 121.9292548109119849, -7.894159318335828068, -9.358103419637847864 ) ) ;
#15247 = CARTESIAN_POINT ( 'NONE',  ( 120.2296266859119953, -0.06289925094097943703, -9.412459353600674206 ) ) ;
#15248 = CARTESIAN_POINT ( 'NONE',  ( 120.4379860609119675, -6.564341423271550902, -7.887810678476487425 ) ) ;
#15249 = PLANE ( 'NONE',  #18080 ) ;
#15250 = EDGE_CURVE ( 'NONE', #25472, #18453, #19080, .T. ) ;
#15251 = CARTESIAN_POINT ( 'NONE',  ( 106.7320983795247855, -8.402594152722688392, -16.93181055722141792 ) ) ;
#15252 = ORIENTED_EDGE ( 'NONE', *, *, #15526, .T. ) ;
#15253 = CARTESIAN_POINT ( 'NONE',  ( 116.1431348109119881, -10.30919188438810075, -12.61870101168855918 ) ) ;
#15254 = CARTESIAN_POINT ( 'NONE',  ( 88.35915213937708756, -11.54718831182111849, -13.65586429604254626 ) ) ;
#15255 = CARTESIAN_POINT ( 'NONE',  ( 119.2631014775786298, -9.565557343593413364, -10.61323700422348004 ) ) ;
#15256 = CARTESIAN_POINT ( 'NONE',  ( 126.3230600034167850, -3.769654384711456085, -8.460624569279659113 ) ) ;
#15257 = DIRECTION ( 'NONE',  ( 0.000000000000000000, 0.000000000000000000, 1.000000000000000000 ) ) ;
#15258 = FACE_OUTER_BOUND ( 'NONE', #38026, .T. ) ;
#15259 = DIRECTION ( 'NONE',  ( 0.000000000000000000, -0.3818493186865927203, 0.9242245927363029745 ) ) ;
#15260 = ORIENTED_EDGE ( 'NONE', *, *, #17247, .T. ) ;
#15261 = DIRECTION ( 'NONE',  ( -1.000000000000000000, 0.000000000000000000, 0.000000000000000000 ) ) ;
#15262 = CARTESIAN_POINT ( 'NONE',  ( 119.0929214775786278, -5.638512984488999180, -18.83840828888717311 ) ) ;
#15263 = ORIENTED_EDGE ( 'NONE', *, *, #6178, .T. ) ;
#15264 = EDGE_CURVE ( 'NONE', #42627, #21157, #13710, .T. ) ;
#15265 = CARTESIAN_POINT ( 'NONE',  ( 114.9518748109119883, -1.834011780172310813, -8.268836392978581529 ) ) ;
#15266 = EDGE_CURVE ( 'NONE', #37005, #33098, #26342, .T. ) ;
#15267 = EDGE_CURVE ( 'NONE', #8254, #27006, #32151, .T. ) ;
#15268 = CARTESIAN_POINT ( 'NONE',  ( 125.5597614775786326, -1.561330072975669392, -17.79121239304076951 ) ) ;
#15269 = CARTESIAN_POINT ( 'NONE',  ( 110.9687390045248208, -9.868328341294150263, -11.32035403202671553 ) ) ;
#15270 = CARTESIAN_POINT ( 'NONE',  ( 124.8223148109119762, -10.15424416112533912, -14.75197769757731336 ) ) ;
#15271 = ORIENTED_EDGE ( 'NONE', *, *, #6417, .F. ) ;
#15272 = CARTESIAN_POINT ( 'NONE',  ( 116.7104014775786425, -0.4660016031367893996, -10.09054647747474043 ) ) ;
#15273 = AXIS2_PLACEMENT_3D ( 'NONE', #31264, #25108, #17158 ) ;
#15274 = FACE_OUTER_BOUND ( 'NONE', #2982, .T. ) ;
#15275 = FACE_OUTER_BOUND ( 'NONE', #42861, .T. ) ;
#15276 = DIRECTION ( 'NONE',  ( -0.9609149988134837450, 0.1028163501681639419, -0.2570431154366518145 ) ) ;
#15277 = CARTESIAN_POINT ( 'NONE',  ( 136.0320772899192718, -5.573080998308148182, -7.524869074880469633 ) ) ;
#15278 = CARTESIAN_POINT ( 'NONE',  ( 112.6260814775786514, -0.8288870151387760510, -10.36305467784173118 ) ) ;
#15279 = CARTESIAN_POINT ( 'NONE',  ( 123.0204673576684797, -6.302457937304696500, -18.83702152638931082 ) ) ;
#15280 = AXIS2_PLACEMENT_3D ( 'NONE', #13583, #27493, #20652 ) ;
#15281 = CARTESIAN_POINT ( 'NONE',  ( 81.52050388106540879, 0.5255923868638483487, -10.89321520033831447 ) ) ;
#15282 = CARTESIAN_POINT ( 'NONE',  ( 112.3991748109119868, -1.833838273342658809, -17.42832698103878286 ) ) ;
#15283 = VECTOR ( 'NONE', #32658, 1000.000000000000000 ) ;
#15284 = CARTESIAN_POINT ( 'NONE',  ( 125.9001214775786224, -5.574606645277164318, -18.38911715685844683 ) ) ;
#15285 = CARTESIAN_POINT ( 'NONE',  ( 120.4379860609119675, -3.387241619883791355, -18.17469012370385073 ) ) ;
#15286 = CARTESIAN_POINT ( 'NONE',  ( 124.2550481442452792, -0.1624402480850797581, -16.17319339645315424 ) ) ;
#15287 = CARTESIAN_POINT ( 'NONE',  ( 92.32016463086877422, -25.23119213852205789, -15.24166438581092109 ) ) ;
#15288 = CARTESIAN_POINT ( 'NONE',  ( 120.1707281442453166, 0.2603800115204892296, -16.42320221600525088 ) ) ;
#15289 = ORIENTED_EDGE ( 'NONE', *, *, #31486, .F. ) ;
#15290 = CARTESIAN_POINT ( 'NONE',  ( 126.8137406968053114, -8.488853573463353896, -17.25709863353327833 ) ) ;
#15291 = CARTESIAN_POINT ( 'NONE',  ( 116.0388171295248014, -10.62599879583958540, -13.39321520033831447 ) ) ;
#15292 = EDGE_CURVE ( 'NONE', #31941, #21796, #4770, .T. ) ;
#15293 = CARTESIAN_POINT ( 'NONE',  ( 110.4825671295247815, 0.1403307496149613920, -13.39321520033831447 ) ) ;
#15294 = CARTESIAN_POINT ( 'NONE',  ( 108.8851452545248151, -9.868328341294098749, -15.46607636864997204 ) ) ;
#15295 = CARTESIAN_POINT ( 'NONE',  ( 125.6059481442453318, -7.866424907534184996, -9.395035934245763443 ) ) ;
#15296 = CARTESIAN_POINT ( 'NONE',  ( 116.0296814775786345, -8.166667518702817929, -8.995218007635861213 ) ) ;
#15297 = ORIENTED_EDGE ( 'NONE', *, *, #17407, .T. ) ;
#15298 = CARTESIAN_POINT ( 'NONE',  ( 116.8805814775786445, -3.505236298600246325, -18.68346056562440793 ) ) ;
#15299 = CARTESIAN_POINT ( 'NONE',  ( 108.5378796295247810, -4.863998795839590272, -19.15521520033831493 ) ) ;
#15300 = CARTESIAN_POINT ( 'NONE',  ( 70.19189222814998175, -67.83330054016514055, -40.33609291459782753 ) ) ;
#15301 = CARTESIAN_POINT ( 'NONE',  ( 111.2646643879000834, -8.898622535612265239, -16.42406377531225914 ) ) ;
#15302 = DIRECTION ( 'NONE',  ( 0.000000000000000000, 0.4669533266896293000, 0.8842819633428516957 ) ) ;
#15303 = CARTESIAN_POINT ( 'NONE',  ( 64.51132457273423881, -13.77492255257581455, -17.92675206381565189 ) ) ;
#15304 = CARTESIAN_POINT ( 'NONE',  ( 117.3911214775786505, -1.561330072975668504, -17.79121239304076951 ) ) ;
#15305 = EDGE_CURVE ( 'NONE', #10182, #511, #1126, .T. ) ;
#15306 = CARTESIAN_POINT ( 'NONE',  ( 109.3713171295247832, -10.62599879583958540, -13.39321520033831447 ) ) ;
#15307 = CARTESIAN_POINT ( 'NONE',  ( 113.7468640045248236, 0.1403307496149616695, -15.46607636864997204 ) ) ;
#15308 = ORIENTED_EDGE ( 'NONE', *, *, #28952, .F. ) ;
#15309 = LINE ( 'NONE', #39708, #33230 ) ;
#15310 = CARTESIAN_POINT ( 'NONE',  ( 118.2987481442453088, -7.894159318335828068, -9.358103419637847864 ) ) ;
#15311 = CARTESIAN_POINT ( 'NONE',  ( 115.8595014775786609, -1.834011780172310813, -8.268836392978581529 ) ) ;
#15312 = CONICAL_SURFACE ( 'NONE', #720, 2.000000000000000444, 0.9599310885968830309 ) ;
#15313 = DIRECTION ( 'NONE',  ( 0.9609149988134837450, -0.1028163501681639419, 0.2570431154366518145 ) ) ;
#15314 = CARTESIAN_POINT ( 'NONE',  ( 123.4041481442452834, 0.1319031606808879209, -14.10382304977623669 ) ) ;
#15315 = CARTESIAN_POINT ( 'NONE',  ( 125.1059481442452750, -1.833838273342660141, -17.42832698103878286 ) ) ;
#15316 = CARTESIAN_POINT ( 'NONE',  ( 116.7104014775786425, -8.899110576539710493, -16.42337572283490132 ) ) ;
#15317 = ORIENTED_EDGE ( 'NONE', *, *, #24542, .F. ) ;
#15318 = CARTESIAN_POINT ( 'NONE',  ( 124.6051735609119646, -9.645473719204776586, -14.86997237629376656 ) ) ;
#15319 = CIRCLE ( 'NONE', #19680, 15.90000000000000036 ) ;
#15320 = CARTESIAN_POINT ( 'NONE',  ( 119.7434548109119703, 2.768327990826033425, -17.42353644532102308 ) ) ;
#15321 = CARTESIAN_POINT ( 'NONE',  ( 117.5045748109119756, -9.859900752359374465, -12.68260735090039404 ) ) ;
#15322 = ORIENTED_EDGE ( 'NONE', *, *, #7754, .T. ) ;
#15323 = AXIS2_PLACEMENT_3D ( 'NONE', #28187, #30932, #41872 ) ;
#15324 = FACE_OUTER_BOUND ( 'NONE', #29838, .T. ) ;
#15325 = ADVANCED_FACE ( 'NONE', ( #7973 ), #18906, .F. ) ;
#15326 = CARTESIAN_POINT ( 'NONE',  ( 114.6115148109119986, -3.383040157471821630, -19.15922257007629170 ) ) ;
#15327 = CARTESIAN_POINT ( 'NONE',  ( 106.5237390045248418, -9.868328341294098749, -11.32035403202665869 ) ) ;
#15328 = CARTESIAN_POINT ( 'NONE',  ( 113.9307948109119764, -10.15424416112533912, -14.75197769757731336 ) ) ;
#15329 = ORIENTED_EDGE ( 'NONE', *, *, #15945, .T. ) ;
#15330 = ORIENTED_EDGE ( 'NONE', *, *, #12505, .T. ) ;
#15331 = CARTESIAN_POINT ( 'NONE',  ( 121.9292548109119849, -7.894159318335828068, -9.358103419637847864 ) ) ;
#15332 = CARTESIAN_POINT ( 'NONE',  ( 117.4478481442453131, -9.565557343593413364, -10.61323700422348004 ) ) ;
#15333 = ADVANCED_FACE ( 'NONE', ( #14592 ), #35465, .T. ) ;
#15334 = DIRECTION ( 'NONE',  ( -0.9908103287288504424, 0.1352586133457950868, 0.000000000000000000 ) ) ;
#15335 = CARTESIAN_POINT ( 'NONE',  ( 116.3700414775786527, -4.153390946401313677, -8.397313243818183892 ) ) ;
#15336 = EDGE_LOOP ( 'NONE', ( #24663, #12156 ) ) ;
#15337 = DIRECTION ( 'NONE',  ( 1.000000000000000000, 0.000000000000000000, 0.000000000000000000 ) ) ;
#15338 = CARTESIAN_POINT ( 'NONE',  ( 71.02242295334774269, -99.02728775972636299, -55.91838671430374319 ) ) ;
#15339 = CARTESIAN_POINT ( 'NONE',  ( 111.3160046295247838, -4.863998795839590272, -7.631215200338315796 ) ) ;
#15340 = CIRCLE ( 'NONE', #16798, 5.000000000000000888 ) ;
#15341 = CARTESIAN_POINT ( 'NONE',  ( 117.2209414775786485, -7.893985811506177619, -18.51759400769804742 ) ) ;
#15343 = CARTESIAN_POINT ( 'NONE',  ( 114.7816948109119863, -9.859900752359374465, -12.68260735090039404 ) ) ;
#15342 = CARTESIAN_POINT ( 'NONE',  ( 125.6164881442453094, -9.565557343593413364, -10.61323700422348004 ) ) ;
#15344 = CARTESIAN_POINT ( 'NONE',  ( 122.9503348109119827, -9.859900752359378018, -12.68260735090039759 ) ) ;
#15345 = CARTESIAN_POINT ( 'NONE',  ( 112.4201593777725208, -1.267766418764741276, -16.93314635290707315 ) ) ;
#15346 = ORIENTED_EDGE ( 'NONE', *, *, #22024, .T. ) ;
#15347 = CARTESIAN_POINT ( 'NONE',  ( 119.3198281442452924, -9.859900752359374465, -12.68260735090039404 ) ) ;
#15348 = B_SPLINE_CURVE_WITH_KNOTS ( 'NONE', 3,
 ( #30214, #26113, #6031, #27025, #33379, #16770, #43902, #29756, #37259, #40940, #12670, #2610, #44358, #43668, #2384, #9018, #22916, #37496 ),
 .UNSPECIFIED., .F., .F.,
 ( 4, 2, 2, 1, 1, 1, 1, 2, 2, 2, 4 ),
 ( 0.000000000000000000, 0.2500000000003136380, 0.3750000000004710121, 0.4375000000005498935, 0.4687500000005943024, 0.4843750000006165068, 0.4921875000006225020, 0.4960937500006203926, 0.5000000000006181722, 0.7500000000003090861, 1.000000000000000000 ),
 .UNSPECIFIED. ) ;
#15349 = CARTESIAN_POINT ( 'NONE',  ( 124.1983214775786166, -1.833838273342659697, -17.42832698103878286 ) ) ;
#15350 = CARTESIAN_POINT ( 'NONE',  ( 112.7745202545247878, -10.62599879583958717, -15.77991374673208469 ) ) ;
#15351 = VECTOR ( 'NONE', #26364, 1000.000000000000000 ) ;
#15352 = CARTESIAN_POINT ( 'NONE',  ( 116.8722546295247895, -4.863998795839590272, -18.39754474579285315 ) ) ;
#15353 = CARTESIAN_POINT ( 'NONE',  ( 115.4831921295247952, 0.8980012041604618078, -13.39321520033831447 ) ) ;
#15354 = B_SPLINE_CURVE_WITH_KNOTS ( 'NONE', 3,
 ( #31173, #23042, #33502, #2281, #41236, #16211, #30113, #44029, #34359, #17062, #21808, #38671, #14074, #609, #7670, #7011, #828, #17941, #42346, #31840, #1054, #7901, #10660, #14970, #42565, #35472, #42794, #10882, #18164, #17490, #28882, #7221, #35702, #42122, #24780, #14520, #27992, #39134, #14296, #4477, #4247, #25006, #38900, #21585, #34795, #11104, #32061, #28433, #14748, #28660, #24564, #11327, #7438, #25237, #21359, #24345, #18397, #32290, #38230, #20920, #21134, #3578, #31388, #158, #35009, #41897 ),
 .UNSPECIFIED., .F., .F.,
 ( 4, 2, 2, 1, 1, 2, 2, 2, 2, 2, 2, 2, 1, 1, 2, 2, 2, 2, 1, 1, 2, 2, 2, 2, 2, 2, 1, 1, 1, 2, 2, 2, 2, 1, 1, 1, 2, 2, 4 ),
 ( 0.000000000000000000, 0.06249999999999879263, 0.09374999999999800160, 0.1093749999999975991, 0.1171874999999972244, 0.1210937499999972106, 0.1249999999999972106, 0.1874999999999967248, 0.2187499999999965861, 0.2499999999999963918, 0.3124999999999960587, 0.3437499999999958922, 0.3593749999999957256, 0.3671874999999955036, 0.3710937499999953926, 0.3749999999999952260, 0.4374999999999928391, 0.4687499999999916733, 0.4843749999999909517, 0.4921874999999907296, 0.4960937499999905631, 0.4999999999999904521, 0.5624999999999886757, 0.6249999999999868994, 0.6874999999999851230, 0.7187499999999844569, 0.7343749999999841238, 0.7421874999999840128, 0.7460937499999840128, 0.7480468749999841238, 0.7499999999999842348, 0.8124999999999881206, 0.8437499999999902300, 0.8593749999999914513, 0.8671874999999922284, 0.8710937499999925615, 0.8730468749999927836, 0.8749999999999930056, 1.000000000000000000 ),
 .UNSPECIFIED. ) ;
#15355 = CARTESIAN_POINT ( 'NONE',  ( 117.7882081442453170, -6.344957434206665248, -7.627207830600338134 ) ) ;
#15356 = ORIENTED_EDGE ( 'NONE', *, *, #8613, .F. ) ;
#15357 = AXIS2_PLACEMENT_3D ( 'NONE', #27765, #15756, #27545 ) ;
#15358 = CARTESIAN_POINT ( 'NONE',  ( 120.0572748109119772, -3.383040157471821630, -19.15922257007629170 ) ) ;
#15359 = DIRECTION ( 'NONE',  ( -0.4461977533474357216, -0.8271203734159379151, -0.3417300876246930907 ) ) ;
#15360 = CARTESIAN_POINT ( 'NONE',  ( 108.8851452545248151, 0.8980012041604421569, -11.00651665394454071 ) ) ;
#15361 = CARTESIAN_POINT ( 'NONE',  ( 114.7816948109119863, 0.5811942927096154232, -14.16772938898807155 ) ) ;
#15362 = CARTESIAN_POINT ( 'NONE',  ( 119.2063748109119814, -1.561330072975668504, -17.79121239304076951 ) ) ;
#15363 = MECHANICAL_DESIGN_GEOMETRIC_PRESENTATION_REPRESENTATION (  '', ( #5162 ), #5189 ) ;
#15364 = CARTESIAN_POINT ( 'NONE',  ( 62.30685165342923426, -3.581745535644693224, -19.25472737399296719 ) ) ;
#15365 = CARTESIAN_POINT ( 'NONE',  ( 117.0279894963340865, -11.45915905890350928, -5.771967884200551069 ) ) ;
#15366 = ORIENTED_EDGE ( 'NONE', *, *, #797, .F. ) ;
#15367 = CARTESIAN_POINT ( 'NONE',  ( 122.0046199480702569, -6.365377317481695663, -18.95617363400926081 ) ) ;
#15368 = CARTESIAN_POINT ( 'NONE',  ( 109.2294433043877575, -8.944666232049794274, -16.92356842977666886 ) ) ;
#15369 = CARTESIAN_POINT ( 'NONE',  ( 122.0994348109119443, -10.15424416112533912, -14.75197769757731336 ) ) ;
#15370 = CARTESIAN_POINT ( 'NONE',  ( 111.7327233795247849, -1.325403438956436419, -9.854619843455211026 ) ) ;
#15371 = CARTESIAN_POINT ( 'NONE',  ( 105.8292077545248446, -7.250697342233347165, -7.631215200338321125 ) ) ;
#15372 = CARTESIAN_POINT ( 'NONE',  ( 113.6471614775786492, -4.153390946401321671, -8.397313243818183892 ) ) ;
#15373 = DIRECTION ( 'NONE',  ( -0.1352586133457950590, -0.9908103287288504424, 0.000000000000000000 ) ) ;
#15374 = CARTESIAN_POINT ( 'NONE',  ( 126.1837548109119211, -10.63000616557722466, -14.87417383870573495 ) ) ;
#15375 = CARTESIAN_POINT ( 'NONE',  ( 119.9438214775786378, -7.893985811506177619, -18.51759400769804742 ) ) ;
#15377 = VERTEX_POINT ( 'NONE', #4158 ) ;
#15376 = EDGE_CURVE ( 'NONE', #2865, #35384, #21271, .T. ) ;
#15378 = CARTESIAN_POINT ( 'NONE',  ( 117.9016614775786280, -0.1624402480850797581, -16.17319339645315424 ) ) ;
#15379 = CARTESIAN_POINT ( 'NONE',  ( 116.3133148109119759, -7.893985811506177619, -18.51759400769804742 ) ) ;
#15380 = AXIS2_PLACEMENT_3D ( 'NONE', #40089, #8850, #8406 ) ;
#15381 = CARTESIAN_POINT ( 'NONE',  ( 122.8368814775786291, -1.561330072975668948, -17.79121239304076951 ) ) ;
#15382 = CARTESIAN_POINT ( 'NONE',  ( 119.2631014775786298, -9.565557343593413364, -10.61323700422348004 ) ) ;
#15383 = ORIENTED_EDGE ( 'NONE', *, *, #43156, .T. ) ;
#15384 = CARTESIAN_POINT ( 'NONE',  ( 123.6877814775786533, -6.222761293078241884, -8.102969835052219238 ) ) ;
#15385 =( BOUNDED_CURVE ( )  B_SPLINE_CURVE ( 3, ( #11193, #14380, #4101, #25770 ),
 .UNSPECIFIED., .F., .F. ) 
 B_SPLINE_CURVE_WITH_KNOTS ( ( 4, 4 ),
 ( 1.159686988438800137, 1.570796326794895004 ),
 .UNSPECIFIED. ) 
 CURVE ( )  GEOMETRIC_REPRESENTATION_ITEM ( )  RATIONAL_B_SPLINE_CURVE ( ( 1.000000000000000000, 0.9859652809920760319, 0.9859652809920760319, 1.000000000000000000 ) ) 
 REPRESENTATION_ITEM ( '' )  );
#15386 = AXIS2_PLACEMENT_3D ( 'NONE', #28838, #12180, #8751 ) ;
#15387 = CARTESIAN_POINT ( 'NONE',  ( 120.7379948109119709, -10.63000616557722466, -14.87417383870573495 ) ) ;
#15388 = CARTESIAN_POINT ( 'NONE',  ( 125.0660727672596408, -6.058182552637899398, -5.977212348642386708 ) ) ;
#15389 = CARTESIAN_POINT ( 'NONE',  ( 121.6456214775786293, -10.63000616557722466, -14.87417383870573495 ) ) ;
#15390 = CIRCLE ( 'NONE', #40889, 4.500000000000003553 ) ;
#15391 = CARTESIAN_POINT ( 'NONE',  ( 64.69189222814998175, -41.76310523276723785, -20.39321520033831447 ) ) ;
#15392 = CARTESIAN_POINT ( 'NONE',  ( 127.8688423620682215, -3.182392322772966242, -14.38315457524332075 ) ) ;
#15393 = CARTESIAN_POINT ( 'NONE',  ( 112.7050671295247923, 0.1403307496149613920, -13.39321520033831447 ) ) ;
#15394 = DIRECTION ( 'NONE',  ( 1.000000000000000000, 0.000000000000000000, 0.000000000000000000 ) ) ;
#15395 = CARTESIAN_POINT ( 'NONE',  ( 136.1673833308564099, -10.27421185173757934, -11.10761155373447373 ) ) ;
#15396 = CARTESIAN_POINT ( 'NONE',  ( 114.2711548109119803, -0.1624402480850797581, -16.17319339645315424 ) ) ;
#15397 = CARTESIAN_POINT ( 'NONE',  ( 112.0588148109119828, -9.859900752359374465, -12.68260735090039404 ) ) ;
#15398 = DIRECTION ( 'NONE',  ( -0.000000000000000000, -0.9284778069183720062, -0.3713878862591650232 ) ) ;
#15399 = CARTESIAN_POINT ( 'NONE',  ( 116.9417077545247992, -2.791137627527939813, -18.39754474579286025 ) ) ;
#15400 = CARTESIAN_POINT ( 'NONE',  ( 109.6491296295247793, -4.863998795839590272, -8.388885654883775800 ) ) ;
#15401 = CARTESIAN_POINT ( 'NONE',  ( 114.9518748109119883, -7.643976991954077427, -18.09477374809248928 ) ) ;
#15402 = CARTESIAN_POINT ( 'NONE',  ( 75.95778847736481509, -3.256761025687722189, -7.993215200338315007 ) ) ;
#15403 = AXIS2_PLACEMENT_3D ( 'NONE', #5042, #32183, #4594 ) ;
#15404 = CARTESIAN_POINT ( 'NONE',  ( 123.9836468052895526, -1.125321370491285444, -17.12283323191017814 ) ) ;
#15406 = CARTESIAN_POINT ( 'NONE',  ( 120.2274548109119934, 0.5811942927096110934, -14.16772938898807510 ) ) ;
#15405 = CARTESIAN_POINT ( 'NONE',  ( 60.06931813437628875, -14.72076136720885309, -8.603412892520120536 ) ) ;
#15407 = CARTESIAN_POINT ( 'NONE',  ( 121.5888948109119809, 0.1319031606808879209, -14.10382304977623669 ) ) ;
#15408 = ORIENTED_EDGE ( 'NONE', *, *, #18053, .F. ) ;
#15409 = CARTESIAN_POINT ( 'NONE',  ( 137.1399781294005891, -8.821015187752031750, -9.781153249680350825 ) ) ;
#15410 = CARTESIAN_POINT ( 'NONE',  ( 66.16856755279033564, -15.11643429149317619, -10.39321520033831270 ) ) ;
#15411 = CARTESIAN_POINT ( 'NONE',  ( 110.5520202545248054, 0.1403307496149616695, -11.32035403202665336 ) ) ;
#15412 = CARTESIAN_POINT ( 'NONE',  ( 119.6601881442453106, -1.833838273342659253, -17.42832698103878286 ) ) ;
#15413 = CARTESIAN_POINT ( 'NONE',  ( 121.0216281442452981, -7.894159318335828068, -9.358103419637847864 ) ) ;
#15414 = CARTESIAN_POINT ( 'NONE',  ( 115.0086014775786509, -5.574606645277164318, -18.38911715685844683 ) ) ;
#15415 = CARTESIAN_POINT ( 'NONE',  ( 120.6611768734311028, -1.223627541775709426, -16.99192386690442547 ) ) ;
#15416 = CARTESIAN_POINT ( 'NONE',  ( 108.9545983795247821, -0.7896495226426338832, -9.318865927141430916 ) ) ;
#15417 = CARTESIAN_POINT ( 'NONE',  ( 124.6521348109119884, -7.894159318335828068, -9.358103419637847864 ) ) ;
#15418 = CARTESIAN_POINT ( 'NONE',  ( 122.2696148109119889, -5.574606645277164318, -18.38911715685844683 ) ) ;
#15419 = DIRECTION ( 'NONE',  ( -1.387778780781445478E-15, -1.000000000000000000, 0.000000000000000000 ) ) ;
#15420 = CARTESIAN_POINT ( 'NONE',  ( 112.6260814775786514, -0.8288870151387699448, -10.36305467784174006 ) ) ;
#15421 = CARTESIAN_POINT ( 'NONE',  ( 120.0212673109119805, -9.289237151508434209, -11.05642687123711276 ) ) ;
#15422 = CARTESIAN_POINT ( 'NONE',  ( 106.2459265045248173, -2.791137627527939813, -8.388885654883777576 ) ) ;
#15423 = CARTESIAN_POINT ( 'NONE',  ( 70.19189222814998175, -57.62004466406306591, -36.25082616574646721 ) ) ;
#15424 = CARTESIAN_POINT ( 'NONE',  ( 83.02743615869442806, -30.94908174223593633, -21.89321520033831447 ) ) ;
#15425 = CARTESIAN_POINT ( 'NONE',  ( 121.8725281442453223, -3.383040157471821630, -19.15922257007629170 ) ) ;
#15426 = CARTESIAN_POINT ( 'NONE',  ( 117.3343948109119737, -3.383040157471821630, -19.15922257007629170 ) ) ;
#15427 = CARTESIAN_POINT ( 'NONE',  ( 107.3571765045248299, -7.250697342233347165, -19.15521520033831138 ) ) ;
#15428 = CARTESIAN_POINT ( 'NONE',  ( 116.5969481442453031, 0.5811942927096154232, -14.16772938898807155 ) ) ;
#15429 = CARTESIAN_POINT ( 'NONE',  ( 46.47434218039879283, -17.93412427487546523, -19.39321520033831447 ) ) ;
#15430 = ORIENTED_EDGE ( 'NONE', *, *, #44279, .T. ) ;
#15431 = CARTESIAN_POINT ( 'NONE',  ( 79.79010115959992788, 5.106172230548759572, -4.893215200338314474 ) ) ;
#15432 = CARTESIAN_POINT ( 'NONE',  ( 118.4122014775786340, 0.5811942927096110934, -14.16772938898807510 ) ) ;
#15433 = CARTESIAN_POINT ( 'NONE',  ( 112.1722681442453222, -0.4660016031367893996, -10.09054647747474043 ) ) ;
#15434 = DIRECTION ( 'NONE',  ( 0.000000000000000000, 0.000000000000000000, 1.000000000000000000 ) ) ;
#15435 = CARTESIAN_POINT ( 'NONE',  ( 113.3635281442453504, -0.1624402480850797581, -16.17319339645315424 ) ) ;
#15436 = CARTESIAN_POINT ( 'NONE',  ( 125.5597614775786326, -1.561330072975669392, -17.79121239304076951 ) ) ;
#15437 = CARTESIAN_POINT ( 'NONE',  ( 110.5520202545248054, -10.62599879583958717, -15.77991374673208469 ) ) ;
#15438 = AXIS2_PLACEMENT_3D ( 'NONE', #27391, #6639, #20770 ) ;
#15439 = EDGE_CURVE ( 'NONE', #34542, #19992, #21982, .T. ) ;
#15440 = CARTESIAN_POINT ( 'NONE',  ( 120.0572748109119772, -6.222761293078241884, -8.102969835052219238 ) ) ;
#15441 = CARTESIAN_POINT ( 'NONE',  ( 110.2742077545248236, -7.250697342233347165, -7.631215200338321125 ) ) ;
#15442 = DIRECTION ( 'NONE',  ( 1.000000000000000000, 0.000000000000000000, -0.000000000000000000 ) ) ;
#15443 = VERTEX_POINT ( 'NONE', #35153 ) ;
#15444 = CARTESIAN_POINT ( 'NONE',  ( 119.6740016859119748, -0.6942167230862511529, -9.935906262978006609 ) ) ;
#15445 = CARTESIAN_POINT ( 'NONE',  ( 123.4608748109119745, -10.63000616557722466, -14.87417383870573495 ) ) ;
#15446 = ORIENTED_EDGE ( 'NONE', *, *, #35105, .F. ) ;
#15447 = CARTESIAN_POINT ( 'NONE',  ( 82.92338557575642710, -31.41857578345838675, -21.89321520033831447 ) ) ;
#15448 = AXIS2_PLACEMENT_3D ( 'NONE', #30383, #20131, #2327 ) ;
#15449 = CARTESIAN_POINT ( 'NONE',  ( -12.68961124276041019, -4.256188596408917668, -7.420957702222477970 ) ) ;
#15450 = FACE_OUTER_BOUND ( 'NONE', #43134, .T. ) ;
#15451 = CARTESIAN_POINT ( 'NONE',  ( 118.6391081442452986, -5.574606645277164318, -18.38911715685844683 ) ) ;
#15452 = FACE_OUTER_BOUND ( 'NONE', #32299, .T. ) ;
#15453 = CARTESIAN_POINT ( 'NONE',  ( 124.5316694066389971, -9.821485997248675659, -12.73715838876115036 ) ) ;
#15454 = CARTESIAN_POINT ( 'NONE',  ( 121.9859814775786333, -9.565557343593413364, -10.61323700422348004 ) ) ;
#15455 = DIRECTION ( 'NONE',  ( -0.000000000000000000, -0.9284778069183721172, -0.3713878862591650232 ) ) ;
#15456 = CARTESIAN_POINT ( 'NONE',  ( 123.8579614775786126, -9.859900752359378018, -12.68260735090039759 ) ) ;
#15457 = CARTESIAN_POINT ( 'NONE',  ( 125.3535861756261482, -11.55705830787929678, -15.61165832305779944 ) ) ;
#15458 = SHAPE_REPRESENTATION ( 'Main Bracket', ( #12375 ), #21301 ) ;
#15459 = CARTESIAN_POINT ( 'NONE',  ( 117.1642148109119859, -0.8288870151387760510, -10.36305467784173118 ) ) ;
#15460 = CARTESIAN_POINT ( 'NONE',  ( 123.1205148109119563, -7.643976991954077427, -18.09477374809248928 ) ) ;
#15461 = CARTESIAN_POINT ( 'NONE',  ( 118.9227414775786400, -10.63000616557722466, -14.87417383870573495 ) ) ;
#15462 = CARTESIAN_POINT ( 'NONE',  ( 116.8805814775786445, -6.344957434206662583, -7.627207830600332805 ) ) ;
#15463 = CARTESIAN_POINT ( 'NONE',  ( 113.8163171295247764, 0.1403307496149613920, -13.39321520033831447 ) ) ;
#15464 = CARTESIAN_POINT ( 'NONE',  ( 123.4608748109119745, 0.4262465694468514643, -12.03445270309931736 ) ) ;
#15465 = EDGE_LOOP ( 'NONE', ( #26416, #10703, #730, #22192, #31656 ) ) ;
#15466 = CARTESIAN_POINT ( 'NONE',  ( 120.1140014775786398, -1.561330072975668504, -17.79121239304076951 ) ) ;
#15467 = CARTESIAN_POINT ( 'NONE',  ( 115.2053796295247849, -4.863998795839590272, -19.15521520033831493 ) ) ;
#15468 = CARTESIAN_POINT ( 'NONE',  ( 109.1629577545248395, -2.791137627527939813, -18.39754474579286025 ) ) ;
#15469 = CARTESIAN_POINT ( 'NONE',  ( 83.49267580666517574, -32.76310523276723785, -23.89321520033831803 ) ) ;
#15470 = DIRECTION ( 'NONE',  ( -0.9498278979187094739, -0.3127730236694427068, -0.000000000000000000 ) ) ;
#15471 = AXIS2_PLACEMENT_3D ( 'NONE', #37563, #34791, #24341 ) ;
#15472 = CARTESIAN_POINT ( 'NONE',  ( 137.6352241515737376, -2.583465948169414883, -17.67907559073337964 ) ) ;
#15473 = CARTESIAN_POINT ( 'NONE',  ( 125.8433948109119456, -1.834011780172310813, -8.268836392978581529 ) ) ;
#15474 = ORIENTED_EDGE ( 'NONE', *, *, #43991, .F. ) ;
#15475 = CARTESIAN_POINT ( 'NONE',  ( 124.4252281442452812, -0.8288870151387760510, -10.36305467784173118 ) ) ;
#15476 = CARTESIAN_POINT ( 'NONE',  ( 121.5492360609119800, -6.564341423271550902, -7.887810678476487425 ) ) ;
#15477 = CARTESIAN_POINT ( 'NONE',  ( 123.9800954359119771, -11.07370829466463569, -12.81314460846529002 ) ) ;
#15478 = AXIS2_PLACEMENT_3D ( 'NONE', #1515, #4934, #1739 ) ;
#15479 = FACE_OUTER_BOUND ( 'NONE', #9041, .T. ) ;
#15480 = CARTESIAN_POINT ( 'NONE',  ( 108.6767858795247861, -8.402594152722688392, -9.854619843455216355 ) ) ;
#15481 = ORIENTED_EDGE ( 'NONE', *, *, #18083, .F. ) ;
#15482 = CIRCLE ( 'NONE', #36584, 0.8509999999999994236 ) ;
#15483 = CARTESIAN_POINT ( 'NONE',  ( 116.5402214775786405, 0.2603800115204892296, -16.42320221600525088 ) ) ;
#15484 = DIRECTION ( 'NONE',  ( 0.9609149988134843001, -0.1028163501681632064, 0.2570431154366505933 ) ) ;
#15485 = CARTESIAN_POINT ( 'NONE',  ( 121.4754414775786131, -1.833838273342659697, -17.42832698103878286 ) ) ;
#15486 = CARTESIAN_POINT ( 'NONE',  ( 115.9729548109119861, -3.505236298600246325, -18.68346056562440793 ) ) ;
#15487 = CARTESIAN_POINT ( 'NONE',  ( 75.95778847736514194, -3.256761025687008537, -12.39321520033831447 ) ) ;
#15488 = CARTESIAN_POINT ( 'NONE',  ( 83.72016463086879412, -25.99489077589524300, -13.39321520033831447 ) ) ;
#15489 = CARTESIAN_POINT ( 'NONE',  ( 113.4202548109119846, -10.30919188438810075, -12.61870101168855918 ) ) ;
#15490 = CARTESIAN_POINT ( 'NONE',  ( 114.7886608795247696, -1.325403438956436419, -16.93181055722141792 ) ) ;
#15491 = CARTESIAN_POINT ( 'NONE',  ( 124.4252281442452812, -9.261995988541697145, -16.69588392320189030 ) ) ;
#15492 = CARTESIAN_POINT ( 'NONE',  ( 137.0134976903428310, -9.802792590006783158, -15.70761676718206523 ) ) ;
#15493 = VERTEX_POINT ( 'NONE', #14654 ) ;
#15494 = CARTESIAN_POINT ( 'NONE',  ( 115.0086014775786509, -4.089484607189486809, -7.948022111789456723 ) ) ;
#15495 = CARTESIAN_POINT ( 'NONE',  ( 124.4819548109119722, -7.893985811506177619, -18.51759400769804742 ) ) ;
#15496 = DIRECTION ( 'NONE',  ( 0.9609149988134837450, -0.1028163501681639419, 0.2570431154366518145 ) ) ;
#15497 = CARTESIAN_POINT ( 'NONE',  ( 125.0492214775786266, -3.505236298600246325, -18.68346056562440793 ) ) ;
#15498 = ORIENTED_EDGE ( 'NONE', *, *, #24246, .T. ) ;
#15499 = CARTESIAN_POINT ( 'NONE',  ( 118.8660148109119774, -10.30919188438810075, -12.61870101168855918 ) ) ;
#15500 = DIRECTION ( 'NONE',  ( 0.000000000000000000, 0.3713878862591642460, -0.9284778069183722282 ) ) ;
#15501 = CARTESIAN_POINT ( 'NONE',  ( 109.9269421295247753, -9.868328341294093420, -13.39321520033838553 ) ) ;
#15502 = DIRECTION ( 'NONE',  ( 0.000000000000000000, 0.000000000000000000, 1.000000000000000000 ) ) ;
#15503 = DIRECTION ( 'NONE',  ( 1.000000000000000000, 0.000000000000000000, -0.000000000000000000 ) ) ;
#15504 = CARTESIAN_POINT ( 'NONE',  ( 115.9162281442453093, -5.574606645277164318, -18.38911715685844683 ) ) ;
#15505 = CARTESIAN_POINT ( 'NONE',  ( 82.31000308962319423, -13.76004065658516673, -18.64321520033831803 ) ) ;
#15506 = AXIS2_PLACEMENT_3D ( 'NONE', #14046, #24097, #20227 ) ;
#15507 = CARTESIAN_POINT ( 'NONE',  ( 124.8714078922225497, -3.772723311433941795, -21.00617493672336167 ) ) ;
#15508 = CARTESIAN_POINT ( 'NONE',  ( 113.7038881442453402, -6.222761293078241884, -8.102969835052219238 ) ) ;
#15509 = CARTESIAN_POINT ( 'NONE',  ( 113.1366214775786432, -1.834011780172310813, -8.268836392978581529 ) ) ;
#15510 = CARTESIAN_POINT ( 'NONE',  ( 116.6078919537301033, -9.852945098058393469, -13.98784572441250162 ) ) ;
#15511 = CARTESIAN_POINT ( 'NONE',  ( 124.9924948109119924, -5.574606645277164318, -18.38911715685844683 ) ) ;
#15512 = CARTESIAN_POINT ( 'NONE',  ( 123.9584548109119737, -7.429215134363809092, -20.97079166887802160 ) ) ;
#15513 = CARTESIAN_POINT ( 'NONE',  ( 120.4543614775786295, -4.089484607189486809, -7.948022111789456723 ) ) ;
#15514 = CARTESIAN_POINT ( 'NONE',  ( 120.8514481442452961, -7.893985811506177619, -18.51759400769804742 ) ) ;
#15515 = ORIENTED_EDGE ( 'NONE', *, *, #4208, .F. ) ;
#15516 = CARTESIAN_POINT ( 'NONE',  ( 117.8659193777725278, -1.267766418764730840, -16.93314635290706605 ) ) ;
#15517 = LINE ( 'NONE', #11437, #5994 ) ;
#15518 = CARTESIAN_POINT ( 'NONE',  ( 110.2047546295247855, -4.863998795839590272, -18.39754474579285315 ) ) ;
#15519 = CARTESIAN_POINT ( 'NONE',  ( 107.8433483795247838, -8.402594152722688392, -16.93181055722141792 ) ) ;
#15520 = CARTESIAN_POINT ( 'NONE',  ( 125.7299414775786488, -10.15424416112507799, -14.75197769757834543 ) ) ;
#15521 = CARTESIAN_POINT ( 'NONE',  ( 113.4769814775786330, -10.63000616557722466, -14.87417383870573495 ) ) ;
#15522 = EDGE_LOOP ( 'NONE', ( #11950, #5287, #32824, #36722 ) ) ;
#15523 = CARTESIAN_POINT ( 'NONE',  ( 106.9404577545248145, -7.250697342233347165, -7.631215200338321125 ) ) ;
#15524 = DIRECTION ( 'NONE',  ( 0.9609149988134837450, -0.1028163501681639419, 0.2570431154366518145 ) ) ;
#15525 = DIRECTION ( 'NONE',  ( -1.000000000000000000, 0.000000000000000000, 0.000000000000000000 ) ) ;
#15526 = EDGE_CURVE ( 'NONE', #10099, #41818, #27810, .T. ) ;
#15527 = CARTESIAN_POINT ( 'NONE',  ( 112.7962614775786676, -3.383040157471821630, -19.15922257007629170 ) ) ;
#15528 = CARTESIAN_POINT ( 'NONE',  ( 121.4187148109119789, -6.344957434206665248, -7.627207830600338134 ) ) ;
#15529 = AXIS2_PLACEMENT_3D ( 'NONE', #10013, #30519, #30970 ) ;
#15530 = CARTESIAN_POINT ( 'NONE',  ( 111.5938171295247940, -10.62599879583958540, -13.39321520033831447 ) ) ;
#15531 = CARTESIAN_POINT ( 'NONE',  ( 71.31713442278437753, 2.423123680056944007, -19.39321520033831447 ) ) ;
#15532 = ORIENTED_EDGE ( 'NONE', *, *, #10152, .T. ) ;
#15533 = CARTESIAN_POINT ( 'NONE',  ( 121.4070848136183400, -3.929494816604741203, -18.62311481910882804 ) ) ;
#15534 = CARTESIAN_POINT ( 'NONE',  ( 120.0572748109119772, -6.222761293078241884, -8.102969835052219238 ) ) ;
#15535 = VECTOR ( 'NONE', #30961, 1000.000000000000000 ) ;
#15536 = CARTESIAN_POINT ( 'NONE',  ( 117.8449348109119938, -8.166667518702817929, -8.995218007635861213 ) ) ;
#15537 = CARTESIAN_POINT ( 'NONE',  ( 112.5126281442453120, -10.30919188438810075, -12.61870101168855918 ) ) ;
#15538 = CARTESIAN_POINT ( 'NONE',  ( 118.0106993026122950, -1.179503403430468333, -17.05068175419387089 ) ) ;
#15539 = CARTESIAN_POINT ( 'NONE',  ( 122.3263414775786373, -3.505236298600246325, -18.68346056562440793 ) ) ;
#15540 = CARTESIAN_POINT ( 'NONE',  ( 115.5758681442453053, -7.894159318335828068, -9.358103419637847864 ) ) ;
#15541 = ORIENTED_EDGE ( 'NONE', *, *, #35321, .T. ) ;
#15542 = CARTESIAN_POINT ( 'NONE',  ( 124.0495485609119584, -0.08252387247370887580, -11.91645802438286417 ) ) ;
#15543 = AXIS2_PLACEMENT_3D ( 'NONE', #33467, #13873, #28234 ) ;
#15544 = CARTESIAN_POINT ( 'NONE',  ( 113.3109957829843779, 0.6362173239733635022, -14.64321520033831447 ) ) ;
#15545 = CARTESIAN_POINT ( 'NONE',  ( 117.6180281442453150, -8.899110576539710493, -16.42337572283490132 ) ) ;
#15546 = ORIENTED_EDGE ( 'NONE', *, *, #31868, .T. ) ;
#15547 = CARTESIAN_POINT ( 'NONE',  ( 110.5266510812576826, -0.01829820670803256055, -12.14321520033831625 ) ) ;
#15548 = CARTESIAN_POINT ( 'NONE',  ( 114.7249681442453237, 0.2603800115204892296, -16.42320221600525088 ) ) ;
#15549 = CARTESIAN_POINT ( 'NONE',  ( 115.5526452545247622, 0.8980012041604421569, -11.00651665394454071 ) ) ;
#15550 = CARTESIAN_POINT ( 'NONE',  ( 113.1933481442453058, -5.574606645277164318, -18.38911715685844683 ) ) ;
#15551 = ADVANCED_FACE ( 'NONE', ( #33874 ), #32542, .T. ) ;
#15552 = ORIENTED_EDGE ( 'NONE', *, *, #17958, .T. ) ;
#15553 = ORIENTED_EDGE ( 'NONE', *, *, #29229, .T. ) ;
#15554 = CARTESIAN_POINT ( 'NONE',  ( 122.7801548109119665, -6.222761293078241884, -8.102969835052219238 ) ) ;
#15555 = CARTESIAN_POINT ( 'NONE',  ( 116.8238548109119819, -5.574606645277164318, -18.38911715685844683 ) ) ;
#15556 = EDGE_CURVE ( 'NONE', #30023, #29206, #31602, .T. ) ;
#15557 = ORIENTED_EDGE ( 'NONE', *, *, #16397, .F. ) ;
#15558 = AXIS2_PLACEMENT_3D ( 'NONE', #7503, #22045, #35938 ) ;
#15559 = CARTESIAN_POINT ( 'NONE',  ( 86.34560043013698305, -9.320000780048239619, -18.64321520033831803 ) ) ;
#15560 = CARTESIAN_POINT ( 'NONE',  ( 61.69189222814998175, -66.36873802749349238, -42.40236911872441539 ) ) ;
#15561 = EDGE_CURVE ( 'NONE', #22394, #7248, #13308, .T. ) ;
#15562 = CARTESIAN_POINT ( 'NONE',  ( 107.3571765045248299, -7.250697342233347165, -19.15521520033831138 ) ) ;
#15563 = VECTOR ( 'NONE', #8925, 1000.000000000000000 ) ;
#15564 = CARTESIAN_POINT ( 'NONE',  ( 118.0718414775786300, -9.261995988541697145, -16.69588392320189030 ) ) ;
#15566 = CARTESIAN_POINT ( 'NONE',  ( 116.3700414775786527, -4.153390946401321671, -8.397313243818183892 ) ) ;
#15565 = CARTESIAN_POINT ( 'NONE',  ( 113.8173414775786512, 0.2603800115204892296, -16.42320221600525088 ) ) ;
#15567 = CARTESIAN_POINT ( 'NONE',  ( 122.7801548109119665, -6.222761293078241884, -8.102969835052219238 ) ) ;
#15568 = DIRECTION ( 'NONE',  ( -0.000000000000000000, -0.9284778069183720062, -0.3713878862591650232 ) ) ;
#15569 = ORIENTED_EDGE ( 'NONE', *, *, #37000, .T. ) ;
#15570 = CARTESIAN_POINT ( 'NONE',  ( 119.4900081442453086, -7.643976991954077427, -18.09477374809248928 ) ) ;
#15571 = ADVANCED_FACE ( 'NONE', ( #24991 ), #28201, .F. ) ;
#15572 = CARTESIAN_POINT ( 'NONE',  ( 124.5386814775786206, -4.153390946401325223, -8.397313243818185668 ) ) ;
#15573 = CARTESIAN_POINT ( 'NONE',  ( 112.9134265045247645, -7.250697342233347165, -19.15521520033831138 ) ) ;
#15574 = CIRCLE ( 'NONE', #33026, 2.445500000000004448 ) ;
#15575 = CARTESIAN_POINT ( 'NONE',  ( 114.1175919737025737, -1.196538596002799215, -17.02799684832027083 ) ) ;
#15576 = CARTESIAN_POINT ( 'NONE',  ( 111.8716296295247901, -4.863998795839590272, -19.15521520033831493 ) ) ;
#15577 = CARTESIAN_POINT ( 'NONE',  ( 118.5823814775786360, -1.834011780172310813, -8.268836392978581529 ) ) ;
#15578 = ORIENTED_EDGE ( 'NONE', *, *, #21874, .T. ) ;
#15579 = EDGE_CURVE ( 'NONE', #21542, #3446, #44619, .T. ) ;
#15580 = CARTESIAN_POINT ( 'NONE',  ( 119.2631014775786298, 0.2603800115204892296, -16.42320221600525088 ) ) ;
#15581 = DIRECTION ( 'NONE',  ( 0.000000000000000000, 0.000000000000000000, -1.000000000000000000 ) ) ;
#15582 = CARTESIAN_POINT ( 'NONE',  ( 106.1764733795248219, -8.938348069036489818, -17.46756447353520159 ) ) ;
#15583 = CARTESIAN_POINT ( 'NONE',  ( 114.7249681442453237, 0.2603800115204892296, -16.42320221600525088 ) ) ;
#15584 = ADVANCED_FACE ( 'NONE', ( #41883 ), #24764, .T. ) ;
#15585 = ADVANCED_FACE ( 'NONE', ( #26517 ), #2328, .T. ) ;
#15586 = CARTESIAN_POINT ( 'NONE',  ( 119.3765548109119834, 0.9020085738987339008, -11.91225656197089222 ) ) ;
#15587 = LINE ( 'NONE', #29489, #7549 ) ;
#15588 = CARTESIAN_POINT ( 'NONE',  ( 116.6905827088848753, -11.81713141088397379, -6.316351274785676040 ) ) ;
#15589 = ORIENTED_EDGE ( 'NONE', *, *, #3676, .F. ) ;
#15590 = DIRECTION ( 'NONE',  ( 0.000000000000000000, 0.000000000000000000, -1.000000000000000000 ) ) ;
#15591 = CARTESIAN_POINT ( 'NONE',  ( 109.2295563141408650, -10.31498796290959774, -11.96776437853030828 ) ) ;
#15592 = CARTESIAN_POINT ( 'NONE',  ( 119.6601881442453106, -1.833838273342659253, -17.42832698103878286 ) ) ;
#15593 = CARTESIAN_POINT ( 'NONE',  ( 113.8163171295247764, 0.1403307496149613920, -13.39321520033831447 ) ) ;
#15594 = CARTESIAN_POINT ( 'NONE',  ( 115.7610046295247912, -4.863998795839590272, -18.39754474579285315 ) ) ;
#15595 = CARTESIAN_POINT ( 'NONE',  ( 112.7962614775786676, -6.222761293078241884, -8.102969835052219238 ) ) ;
#15596 = DIRECTION ( 'NONE',  ( 0.000000000000000000, -0.9242245927363028635, -0.3818493186865930533 ) ) ;
#15597 = CARTESIAN_POINT ( 'NONE',  ( 71.38975968946110129, -26.28004934490193989, -5.218938316979315317 ) ) ;
#15598 = CARTESIAN_POINT ( 'NONE',  ( 113.5337081442453240, -0.8288870151387760510, -10.36305467784173118 ) ) ;
#15599 = CARTESIAN_POINT ( 'NONE',  ( 118.8092881442453290, -9.988377603198976828, -10.36322818467138340 ) ) ;
#15600 = ORIENTED_EDGE ( 'NONE', *, *, #11107, .T. ) ;
#15601 = CARTESIAN_POINT ( 'NONE',  ( 118.9794681442453026, -0.8288870151387760510, -10.36305467784173118 ) ) ;
#15602 = CARTESIAN_POINT ( 'NONE',  ( 116.0296814775786345, -8.166667518702817929, -8.995218007635861213 ) ) ;
#15603 = CARTESIAN_POINT ( 'NONE',  ( 123.1772414775786189, -4.089484607189486809, -7.948022111789456723 ) ) ;
#15604 = CARTESIAN_POINT ( 'NONE',  ( 120.0572748109119772, -6.222761293078241884, -8.102969835052219238 ) ) ;
#15605 = VERTEX_POINT ( 'NONE', #37200 ) ;
#15606 = CARTESIAN_POINT ( 'NONE',  ( 125.6732148109119862, -9.859900752359378018, -12.68260735090039759 ) ) ;
#15607 = CARTESIAN_POINT ( 'NONE',  ( 120.0005481442453146, -5.638512984488999180, -18.83840828888717311 ) ) ;
#15608 = CARTESIAN_POINT ( 'NONE',  ( 124.7472578386067283, -5.916068793159596773, -5.684620300579358521 ) ) ;
#15609 = CARTESIAN_POINT ( 'NONE',  ( 122.4965214775786251, -10.30919188438810075, -12.61870101168855918 ) ) ;
#15610 = CARTESIAN_POINT ( 'NONE',  ( 107.9822546295247889, -4.863998795839590272, -7.631215200338315796 ) ) ;
#15611 = CARTESIAN_POINT ( 'NONE',  ( 67.69189222814998175, -59.27884951796254853, -42.87418841894956500 ) ) ;
#15612 = CYLINDRICAL_SURFACE ( 'NONE', #16454, 5.000000000000004441 ) ;
#15613 = CIRCLE ( 'NONE', #28025, 5.000000000000000000 ) ;
#15614 = CARTESIAN_POINT ( 'NONE',  ( 115.4831921295247952, -9.868328341294093420, -13.39321520033831447 ) ) ;
#15615 = B_SPLINE_CURVE_WITH_KNOTS ( 'NONE', 3,
 ( #6991, #40993, #23657, #3343, #6773, #37543, #20683, #17262, #20234, #10639 ),
 .UNSPECIFIED., .F., .F.,
 ( 4, 3, 3, 4 ),
 ( 0.000000000000000000, 0.0001671877548681325037, 0.0003343755096277755095, 0.0006463528481650619413 ),
 .UNSPECIFIED. ) ;
#15616 = DIRECTION ( 'NONE',  ( 0.9609149988134837450, -0.1028163501681639419, 0.2570431154366518145 ) ) ;
#15617 = CARTESIAN_POINT ( 'NONE',  ( 136.9012041053371149, -10.04030426489261707, -11.44593779250850574 ) ) ;
#15618 = CARTESIAN_POINT ( 'NONE',  ( 119.6601881442453106, -1.833838273342659253, -17.42832698103878286 ) ) ;
#15619 = CARTESIAN_POINT ( 'NONE',  ( 124.3117748109119844, -10.30919188438810075, -12.61870101168855918 ) ) ;
#15620 = CARTESIAN_POINT ( 'NONE',  ( 64.75357039381266588, -13.20363101263777850, -15.30938453869310578 ) ) ;
#15621 = ADVANCED_BREP_SHAPE_REPRESENTATION ( '', ( #36189, #12375 ), #43820 ) ;
#15622 = EDGE_LOOP ( 'NONE', ( #29875, #41776, #35573, #35091, #3599, #18469 ) ) ;
#15623 = CARTESIAN_POINT ( 'NONE',  ( 66.58723489636778936, -20.14619392353143112, -15.89321520033831447 ) ) ;
#15624 = CARTESIAN_POINT ( 'NONE',  ( 112.0105358795247810, -8.402594152722688392, -9.854619843455216355 ) ) ;
#15625 = CARTESIAN_POINT ( 'NONE',  ( 114.5547881442453217, -4.153390946401321671, -8.397313243818183892 ) ) ;
#15626 = VECTOR ( 'NONE', #17526, 1000.000000000000114 ) ;
#15627 = CARTESIAN_POINT ( 'NONE',  ( 113.3250873908105945, -2.443475742715324639, -17.86549347949428679 ) ) ;
#15628 = ADVANCED_FACE ( 'NONE', ( #5305 ), #34018, .F. ) ;
#15629 = CARTESIAN_POINT ( 'NONE',  ( 71.04661719609278236, 0.4415030225992447321, -14.39321520033831625 ) ) ;
#15630 = CARTESIAN_POINT ( 'NONE',  ( -2.172448456896171720, -6.936427131018752412, -19.06457999368345924 ) ) ;
#15632 = CARTESIAN_POINT ( 'NONE',  ( 124.4252281442452812, -9.261995988541697145, -16.69588392320189030 ) ) ;
#15631 = CARTESIAN_POINT ( 'NONE',  ( 60.51500512425220535, -14.57399912981923684, -8.628611073238383611 ) ) ;
#15633 = CARTESIAN_POINT ( 'NONE',  ( 121.3052614775786111, -7.643976991954077427, -18.09477374809248928 ) ) ;
#15634 = ORIENTED_EDGE ( 'NONE', *, *, #42304, .T. ) ;
#15635 = CARTESIAN_POINT ( 'NONE',  ( 89.29245855188943892, -9.882163754870950001, -13.24321520033830879 ) ) ;
#15636 = DIRECTION ( 'NONE',  ( 0.000000000000000000, 0.000000000000000000, -1.000000000000000000 ) ) ;
#15637 = CARTESIAN_POINT ( 'NONE',  ( 110.3436608795247764, -1.325403438956436419, -16.93181055722141792 ) ) ;
#15638 = CARTESIAN_POINT ( 'NONE',  ( 124.4252281442452812, -0.8288870151387760510, -10.36305467784173118 ) ) ;
#15639 = CARTESIAN_POINT ( 'NONE',  ( 122.3263414775786373, -3.505236298600246325, -18.68346056562440793 ) ) ;
#15640 = CARTESIAN_POINT ( 'NONE',  ( 119.2063748109119814, -7.894159318335828068, -9.358103419637847864 ) ) ;
#15641 = CARTESIAN_POINT ( 'NONE',  ( 124.3692356341941974, 2.697552217974573896, -15.83745505781797647 ) ) ;
#15642 = CARTESIAN_POINT ( 'NONE',  ( 110.3436608795247764, -8.938348069036489818, -9.318865927141430916 ) ) ;
#15643 = DIRECTION ( 'NONE',  ( 0.000000000000000000, 0.000000000000000000, 1.000000000000000000 ) ) ;
#15644 = CARTESIAN_POINT ( 'NONE',  ( 120.3439060953690642, -6.001247023715329476, -18.26661038929047720 ) ) ;
#15645 = CARTESIAN_POINT ( 'NONE',  ( 122.6009548109119720, 0.04957186715663641774, -7.079989135975798931 ) ) ;
#15646 = CARTESIAN_POINT ( 'NONE',  ( 109.8574890045247940, 0.8980012041604421569, -15.77991374673208469 ) ) ;
#15647 = FACE_OUTER_BOUND ( 'NONE', #15108, .T. ) ;
#15648 = CARTESIAN_POINT ( 'NONE',  ( 83.90357420486833462, -31.65026256602387633, -22.30771876464736891 ) ) ;
#15649 = CARTESIAN_POINT ( 'NONE',  ( 121.0216281442452981, -1.561330072975668948, -17.79121239304076951 ) ) ;
#15650 = CARTESIAN_POINT ( 'NONE',  ( 118.3554748109119998, 0.2603800115204892296, -16.42320221600525088 ) ) ;
#15651 = CARTESIAN_POINT ( 'NONE',  ( 108.6767858795247861, -0.7896495226426338832, -17.46756447353520159 ) ) ;
#15652 = EDGE_CURVE ( 'NONE', #44020, #17452, #34395, .T. ) ;
#15653 = PRODUCT_DEFINITION ( 'UNKNOWN', '', #917, #42913 ) ;
#15654 =( BOUNDED_CURVE ( )  B_SPLINE_CURVE ( 2, ( #14776, #18428, #32320, #31870, #7039, #635, #411, #28691, #34823, #3606, #14548, #17522, #31419, #7251, #21166, #28466, #35042 ),
 .UNSPECIFIED., .F., .T. ) 
 B_SPLINE_CURVE_WITH_KNOTS ( ( 3, 2, 2, 2, 2, 2, 2, 2, 3 ),
 ( 0.7045046674808920217, 0.7109375000000000000, 0.7187500000000000000, 0.7265625000000000000, 0.7343750000000000000, 0.7421875000000000000, 0.7500000000000000000, 0.7578125000000000000, 0.7642453325190590174 ),
 .UNSPECIFIED. ) 
 CURVE ( )  GEOMETRIC_REPRESENTATION_ITEM ( )  RATIONAL_B_SPLINE_CURVE ( ( 0.9778625265006459788, 0.9373222120152210346, 1.000000000000000000, 0.9238795325112869605, 1.000000000000000000, 0.9238795325112869605, 1.000000000000000000, 0.9238795325112869605, 1.000000000000000000, 0.9238795325112869605, 1.000000000000000000, 0.9238795325112869605, 1.000000000000000000, 0.9238795325112869605, 1.000000000000000000, 0.9373222120157009840, 0.9778625265000250311 ) ) 
 REPRESENTATION_ITEM ( '' )  );
#15655 = CARTESIAN_POINT ( 'NONE',  ( 117.7882081442453170, -6.344957434206665248, -7.627207830600338134 ) ) ;
#15656 = CARTESIAN_POINT ( 'NONE',  ( 111.4705635773848940, -2.467220198592768199, -17.83387418641523325 ) ) ;
#15657 = VERTEX_POINT ( 'NONE', #9636 ) ;
#15658 = DIRECTION ( 'NONE',  ( 0.000000000000000000, 0.000000000000000000, -1.000000000000000000 ) ) ;
#15659 = VECTOR ( 'NONE', #31257, 1000.000000000000000 ) ;
#15660 = CARTESIAN_POINT ( 'NONE',  ( 121.0783548109119749, 0.2603800115204892296, -16.42320221600525088 ) ) ;
#15661 = CARTESIAN_POINT ( 'NONE',  ( 121.0783548109119749, 0.2603800115204892296, -16.42320221600525088 ) ) ;
#15662 = CARTESIAN_POINT ( 'NONE',  ( 126.4673881442452910, -7.894159318335828068, -9.358103419637847864 ) ) ;
#15663 = CARTESIAN_POINT ( 'NONE',  ( 114.1009748109119784, -5.574606645277164318, -18.38911715685844683 ) ) ;
#15664 = CARTESIAN_POINT ( 'NONE',  ( 111.4915481442453142, -1.833838273342658365, -17.42832698103878286 ) ) ;
#15665 = CIRCLE ( 'NONE', #19311, 4.999999999999998224 ) ;
#15666 = CARTESIAN_POINT ( 'NONE',  ( 111.1770983795247787, -0.7896495226426338832, -9.318865927141430916 ) ) ;
#15667 = CARTESIAN_POINT ( 'NONE',  ( 120.7947214775786193, -0.8288870151387760510, -10.36305467784173118 ) ) ;
#15668 = CARTESIAN_POINT ( 'NONE',  ( 116.7770425732746986, -3.808795826660715367, -18.46995572362991567 ) ) ;
#15669 = CARTESIAN_POINT ( 'NONE',  ( 124.1773369107181821, -2.467220198592779301, -17.83387418641524391 ) ) ;
#15670 = ORIENTED_EDGE ( 'NONE', *, *, #10288, .F. ) ;
#15671 = DIRECTION ( 'NONE',  ( 1.000000000000000000, 0.000000000000000000, 0.000000000000000000 ) ) ;
#15672 = CARTESIAN_POINT ( 'NONE',  ( 121.9859814775786333, 0.2603800115204892296, -16.42320221600525088 ) ) ;
#15673 = CARTESIAN_POINT ( 'NONE',  ( 70.19189222814998175, -66.20485342690169261, -45.06987807991856698 ) ) ;
#15674 = CARTESIAN_POINT ( 'NONE',  ( 62.63422871652684876, -3.456519832263517333, -7.588643140964075329 ) ) ;
#15675 =( LENGTH_UNIT ( ) NAMED_UNIT ( * ) SI_UNIT ( .MILLI., .METRE. ) );
#15676 = CARTESIAN_POINT ( 'NONE',  ( 118.9227414775786542, 0.4262465694468514643, -12.03445270309931736 ) ) ;
#15677 = DIRECTION ( 'NONE',  ( 0.000000000000000000, 1.000000000000000000, 0.000000000000000000 ) ) ;
#15678 = CARTESIAN_POINT ( 'NONE',  ( 64.24559192882155401, -35.37386509779257437, -5.871741255084225841 ) ) ;
#15679 = CARTESIAN_POINT ( 'NONE',  ( 125.2761281442453054, 0.4262465694468514643, -12.03445270309931736 ) ) ;
#15680 = ADVANCED_FACE ( 'NONE', ( #2787 ), #40194, .T. ) ;
#15681 = CARTESIAN_POINT ( 'NONE',  ( 121.2019704359119885, 1.345710702986149920, -13.97328579221134071 ) ) ;
#15682 = CARTESIAN_POINT ( 'NONE',  ( 125.5030348109119558, -6.222761293078241884, -8.102969835052219238 ) ) ;
#15683 = AXIS2_PLACEMENT_3D ( 'NONE', #22292, #18649, #8611 ) ;
#15684 = CARTESIAN_POINT ( 'NONE',  ( 125.2723929556167661, -11.93466551383809815, -14.87328830137684221 ) ) ;
#15685 = CARTESIAN_POINT ( 'NONE',  ( 122.1561614775786353, -0.4660016031367893996, -10.09054647747474043 ) ) ;
#15686 = CARTESIAN_POINT ( 'NONE',  ( 117.2776681442452968, -4.153390946401325223, -8.397313243818185668 ) ) ;
#15687 = CARTESIAN_POINT ( 'NONE',  ( 121.8725281442453223, -6.222761293078241884, -8.102969835052219238 ) ) ;
#15688 = EDGE_LOOP ( 'NONE', ( #13904, #17743, #16501, #19880, #40440, #22359 ) ) ;
#15689 = CARTESIAN_POINT ( 'NONE',  ( 124.3685014775786328, -10.63000616557722466, -14.87417383870573495 ) ) ;
#15690 = CARTESIAN_POINT ( 'NONE',  ( 116.3700414775786527, -5.638512984488999180, -18.83840828888717311 ) ) ;
#15691 = CARTESIAN_POINT ( 'NONE',  ( 112.9828796295247884, -4.863998795839590272, -8.388885654883775800 ) ) ;
#15692 = CARTESIAN_POINT ( 'NONE',  ( 113.8740681442453138, -9.859900752359374465, -12.68260735090039404 ) ) ;
#15693 = CARTESIAN_POINT ( 'NONE',  ( 122.6099748109119929, -0.8288870151387760510, -10.36305467784173118 ) ) ;
#15694 = CARTESIAN_POINT ( 'NONE',  ( 120.6245414775786458, -9.988377603198976828, -10.36322818467138340 ) ) ;
#15695 = CARTESIAN_POINT ( 'NONE',  ( 115.5526452545247622, 0.8980012041604421569, -11.00651665394454071 ) ) ;
#15696 = CARTESIAN_POINT ( 'NONE',  ( 107.9822546295247889, -4.863998795839590272, -18.39754474579285315 ) ) ;
#15697 = DIRECTION ( 'NONE',  ( 0.000000000000000000, 0.000000000000000000, 1.000000000000000000 ) ) ;
#15698 = DIRECTION ( 'NONE',  ( 0.3127730236694426513, -0.9498278979187093629, 0.000000000000000000 ) ) ;
#15699 = ADVANCED_FACE ( 'NONE', ( #15799 ), #16714, .T. ) ;
#15700 = CARTESIAN_POINT ( 'NONE',  ( 91.77400275106518279, -25.99489077589524300, -13.39321520033831625 ) ) ;
#15701 = CARTESIAN_POINT ( 'NONE',  ( 125.7299414775786346, 0.9020085738987339008, -11.91225656197089222 ) ) ;
#15702 = ORIENTED_EDGE ( 'NONE', *, *, #20863, .F. ) ;
#15703 = CARTESIAN_POINT ( 'NONE',  ( 111.8886348109120092, -3.383040157471821630, -19.15922257007629170 ) ) ;
#15704 = CARTESIAN_POINT ( 'NONE',  ( 124.0495485609119584, -10.36940331770106916, -15.09355782777062061 ) ) ;
#15705 = CARTESIAN_POINT ( 'NONE',  ( 119.8129079359119942, -5.444069387712269226, -19.60292469916370450 ) ) ;
#15706 = CARTESIAN_POINT ( 'NONE',  ( 111.7857214775786474, -4.159894987975828684, -8.443039665293898821 ) ) ;
#15707 = CARTESIAN_POINT ( 'NONE',  ( 107.9822546295247889, -4.863998795839590272, -18.39754474579285315 ) ) ;
#15708 = EDGE_LOOP ( 'NONE', ( #38255, #6969, #31767, #20987, #40709 ) ) ;
#15709 = CARTESIAN_POINT ( 'NONE',  ( 116.0296814775786345, -8.166667518702817929, -8.995218007635861213 ) ) ;
#15710 = CARTESIAN_POINT ( 'NONE',  ( 112.8721930757767495, -0.9924539043446216624, -17.29976612834909133 ) ) ;
#15711 = CARTESIAN_POINT ( 'NONE',  ( 124.3685014775786328, 0.4262465694468514643, -12.03445270309931736 ) ) ;
#15712 = CARTESIAN_POINT ( 'NONE',  ( 116.1431348109119881, 0.1319031606808879209, -14.10382304977623669 ) ) ;
#15713 = VECTOR ( 'NONE', #15643, 1000.000000000000000 ) ;
#15714 = CARTESIAN_POINT ( 'NONE',  ( 116.0479673908105980, -2.443475742715333965, -17.86549347949429389 ) ) ;
#15715 = CARTESIAN_POINT ( 'NONE',  ( 123.9146881442452894, 0.9020085738987452251, -11.91225656197092597 ) ) ;
#15716 = CARTESIAN_POINT ( 'NONE',  ( 116.0296814775786345, -8.166667518702817929, -8.995218007635861213 ) ) ;
#15717 = B_SPLINE_CURVE_WITH_KNOTS ( 'NONE', 3,
 ( #30627, #37457, #7122, #21032, #30851, #23801, #37691, #6464, #37910, #20373 ),
 .UNSPECIFIED., .F., .F.,
 ( 4, 3, 3, 4 ),
 ( 0.000000000000000000, 0.0001671877560959399915, 0.0003343755126089165055, 0.0006438490228512240001 ),
 .UNSPECIFIED. ) ;
#15718 = CARTESIAN_POINT ( 'NONE',  ( 110.3436608795247764, -1.325403438956436419, -16.93181055722141792 ) ) ;
#15719 = EDGE_CURVE ( 'NONE', #2333, #33578, #9405, .T. ) ;
#15720 = CARTESIAN_POINT ( 'NONE',  ( 125.3895814775786448, -7.893985811506177619, -18.51759400769804742 ) ) ;
#15721 =( LENGTH_UNIT ( ) NAMED_UNIT ( * ) SI_UNIT ( .MILLI., .METRE. ) );
#15722 = VERTEX_POINT ( 'NONE', #33784 ) ;
#15723 = CARTESIAN_POINT ( 'NONE',  ( 114.1009748109119784, -4.089484607189486809, -7.948022111789456723 ) ) ;
#15724 = CARTESIAN_POINT ( 'NONE',  ( 113.1366214775786432, -7.643976991954077427, -18.09477374809248928 ) ) ;
#15725 = AXIS2_PLACEMENT_3D ( 'NONE', #4219, #11528, #800 ) ;
#15726 = CARTESIAN_POINT ( 'NONE',  ( 35.90261398037149121, 14.17005867477686820, -8.593215200338315540 ) ) ;
#15727 = CARTESIAN_POINT ( 'NONE',  ( 113.1366214775786432, -1.834011780172310813, -8.268836392978581529 ) ) ;
#15728 = ORIENTED_EDGE ( 'NONE', *, *, #27901, .T. ) ;
#15729 = CARTESIAN_POINT ( 'NONE',  ( 118.6391081442452986, -4.089484607189486809, -7.948022111789456723 ) ) ;
#15730 = DIRECTION ( 'NONE',  ( 0.000000000000000000, 0.3818493186865928868, -0.9242245927363028635 ) ) ;
#15731 = CARTESIAN_POINT ( 'NONE',  ( 109.8574890045248367, -9.868328341294150263, -11.32035403202669777 ) ) ;
#15732 = CARTESIAN_POINT ( 'NONE',  ( 111.5599048082056868, -0.1020945015690391533, -15.74893487844545703 ) ) ;
#15733 = CARTESIAN_POINT ( 'NONE',  ( 136.9394333025907713, -2.946625990313646248, -8.232885575275636469 ) ) ;
#15734 = CARTESIAN_POINT ( 'NONE',  ( 112.6828081442453282, -2.084020599724406786, -8.691656652584148546 ) ) ;
#15735 = CARTESIAN_POINT ( 'NONE',  ( 69.69189222814998175, -41.76310523276723785, -24.39321520033831447 ) ) ;
#15736 = CARTESIAN_POINT ( 'NONE',  ( 124.7156075856321991, -3.817466558032057478, -21.12005900094969491 ) ) ;
#15737 = VECTOR ( 'NONE', #29715, 1000.000000000000000 ) ;
#15738 = CARTESIAN_POINT ( 'NONE',  ( 113.0231681442453180, -10.15424416112533912, -14.75197769757731336 ) ) ;
#15739 = CARTESIAN_POINT ( 'NONE',  ( 126.4106614775786284, -6.222761293078241884, -8.102969835052219238 ) ) ;
#15740 = CARTESIAN_POINT ( 'NONE',  ( 116.6027202256327655, -9.865431707603255163, -13.72396611541779166 ) ) ;
#15741 = CARTESIAN_POINT ( 'NONE',  ( 123.1205148109119563, -7.643976991954077427, -18.09477374809248928 ) ) ;
#15742 = DIRECTION ( 'NONE',  ( 0.8636456077245092677, -0.5040994586965584778, 0.000000000000000000 ) ) ;
#15743 = CARTESIAN_POINT ( 'NONE',  ( 124.4252281442452812, -9.261995988541697145, -16.69588392320189030 ) ) ;
#15744 = CARTESIAN_POINT ( 'NONE',  ( 122.0994348109119443, 0.9020085738987339008, -11.91225656197089222 ) ) ;
#15745 = ORIENTED_EDGE ( 'NONE', *, *, #6423, .F. ) ;
#15746 = CARTESIAN_POINT ( 'NONE',  ( 127.0298367773232400, -8.469156795426192375, -17.42115985237845521 ) ) ;
#15747 = CARTESIAN_POINT ( 'NONE',  ( 114.0941296295247867, -4.863998795839590272, -19.15521520033831493 ) ) ;
#15748 = CIRCLE ( 'NONE', #41259, 4.999999999999998224 ) ;
#15749 = CARTESIAN_POINT ( 'NONE',  ( 110.0658483795247804, -8.402594152722688392, -16.93181055722141792 ) ) ;
#15750 = CARTESIAN_POINT ( 'NONE',  ( 107.4960827545248350, -6.936859964151250502, -8.388885654883777576 ) ) ;
#15751 = EDGE_CURVE ( 'NONE', #28070, #32861, #33101, .T. ) ;
#15752 = CARTESIAN_POINT ( 'NONE',  ( 125.6732148109119862, -9.859900752359514797, -12.68260735090137459 ) ) ;
#15753 = CARTESIAN_POINT ( 'NONE',  ( 115.2922348109119781, -10.63000616557722466, -14.87417383870573495 ) ) ;
#15754 = EDGE_LOOP ( 'NONE', ( #10535, #12632 ) ) ;
#15755 = CARTESIAN_POINT ( 'NONE',  ( 124.8842416685201471, -9.531938938847675402, -19.51325999086594720 ) ) ;
#15756 = DIRECTION ( 'NONE',  ( 1.000000000000000000, 0.000000000000000000, 0.000000000000000000 ) ) ;
#15757 = CYLINDRICAL_SURFACE ( 'NONE', #1569, 0.5000000000000004441 ) ;
#15758 = CARTESIAN_POINT ( 'NONE',  ( 113.4202548109119846, 0.1319031606808879209, -14.10382304977623669 ) ) ;
#15759 = CARTESIAN_POINT ( 'NONE',  ( 113.0294866692503888, -2.311015703046748193, -18.04188382666269064 ) ) ;
#15760 = CARTESIAN_POINT ( 'NONE',  ( 120.8514481442452961, -7.893985811506177619, -18.51759400769804742 ) ) ;
#15761 = CARTESIAN_POINT ( 'NONE',  ( 108.6767858795247861, -0.7896495226426338832, -17.46756447353520159 ) ) ;
#15762 = CARTESIAN_POINT ( 'NONE',  ( 85.70478001548416103, -27.84333996136784961, -14.15691383771150136 ) ) ;
#15763 = VERTEX_POINT ( 'NONE', #43847 ) ;
#15764 = CARTESIAN_POINT ( 'NONE',  ( 110.9034820646196806, 0.6269505268395592079, -14.64321520033834645 ) ) ;
#15765 = CARTESIAN_POINT ( 'NONE',  ( 117.9583881442453048, 0.1319031606808879209, -14.10382304977623669 ) ) ;
#15766 = CARTESIAN_POINT ( 'NONE',  ( 116.3700414775786527, -5.638512984488999180, -18.83840828888717311 ) ) ;
#15767 = CARTESIAN_POINT ( 'NONE',  ( 116.0864081442453113, -9.988377603198976828, -10.36322818467138340 ) ) ;
#15768 = CARTESIAN_POINT ( 'NONE',  ( 118.1613820163423298, -1.087735405160632718, -17.17288456429612253 ) ) ;
#15769 = CARTESIAN_POINT ( 'NONE',  ( 123.2906948109119867, -1.833838273342659697, -17.42832698103878286 ) ) ;
#15770 = CARTESIAN_POINT ( 'NONE',  ( 120.5110881442453206, -3.505236298600246325, -18.68346056562440793 ) ) ;
#15771 = VERTEX_POINT ( 'NONE', #2554 ) ;
#15772 = CARTESIAN_POINT ( 'NONE',  ( 121.9659548109119811, -7.554583864224885481, -18.48844787311982785 ) ) ;
#15773 = AXIS2_PLACEMENT_3D ( 'NONE', #24469, #31301, #17193 ) ;
#15774 = CARTESIAN_POINT ( 'NONE',  ( 112.2289948109119848, -1.834011780172310813, -8.268836392978581529 ) ) ;
#15775 = CARTESIAN_POINT ( 'NONE',  ( 122.6099748109119929, -0.8288870151387760510, -10.36305467784173118 ) ) ;
#15776 = ORIENTED_EDGE ( 'NONE', *, *, #41219, .T. ) ;
#15777 = CARTESIAN_POINT ( 'NONE',  ( 72.87572422742091760, -11.86958442233774313, -21.39321520033831447 ) ) ;
#15778 = CARTESIAN_POINT ( 'NONE',  ( 115.4056881442453459, -7.893985811506177619, -18.51759400769804742 ) ) ;
#15779 = CARTESIAN_POINT ( 'NONE',  ( 106.8710046295248759, -4.863998795839590272, -18.39754474579285315 ) ) ;
#15780 = CARTESIAN_POINT ( 'NONE',  ( 115.5758681442453053, -7.894159318335828068, -9.358103419637847864 ) ) ;
#15781 = AXIS2_PLACEMENT_3D ( 'NONE', #12003, #39812, #22479 ) ;
#15782 = ORIENTED_EDGE ( 'NONE', *, *, #29573, .F. ) ;
#15783 = EDGE_LOOP ( 'NONE', ( #24740, #2210, #5748, #26623, #32557 ) ) ;
#15784 = CARTESIAN_POINT ( 'NONE',  ( 123.4041481442452834, 0.1319031606808879209, -14.10382304977623669 ) ) ;
#15785 = CARTESIAN_POINT ( 'NONE',  ( 121.4187148109119789, -3.505236298600246325, -18.68346056562440793 ) ) ;
#15786 = CARTESIAN_POINT ( 'NONE',  ( 66.30459164891361468, -14.82339685155236886, -16.39321520033831447 ) ) ;
#15787 = CIRCLE ( 'NONE', #44937, 20.00000000000000000 ) ;
#15788 = DIRECTION ( 'NONE',  ( 0.000000000000000000, 0.000000000000000000, 1.000000000000000000 ) ) ;
#15789 = DIRECTION ( 'NONE',  ( 0.000000000000000000, 0.000000000000000000, -1.000000000000000000 ) ) ;
#15790 = CARTESIAN_POINT ( 'NONE',  ( 71.90980237029992850, -25.93883227901748967, -4.893215200338314474 ) ) ;
#15791 = CARTESIAN_POINT ( 'NONE',  ( 107.4960827545248350, -2.477300249445798297, -19.15521520033831138 ) ) ;
#15792 = CARTESIAN_POINT ( 'NONE',  ( 115.5758681442453053, -1.561330072975668060, -17.79121239304076951 ) ) ;
#15794 = CARTESIAN_POINT ( 'NONE',  ( 116.4834948109119779, -7.894159318335828068, -9.358103419637847864 ) ) ;
#15793 = CARTESIAN_POINT ( 'NONE',  ( 115.8595014775786609, -1.834011780172310813, -8.268836392978581529 ) ) ;
#15795 = CARTESIAN_POINT ( 'NONE',  ( 120.2841814775786276, -10.15424416112533912, -14.75197769757731336 ) ) ;
#15796 = CARTESIAN_POINT ( 'NONE',  ( 113.1366214775786432, -1.834011780172310813, -8.268836392978581529 ) ) ;
#15797 = ORIENTED_EDGE ( 'NONE', *, *, #301, .F. ) ;
#15798 = CARTESIAN_POINT ( 'NONE',  ( 119.9438214775786378, -2.084020599724406786, -8.691656652584148546 ) ) ;
#15799 = FACE_OUTER_BOUND ( 'NONE', #7082, .T. ) ;
#15800 = CARTESIAN_POINT ( 'NONE',  ( 110.6214733795247867, -8.938348069036489818, -17.46756447353520159 ) ) ;
#15801 = DIRECTION ( 'NONE',  ( 0.9908103287288504424, -0.1352586133457951423, 0.000000000000000000 ) ) ;
#15802 = CARTESIAN_POINT ( 'NONE',  ( 113.0523327545247838, -2.477300249445798297, -19.15521520033831138 ) ) ;
#15803 = AXIS2_PLACEMENT_3D ( 'NONE', #9051, #22953, #19082 ) ;
#15804 = CARTESIAN_POINT ( 'NONE',  ( 119.3765548109119834, 0.9020085738987339008, -11.91225656197089222 ) ) ;
#15805 = ORIENTED_EDGE ( 'NONE', *, *, #5330, .T. ) ;
#15806 = CARTESIAN_POINT ( 'NONE',  ( 119.3765548109119834, 0.9020085738987339008, -11.91225656197089222 ) ) ;
#15807 = CARTESIAN_POINT ( 'NONE',  ( 123.9584548109119737, 2.753894863294152007, -15.83610205775420177 ) ) ;
#15808 = CARTESIAN_POINT ( 'NONE',  ( 108.8156921295247912, 0.8980012041604618078, -13.39321520033831447 ) ) ;
#15809 = CARTESIAN_POINT ( 'NONE',  ( 118.2987481442453088, -1.561330072975668504, -17.79121239304076951 ) ) ;
#15810 = CARTESIAN_POINT ( 'NONE',  ( 116.9373081442452929, -8.166667518702817929, -8.995218007635861213 ) ) ;
#15811 = CARTESIAN_POINT ( 'NONE',  ( 63.00984045858719185, -3.312991842083455207, -19.12743919334240417 ) ) ;
#15812 = DIRECTION ( 'NONE',  ( 1.000000000000000000, 0.000000000000000000, 0.000000000000000000 ) ) ;
#15813 = EDGE_CURVE ( 'NONE', #29158, #2916, #35192, .T. ) ;
#15814 = AXIS2_PLACEMENT_3D ( 'NONE', #43499, #12713, #33207 ) ;
#15815 = ORIENTED_EDGE ( 'NONE', *, *, #43145, .T. ) ;
#15816 = CARTESIAN_POINT ( 'NONE',  ( 31.16856251326851179, -20.50830283073288030, -18.19321520033831519 ) ) ;
#15817 = CARTESIAN_POINT ( 'NONE',  ( 109.2295007571409542, -9.177044000692852421, -16.67882263470107418 ) ) ;
#15818 = CARTESIAN_POINT ( 'NONE',  ( 118.6958348109119754, -3.505236298600246325, -18.68346056562440793 ) ) ;
#15819 = CARTESIAN_POINT ( 'NONE',  ( 113.1217858795247935, -8.402594152722688392, -9.854619843455216355 ) ) ;
#15820 = CARTESIAN_POINT ( 'NONE',  ( 112.6356140045247827, 0.1403307496149616695, -15.46607636864997204 ) ) ;
#15821 = CARTESIAN_POINT ( 'NONE',  ( 118.5256548109119876, -8.899110576539710493, -16.42337572283490132 ) ) ;
#15822 = FACE_OUTER_BOUND ( 'NONE', #1353, .T. ) ;
#15823 = CARTESIAN_POINT ( 'NONE',  ( 69.25500790402072937, -25.95870368663648975, -5.871751884747664185 ) ) ;
#15824 = CARTESIAN_POINT ( 'NONE',  ( 112.5126281442453120, 0.1319031606808879209, -14.10382304977623669 ) ) ;
#15825 = CARTESIAN_POINT ( 'NONE',  ( 124.5386814775786206, -5.638512984488999180, -18.83840828888717311 ) ) ;
#15826 = ORIENTED_EDGE ( 'NONE', *, *, #341, .T. ) ;
#15827 = CIRCLE ( 'NONE', #31114, 2.000000000000000444 ) ;
#15828 = ADVANCED_FACE ( 'NONE', ( #9872 ), #40211, .T. ) ;
#15829 = CARTESIAN_POINT ( 'NONE',  ( 117.9583881442453048, 0.1319031606808879209, -14.10382304977623669 ) ) ;
#15830 = CARTESIAN_POINT ( 'NONE',  ( 114.4413348109119823, -9.261995988541697145, -16.69588392320189030 ) ) ;
#15831 = CARTESIAN_POINT ( 'NONE',  ( 119.8303681442453126, -10.63000616557722466, -14.87417383870573495 ) ) ;
#15832 = CARTESIAN_POINT ( 'NONE',  ( 124.0281414775786146, -7.643976991954077427, -18.09477374809248928 ) ) ;
#15833 = VERTEX_POINT ( 'NONE', #19221 ) ;
#15834 = CARTESIAN_POINT ( 'NONE',  ( 125.5597614775786326, -7.894159318335828068, -9.358103419637847864 ) ) ;
#15835 = EDGE_CURVE ( 'NONE', #14254, #40113, #6395, .T. ) ;
#15836 = CARTESIAN_POINT ( 'NONE',  ( 122.9503348109119827, 0.5811942927096110934, -14.16772938898807510 ) ) ;
#15837 = CARTESIAN_POINT ( 'NONE',  ( 112.3424481442453384, -3.505236298600246325, -18.68346056562440793 ) ) ;
#15838 = VECTOR ( 'NONE', #18148, 1000.000000000000000 ) ;
#15839 = CARTESIAN_POINT ( 'NONE',  ( 111.2646414775786496, -8.899110576539710493, -16.42337572283490132 ) ) ;
#15840 = EDGE_CURVE ( 'NONE', #15917, #38098, #43863, .T. ) ;
#15841 = CARTESIAN_POINT ( 'NONE',  ( 117.4893492294923902, -2.263366209404196638, -18.10533625161307114 ) ) ;
#15842 = EDGE_CURVE ( 'NONE', #11410, #19947, #6448, .T. ) ;
#15843 = EDGE_CURVE ( 'NONE', #35580, #27652, #28199, .T. ) ;
#15844 = DIRECTION ( 'NONE',  ( 0.000000000000000000, -0.3818493186865927203, 0.9242245927363029745 ) ) ;
#15845 = CARTESIAN_POINT ( 'NONE',  ( 138.2004992774602954, -2.227975765267806274, -15.65448404533372972 ) ) ;
#15846 = CARTESIAN_POINT ( 'NONE',  ( 111.5243640045248412, 0.1403307496149616695, -15.46607636864997204 ) ) ;
#15847 = CARTESIAN_POINT ( 'NONE',  ( 70.19189222814998175, -53.33815113939435548, -34.53808368179734600 ) ) ;
#15848 = CARTESIAN_POINT ( 'NONE',  ( 137.4443952029584750, -9.944843709095133377, -13.20533582317771248 ) ) ;
#15849 = CARTESIAN_POINT ( 'NONE',  ( 118.5823814775786360, -7.643976991954077427, -18.09477374809248928 ) ) ;
#15850 = CARTESIAN_POINT ( 'NONE',  ( 124.0848681442452772, -4.089484607189486809, -7.948022111789456723 ) ) ;
#15851 = CARTESIAN_POINT ( 'NONE',  ( 69.48536631248848039, -69.56066907060868232, -44.09544185076553191 ) ) ;
#15852 = ORIENTED_EDGE ( 'NONE', *, *, #35034, .T. ) ;
#15853 = CARTESIAN_POINT ( 'NONE',  ( 117.0806140045248185, 0.1403307496149616695, -15.46607636864997204 ) ) ;
#15854 = CARTESIAN_POINT ( 'NONE',  ( 108.3295202545248657, 0.1403307496149616695, -11.32035403202665336 ) ) ;
#15855 = AXIS2_PLACEMENT_3D ( 'NONE', #34294, #13345, #33603 ) ;
#15856 = CARTESIAN_POINT ( 'NONE',  ( 114.6682414775786469, -7.894159318335828068, -9.358103419637847864 ) ) ;
#15857 = CARTESIAN_POINT ( 'NONE',  ( 113.3643610407382454, -2.419733177069680607, -17.89711025544712442 ) ) ;
#15858 = CARTESIAN_POINT ( 'NONE',  ( 65.99667006149269355, -0.1541283259764877900, -10.39321520033831270 ) ) ;
#15859 = CARTESIAN_POINT ( 'NONE',  ( 124.0622086996681901, -1.172797794773259072, -17.05961127468926719 ) ) ;
#15861 = CARTESIAN_POINT ( 'NONE',  ( 122.0994348109119443, 0.9020085738987339008, -11.91225656197089222 ) ) ;
#15860 = CARTESIAN_POINT ( 'NONE',  ( 94.86797725101187950, -26.47803208098435945, -14.15005199485239906 ) ) ;
#15862 = CARTESIAN_POINT ( 'NONE',  ( 122.2128881442453263, -7.643976991954077427, -18.09477374809248928 ) ) ;
#15863 = ORIENTED_EDGE ( 'NONE', *, *, #44553, .F. ) ;
#15864 = LINE ( 'NONE', #22920, #15874 ) ;
#15865 = CARTESIAN_POINT ( 'NONE',  ( 126.2597653975789598, 0.06634425167100366227, -14.34189767235250912 ) ) ;
#15866 = CARTESIAN_POINT ( 'NONE',  ( 110.6214733795247867, -1.325403438956436419, -9.854619843455211026 ) ) ;
#15867 = CARTESIAN_POINT ( 'NONE',  ( 121.7590748109119687, -2.084020599724406786, -8.691656652584148546 ) ) ;
#15868 = CARTESIAN_POINT ( 'NONE',  ( 121.2485348109119769, -8.899110576539710493, -16.42337572283490132 ) ) ;
#15869 = CARTESIAN_POINT ( 'NONE',  ( 124.1685108350173010, 2.742570392492192255, -15.83608568264068062 ) ) ;
#15870 = CARTESIAN_POINT ( 'NONE',  ( 110.4825671295247815, -10.62599879583958540, -13.39321520033831447 ) ) ;
#15871 = DIRECTION ( 'NONE',  ( 1.000000000000000000, 0.000000000000000000, -0.000000000000000000 ) ) ;
#15872 = CARTESIAN_POINT ( 'NONE',  ( 115.1010702440515558, -2.467220198592777525, -17.83387418641524391 ) ) ;
#15873 = DIRECTION ( 'NONE',  ( 0.000000000000000000, 1.000000000000000000, 2.168404344971010101E-16 ) ) ;
#15874 = VECTOR ( 'NONE', #23381, 1000.000000000000000 ) ;
#15875 = CARTESIAN_POINT ( 'NONE',  ( 110.0658483795247804, -0.7896495226426338832, -9.318865927141430916 ) ) ;
#15876 = CARTESIAN_POINT ( 'NONE',  ( -13.56828337869085210, -4.779084862085888119, -17.89321520033830026 ) ) ;
#15877 = CARTESIAN_POINT ( 'NONE',  ( 83.52255208528447383, -32.68847348073289538, -24.11834731266797505 ) ) ;
#15878 = CARTESIAN_POINT ( 'NONE',  ( 121.3052614775786111, -1.834011780172310813, -8.268836392978581529 ) ) ;
#15879 = CARTESIAN_POINT ( 'NONE',  ( 123.8579614775786126, 0.5811942927096110934, -14.16772938898807510 ) ) ;
#15880 = CARTESIAN_POINT ( 'NONE',  ( 107.9822546295247889, -4.863998795839590272, -7.631215200338315796 ) ) ;
#15881 = CARTESIAN_POINT ( 'NONE',  ( 116.4834948109119779, -1.561330072975668504, -17.79121239304076951 ) ) ;
#15882 = DIRECTION ( 'NONE',  ( -0.000000000000000000, -0.9284778069183718952, -0.3713878862591649677 ) ) ;
#15883 = VERTEX_POINT ( 'NONE', #14396 ) ;
#15884 = UNCERTAINTY_MEASURE_WITH_UNIT (LENGTH_MEASURE( 1.000000000000000082E-05 ), #23883, 'distance_accuracy_value', 'NONE');
#15885 = CARTESIAN_POINT ( 'NONE',  ( 70.19189222814998175, -57.62004466406304459, -36.25082616574700722 ) ) ;
#15886 = EDGE_CURVE ( 'NONE', #3470, #31689, #9656, .T. ) ;
#15887 = CARTESIAN_POINT ( 'NONE',  ( 124.5386814775786206, -5.638512984488999180, -18.83840828888717311 ) ) ;
#15888 = CARTESIAN_POINT ( 'NONE',  ( 119.5467348109119712, -4.089484607189486809, -7.948022111789456723 ) ) ;
#15889 = CARTESIAN_POINT ( 'NONE',  ( 125.8433948109119456, -7.643976991954077427, -18.09477374809248928 ) ) ;
#15890 = APPLICATION_PROTOCOL_DEFINITION ( 'draft international standard', 'automotive_design', 1998, #23302 ) ;
#15891 = CARTESIAN_POINT ( 'NONE',  ( -3.075987277002700804, -7.207016596002322473, -19.39321520033831447 ) ) ;
#15892 = CARTESIAN_POINT ( 'NONE',  ( 113.5337081442453240, -0.8288870151387760510, -10.36305467784173118 ) ) ;
#15893 = CARTESIAN_POINT ( 'NONE',  ( 126.0135748109119902, -8.166667518702819706, -8.995218007635861213 ) ) ;
#15894 = CARTESIAN_POINT ( 'NONE',  ( 109.1629577545248395, -7.250697342233347165, -7.631215200338321125 ) ) ;
#15895 = CARTESIAN_POINT ( 'NONE',  ( 119.1496481442453046, -6.222761293078241884, -8.102969835052219238 ) ) ;
#15896 = CARTESIAN_POINT ( 'NONE',  ( 84.10271796608054728, -31.10763468207608895, -20.89321520033831447 ) ) ;
#15897 = CARTESIAN_POINT ( 'NONE',  ( 70.19189222814998175, -100.0979043305785581, -53.24182196210380624 ) ) ;
#15898 = ORIENTED_EDGE ( 'NONE', *, *, #21087, .F. ) ;
#15899 = EDGE_CURVE ( 'NONE', #12976, #37160, #10101, .T. ) ;
#15900 = CARTESIAN_POINT ( 'NONE',  ( 121.3408766859119794, -9.033780868592240054, -16.85052413769862056 ) ) ;
#15901 = CARTESIAN_POINT ( 'NONE',  ( 122.2128881442453263, -1.834011780172310813, -8.268836392978581529 ) ) ;
#15902 = CARTESIAN_POINT ( 'NONE',  ( 87.14323352029596492, -25.23119213852205789, -15.24166438581092109 ) ) ;
#15903 = CARTESIAN_POINT ( 'NONE',  ( 125.0211000582878711, 1.959868932401269470, -10.14215219406585256 ) ) ;
#15904 = CARTESIAN_POINT ( 'NONE',  ( 69.69189222814998175, -41.76310523276723785, -24.89321520033831447 ) ) ;
#15905 = VECTOR ( 'NONE', #20526, 1000.000000000000114 ) ;
#15906 = CARTESIAN_POINT ( 'NONE',  ( 119.1496481442453046, -6.222761293078241884, -8.102969835052219238 ) ) ;
#15907 = CARTESIAN_POINT ( 'NONE',  ( 67.62945316293361486, -0.2852776976338805004, -16.39321520033831447 ) ) ;
#15908 = EDGE_CURVE ( 'NONE', #19850, #27673, #31491, .T. ) ;
#15909 = DIRECTION ( 'NONE',  ( 0.000000000000000000, -0.4669533266896290225, -0.8842819633428516957 ) ) ;
#15910 = CARTESIAN_POINT ( 'NONE',  ( 121.7023481442452777, -0.8288870151387760510, -10.36305467784173118 ) ) ;
#15911 = DIRECTION ( 'NONE',  ( 0.000000000000000000, 0.3713878862591642460, -0.9284778069183722282 ) ) ;
#15912 = CARTESIAN_POINT ( 'NONE',  ( 125.7299414775786346, -10.15424416112533912, -14.75197769757731336 ) ) ;
#15913 = CARTESIAN_POINT ( 'NONE',  ( 124.7774606721202986, -11.80897325920537888, -16.84910625859622968 ) ) ;
#15914 = CARTESIAN_POINT ( 'NONE',  ( 125.0492214775786266, -6.344957434206665248, -7.627207830600338134 ) ) ;
#15915 = CARTESIAN_POINT ( 'NONE',  ( 117.5045748109119756, -9.859900752359374465, -12.68260735090039404 ) ) ;
#15916 = CARTESIAN_POINT ( 'NONE',  ( 122.1561614775786353, -8.899110576539710493, -16.42337572283490132 ) ) ;
#15917 = VERTEX_POINT ( 'NONE', #44755 ) ;
#15918 = CARTESIAN_POINT ( 'NONE',  ( 121.7023481442452777, -9.261995988541697145, -16.69588392320189030 ) ) ;
#15919 = CARTESIAN_POINT ( 'NONE',  ( 115.8595014775786609, -1.834011780172310813, -8.268836392978581529 ) ) ;
#15920 = CARTESIAN_POINT ( 'NONE',  ( 114.7192077545248594, -2.791137627527939813, -18.39754474579286025 ) ) ;
#15921 = CARTESIAN_POINT ( 'NONE',  ( 112.5693548109119888, 0.4262465694468514643, -12.03445270309931736 ) ) ;
#15922 =( BOUNDED_CURVE ( )  B_SPLINE_CURVE ( 3, ( #29329, #33174, #21812, #12235 ),
 .UNSPECIFIED., .F., .T. ) 
 B_SPLINE_CURVE_WITH_KNOTS ( ( 4, 4 ),
 ( 1.570796326794895004, 1.981905665150994977 ),
 .UNSPECIFIED. ) 
 CURVE ( )  GEOMETRIC_REPRESENTATION_ITEM ( )  RATIONAL_B_SPLINE_CURVE ( ( 1.000000000000000000, 0.9859652809920760319, 0.9859652809920760319, 1.000000000000000000 ) ) 
 REPRESENTATION_ITEM ( '' )  );
#15923 = CARTESIAN_POINT ( 'NONE',  ( 124.4252281442452812, -0.8288870151387760510, -10.36305467784173118 ) ) ;
#15924 = CARTESIAN_POINT ( 'NONE',  ( 125.7299414775786346, 0.9020085738987339008, -11.91225656197089222 ) ) ;
#15925 = CARTESIAN_POINT ( 'NONE',  ( 114.9275671295247889, -10.62599879583958540, -13.39321520033831447 ) ) ;
#15926 = CARTESIAN_POINT ( 'NONE',  ( 110.0658483795247804, -8.402594152722688392, -16.93181055722141792 ) ) ;
#15927 = DIRECTION ( 'NONE',  ( -1.000000000000000000, 0.000000000000000000, 0.000000000000000000 ) ) ;
#15928 = CARTESIAN_POINT ( 'NONE',  ( 112.1722681442453222, -8.899110576539710493, -16.42337572283490132 ) ) ;
#15929 = CARTESIAN_POINT ( 'NONE',  ( 67.30914723170953096, -58.60056893040009385, -37.53754034566229336 ) ) ;
#15930 = CARTESIAN_POINT ( 'NONE',  ( 112.4272546295247821, -4.863998795839590272, -18.39754474579285315 ) ) ;
#15931 = ORIENTED_EDGE ( 'NONE', *, *, #19759, .F. ) ;
#15932 = CARTESIAN_POINT ( 'NONE',  ( 126.0703014775786102, -0.1624402480850797581, -16.17319339645315424 ) ) ;
#15933 = CARTESIAN_POINT ( 'NONE',  ( 119.8823610609119754, -6.340755971794695078, -8.611740276972781771 ) ) ;
#15934 = CARTESIAN_POINT ( 'NONE',  ( 120.0907204359119760, 1.345710702986147034, -13.97328579221134426 ) ) ;
#15935 = ORIENTED_EDGE ( 'NONE', *, *, #7278, .T. ) ;
#15936 = CARTESIAN_POINT ( 'NONE',  ( 78.69189222814998175, -49.76310523276723785, -24.89321520033831447 ) ) ;
#15937 = CARTESIAN_POINT ( 'NONE',  ( 109.0240515045248202, -6.936859964151250502, -18.39754474579286025 ) ) ;
#15938 = ORIENTED_EDGE ( 'NONE', *, *, #14765, .T. ) ;
#15939 = CARTESIAN_POINT ( 'NONE',  ( 120.1707281442453166, 0.2603800115204892296, -16.42320221600525088 ) ) ;
#15940 = CARTESIAN_POINT ( 'NONE',  ( 122.7234281442452755, -4.153390946401325223, -8.397313243818185668 ) ) ;
#15941 = CARTESIAN_POINT ( 'NONE',  ( 116.4834948109119779, -7.894159318335828068, -9.358103419637847864 ) ) ;
#15942 = DIRECTION ( 'NONE',  ( -0.9908103287288504424, 0.1352586133457951423, 0.000000000000000000 ) ) ;
#15943 = CARTESIAN_POINT ( 'NONE',  ( 128.2184548109119930, -2.475900776146301219, -7.888945235271306977 ) ) ;
#15944 = CARTESIAN_POINT ( 'NONE',  ( 115.2922348109119781, -10.63000616557722466, -14.87417383870573495 ) ) ;
#15945 = EDGE_CURVE ( 'NONE', #29611, #40557, #34242, .T. ) ;
#15946 = CARTESIAN_POINT ( 'NONE',  ( 111.5243640045248412, 0.1403307496149616695, -15.46607636864997204 ) ) ;
#15947 = CARTESIAN_POINT ( 'NONE',  ( 123.4041481442452834, -10.30919188438810075, -12.61870101168855918 ) ) ;
#15948 = DIRECTION ( 'NONE',  ( -1.000000000000000000, 0.000000000000000000, 0.000000000000000000 ) ) ;
#15949 = EDGE_LOOP ( 'NONE', ( #20482, #39412, #24479, #42553 ) ) ;
#15950 = CARTESIAN_POINT ( 'NONE',  ( 113.2500748109119968, -6.344957434206662583, -7.627207830600332805 ) ) ;
#15951 = CARTESIAN_POINT ( 'NONE',  ( 113.3068014775786594, -1.833838273342658809, -17.42832698103878286 ) ) ;
#15952 = DIRECTION ( 'NONE',  ( 0.000000000000000000, 0.3713878862591650232, -0.9284778069183718952 ) ) ;
#15953 = CARTESIAN_POINT ( 'NONE',  ( 112.1722681442453222, -0.4660016031367893996, -10.09054647747474043 ) ) ;
#15954 = VERTEX_POINT ( 'NONE', #17817 ) ;
#15955 = CARTESIAN_POINT ( 'NONE',  ( 121.3052614775786111, -1.834011780172310813, -8.268836392978581529 ) ) ;
#15956 = EDGE_CURVE ( 'NONE', #34537, #10427, #878, .T. ) ;
#15957 = DIRECTION ( 'NONE',  ( 0.000000000000000000, -0.3818493186865936084, 0.9242245927363024194 ) ) ;
#15958 = CARTESIAN_POINT ( 'NONE',  ( 107.2294421295247844, -9.051693226400931991, -21.39321520033831447 ) ) ;
#15959 = DIRECTION ( 'NONE',  ( 0.000000000000000000, 0.000000000000000000, 1.000000000000000000 ) ) ;
#15960 = CARTESIAN_POINT ( 'NONE',  ( 137.1886586612182271, -3.190032180672805140, -8.343492096882645370 ) ) ;
#15961 = CARTESIAN_POINT ( 'NONE',  ( 115.6893214775786447, -9.859900752359374465, -12.68260735090039404 ) ) ;
#15962 = CARTESIAN_POINT ( 'NONE',  ( 63.69189222814998175, -69.76310523276724496, 3.106784799661685526 ) ) ;
#15963 = CARTESIAN_POINT ( 'NONE',  ( 125.3031471548959814, -3.285148677421780405, -20.38179746482967758 ) ) ;
#15964 = CARTESIAN_POINT ( 'NONE',  ( 126.1270281442452870, -10.30919188438810075, -12.61870101168855918 ) ) ;
#15965 = CARTESIAN_POINT ( 'NONE',  ( 113.5337081442453240, -9.261995988541697145, -16.69588392320189030 ) ) ;
#15966 = CARTESIAN_POINT ( 'NONE',  ( 123.6328298109119714, -7.200787124940443817, -17.81845355600750835 ) ) ;
#15967 = VECTOR ( 'NONE', #31776, 1000.000000000000000 ) ;
#15968 = CARTESIAN_POINT ( 'NONE',  ( 111.8886348109120092, -3.383040157471821630, -19.15922257007629170 ) ) ;
#15969 = CARTESIAN_POINT ( 'NONE',  ( 115.4056881442453459, -2.084020599724406786, -8.691656652584148546 ) ) ;
#15970 = CARTESIAN_POINT ( 'NONE',  ( 123.5743281442453139, -7.893985811506177619, -18.51759400769804742 ) ) ;
#15971 = CARTESIAN_POINT ( 'NONE',  ( 122.8936081442453059, 0.2603800115204892296, -16.42320221600525088 ) ) ;
#15972 = ORIENTED_EDGE ( 'NONE', *, *, #9728, .F. ) ;
#15973 = CARTESIAN_POINT ( 'NONE',  ( 112.0588148109119828, 0.5811942927096154232, -14.16772938898807155 ) ) ;
#15974 = CARTESIAN_POINT ( 'NONE',  ( 113.3301452545248083, 0.8980012041604421569, -11.00651665394454071 ) ) ;
#15975 = CARTESIAN_POINT ( 'NONE',  ( 110.2742077545248094, -2.791137627527939813, -18.39754474579286025 ) ) ;
#15976 = CARTESIAN_POINT ( 'NONE',  ( 107.0099108795247815, -1.325403438956436419, -16.93181055722141792 ) ) ;
#15977 = CARTESIAN_POINT ( 'NONE',  ( 64.14770544480609260, -35.52995977698498109, -5.855554904209406608 ) ) ;
#15978 = CARTESIAN_POINT ( 'NONE',  ( 120.0572748109119772, -3.383040157471821630, -19.15922257007629170 ) ) ;
#15979 = ORIENTED_EDGE ( 'NONE', *, *, #13684, .T. ) ;
#15980 = CARTESIAN_POINT ( 'NONE',  ( 70.19189222814998175, -40.46710316615127567, -32.62080435916936239 ) ) ;
#15981 = CARTESIAN_POINT ( 'NONE',  ( 123.9106423109119675, -0.4387604401700495593, -15.73000352943951263 ) ) ;
#15982 = LINE ( 'NONE', #42899, #22668 ) ;
#15983 = CARTESIAN_POINT ( 'NONE',  ( 114.8384214775786489, -10.15424416112533912, -14.75197769757731336 ) ) ;
#15984 = DIRECTION ( 'NONE',  ( -0.000000000000000000, -0.9284778069183720062, -0.3713878862591650232 ) ) ;
#15985 = CARTESIAN_POINT ( 'NONE',  ( 119.9438214775786378, -7.893985811506177619, -18.51759400769804742 ) ) ;
#15986 = CARTESIAN_POINT ( 'NONE',  ( 111.3160046295247838, -4.863998795839590272, -7.631215200338315796 ) ) ;
#15987 = CARTESIAN_POINT ( 'NONE',  ( 119.3828733359170400, -2.311015703046761072, -18.04188382666269774 ) ) ;
#15988 = ORIENTED_EDGE ( 'NONE', *, *, #34509, .T. ) ;
#15989 = CARTESIAN_POINT ( 'NONE',  ( 120.6361714748722420, -0.1020945015695078478, -15.74893487844866691 ) ) ;
#15990 = CARTESIAN_POINT ( 'NONE',  ( 122.5532481442453019, 0.4262465694468514643, -12.03445270309931736 ) ) ;
#15991 = CARTESIAN_POINT ( 'NONE',  ( 120.6245414775786458, -9.988377603198976828, -10.36322818467138340 ) ) ;
#15992 = CARTESIAN_POINT ( 'NONE',  ( 112.3991748109119868, -1.833838273342658809, -17.42832698103878286 ) ) ;
#15993 = CARTESIAN_POINT ( 'NONE',  ( 115.0653281442453277, -6.344957434206662583, -7.627207830600332805 ) ) ;
#15994 = CARTESIAN_POINT ( 'NONE',  ( 135.5197384689382432, -7.252067445482663466, -18.89745628190793525 ) ) ;
#15995 = CARTESIAN_POINT ( 'NONE',  ( 122.4397948109119767, -0.1624402480850797581, -16.17319339645315424 ) ) ;
#15996 = CARTESIAN_POINT ( 'NONE',  ( 121.1918081442452859, -10.15424416112533912, -14.75197769757731336 ) ) ;
#15997 = EDGE_LOOP ( 'NONE', ( #7504, #12533 ) ) ;
#15998 = CARTESIAN_POINT ( 'NONE',  ( 83.16394245587648015, -30.76310523276723785, -21.89321520033831447 ) ) ;
#15999 = AXIS2_PLACEMENT_3D ( 'NONE', #36611, #5386, #19303 ) ;
#16000 = CARTESIAN_POINT ( 'NONE',  ( 112.7962614775786676, -3.383040157471821630, -19.15922257007629170 ) ) ;
#16001 = CARTESIAN_POINT ( 'NONE',  ( 121.0783548109119749, -9.565557343593413364, -10.61323700422348004 ) ) ;
#16002 = ORIENTED_EDGE ( 'NONE', *, *, #28641, .F. ) ;
#16003 = CARTESIAN_POINT ( 'NONE',  ( 119.8823610609119754, -3.163656168406935087, -18.89861972220014508 ) ) ;
#16004 = CARTESIAN_POINT ( 'NONE',  ( 117.1642148109119859, -9.261995988541697145, -16.69588392320189030 ) ) ;
#16005 = CARTESIAN_POINT ( 'NONE',  ( 112.6356140045247827, -10.62599879583958717, -11.00651665394454604 ) ) ;
#16006 = CARTESIAN_POINT ( 'NONE',  ( 118.0151148109119816, 0.4262465694468514643, -12.03445270309931736 ) ) ;
#16007 = EDGE_LOOP ( 'NONE', ( #14082, #329, #42972, #44580, #30344 ) ) ;
#16008 = EDGE_LOOP ( 'NONE', ( #20768, #26301, #23818, #34454, #4726 ) ) ;
#16009 = CARTESIAN_POINT ( 'NONE',  ( 124.6521348109119884, -7.894159318335828068, -9.358103419637847864 ) ) ;
#16010 = ADVANCED_FACE ( 'NONE', ( #24005 ), #10730, .T. ) ;
#16011 = CARTESIAN_POINT ( 'NONE',  ( 122.3830681442452857, -1.833838273342659697, -17.42832698103878286 ) ) ;
#16012 = CARTESIAN_POINT ( 'NONE',  ( 124.5966688623432219, -9.713577380183913590, -14.62808432448665563 ) ) ;
#16013 = DIRECTION ( 'NONE',  ( 0.000000000000000000, 1.069961080215129965E-32, -1.000000000000000000 ) ) ;
#16014 = COLOUR_RGB ( '',0.7921568627450980005, 0.8196078431372548767, 0.9333333333333333481 ) ;
#16015 = CARTESIAN_POINT ( 'NONE',  ( 118.5823814775786360, -1.834011780172310813, -8.268836392978581529 ) ) ;
#16016 = CARTESIAN_POINT ( 'NONE',  ( 105.7597546295248350, -4.863998795839590272, -7.631215200338315796 ) ) ;
#16017 = CARTESIAN_POINT ( 'NONE',  ( 115.0086014775786509, -4.089484607189486809, -7.948022111789456723 ) ) ;
#16019 = CARTESIAN_POINT ( 'NONE',  ( 115.7460481442453357, -10.15424416112533912, -14.75197769757731336 ) ) ;
#16018 = CARTESIAN_POINT ( 'NONE',  ( 116.6536748109119941, 0.9020085738987339008, -11.91225656197089222 ) ) ;
#16020 = CARTESIAN_POINT ( 'NONE',  ( 123.1772414775786189, -5.574606645277164318, -18.38911715685844683 ) ) ;
#16021 = CARTESIAN_POINT ( 'NONE',  ( 112.9664414775786412, 0.5811942927096154232, -14.16772938898807155 ) ) ;
#16022 = VERTEX_POINT ( 'NONE', #35802 ) ;
#16023 = CARTESIAN_POINT ( 'NONE',  ( 121.7023481442452919, -0.8288870151387760510, -10.36305467784173118 ) ) ;
#16024 = DIRECTION ( 'NONE',  ( 1.000000000000000000, 0.000000000000000000, 0.000000000000000000 ) ) ;
#16025 = CARTESIAN_POINT ( 'NONE',  ( 85.82015659721905365, -25.23119213852205789, -15.24166438581092109 ) ) ;
#16026 = CARTESIAN_POINT ( 'NONE',  ( 114.8581140045248361, -10.62599879583958717, -11.00651665394454604 ) ) ;
#16027 = CARTESIAN_POINT ( 'NONE',  ( 114.3024890045248156, -9.868328341294098749, -11.32035403202665869 ) ) ;
#16028 = CARTESIAN_POINT ( 'NONE',  ( 111.4549108795247747, -8.938348069036489818, -9.318865927141430916 ) ) ;
#16029 = AXIS2_PLACEMENT_3D ( 'NONE', #29880, #19848, #26467 ) ;
#16030 = CARTESIAN_POINT ( 'NONE',  ( 118.8092881442453290, -9.988377603198976828, -10.36322818467138340 ) ) ;
#16031 = ORIENTED_EDGE ( 'NONE', *, *, #7485, .F. ) ;
#16032 = CARTESIAN_POINT ( 'NONE',  ( 119.8303681442453126, -10.63000616557722466, -14.87417383870573495 ) ) ;
#16033 = PLANE ( 'NONE',  #42921 ) ;
#16034 = CARTESIAN_POINT ( 'NONE',  ( 106.8710046295248759, -4.863998795839590272, -7.631215200338315796 ) ) ;
#16035 = CARTESIAN_POINT ( 'NONE',  ( 118.2420214775786320, -3.383040157471821630, -19.15922257007629170 ) ) ;
#16036 = CARTESIAN_POINT ( 'NONE',  ( 121.4754414775786131, -8.166667518702819706, -8.995218007635861213 ) ) ;
#16037 = CARTESIAN_POINT ( 'NONE',  ( 64.65425730835187323, -2.684632774272076805, -18.61636701123672921 ) ) ;
#16038 = CARTESIAN_POINT ( 'NONE',  ( 116.8344096179147442, -11.69876286440622692, -6.100568865546136088 ) ) ;
#16039 = EDGE_LOOP ( 'NONE', ( #17861, #23908 ) ) ;
#16040 = DIRECTION ( 'NONE',  ( 1.000000000000000000, 0.000000000000000000, 0.000000000000000000 ) ) ;
#16041 = AXIS2_PLACEMENT_3D ( 'NONE', #832, #14751, #35932 ) ;
#16042 = CARTESIAN_POINT ( 'NONE',  ( 109.2296186286734638, -9.487811336982241883, -16.25376729502801254 ) ) ;
#16043 = CARTESIAN_POINT ( 'NONE',  ( 125.6732148109119862, -9.859900752359378018, -12.68260735090039759 ) ) ;
#16045 = CARTESIAN_POINT ( 'NONE',  ( 112.4272546295247821, -4.863998795839590272, -18.39754474579285315 ) ) ;
#16044 = APPLICATION_CONTEXT ( 'automotive_design' ) ;
#16046 = CARTESIAN_POINT ( 'NONE',  ( 110.8298327545248299, -6.936859964151250502, -8.388885654883777576 ) ) ;
#16047 = CARTESIAN_POINT ( 'NONE',  ( 119.3765548109119834, -10.15424416112533912, -14.75197769757731336 ) ) ;
#16048 = DIRECTION ( 'NONE',  ( 0.7871354856660167654, -0.6167752151498625546, -0.002461946824136807422 ) ) ;
#16049 = CARTESIAN_POINT ( 'NONE',  ( 69.77874801882427391, -26.16868962091858464, -5.786137840895065665 ) ) ;
#16050 = CARTESIAN_POINT ( 'NONE',  ( 111.4348214775786801, -3.505236298600246325, -18.68346056562440793 ) ) ;
#16051 = CARTESIAN_POINT ( 'NONE',  ( 125.0492214775786266, -6.344957434206665248, -7.627207830600338134 ) ) ;
#16052 = ORIENTED_EDGE ( 'NONE', *, *, #29888, .T. ) ;
#16053 = CARTESIAN_POINT ( 'NONE',  ( 121.9859814775786333, -9.565557343593413364, -10.61323700422348004 ) ) ;
#16054 = CARTESIAN_POINT ( 'NONE',  ( 115.5191414775786569, -3.383040157471821630, -19.15922257007629170 ) ) ;
#16055 = CARTESIAN_POINT ( 'NONE',  ( 121.8158014775786171, -5.638512984488999180, -18.83840828888717311 ) ) ;
#16056 = PRODUCT_RELATED_PRODUCT_CATEGORY ( 'part', '', ( #38304 ) ) ;
#16057 = CARTESIAN_POINT ( 'NONE',  ( 124.8790414775786246, -8.899110576539710493, -16.42337572283490132 ) ) ;
#16058 = ORIENTED_EDGE ( 'NONE', *, *, #5527, .F. ) ;
#16059 = CARTESIAN_POINT ( 'NONE',  ( 143.3676850761856940, -69.76310523276724496, -0.9932152003383157846 ) ) ;
#16060 = CARTESIAN_POINT ( 'NONE',  ( 122.6099748109119929, -9.261995988541697145, -16.69588392320189030 ) ) ;
#16061 = AXIS2_PLACEMENT_3D ( 'NONE', #31841, #7222, #21135 ) ;
#16062 = FACE_OUTER_BOUND ( 'NONE', #20106, .T. ) ;
#16063 = CARTESIAN_POINT ( 'NONE',  ( 111.7184548109119788, -0.8288870151387760510, -10.36305467784173118 ) ) ;
#16064 = CARTESIAN_POINT ( 'NONE',  ( 106.8710046295248759, -4.863998795839590272, -7.631215200338315796 ) ) ;
#16065 = CARTESIAN_POINT ( 'NONE',  ( 120.9241579359119925, -4.360204210389833968, -8.000047426360245240 ) ) ;
#16066 = CARTESIAN_POINT ( 'NONE',  ( 118.7315769107182177, -2.467220198592778413, -17.83387418641524391 ) ) ;
#16067 = CARTESIAN_POINT ( 'NONE',  ( 111.3160046295247838, -4.863998795839590272, -18.39754474579285315 ) ) ;
#16068 = CIRCLE ( 'NONE', #3695, 1.587500000000000799 ) ;
#16069 = CARTESIAN_POINT ( 'NONE',  ( 63.12337091419462354, -3.603895683774054781, -17.39321520033831447 ) ) ;
#16070 = AXIS2_PLACEMENT_3D ( 'NONE', #19394, #2058, #27320 ) ;
#16071 = CARTESIAN_POINT ( 'NONE',  ( 119.8303681442453126, 0.4262465694468514643, -12.03445270309931736 ) ) ;
#16072 = CARTESIAN_POINT ( 'NONE',  ( 111.4348214775786801, -3.505236298600246325, -18.68346056562440793 ) ) ;
#16073 = CARTESIAN_POINT ( 'NONE',  ( 125.1269327111056953, -1.267766418764818770, -16.93314635290698078 ) ) ;
#16074 = ORIENTED_EDGE ( 'NONE', *, *, #8044, .T. ) ;
#16075 = CARTESIAN_POINT ( 'NONE',  ( 117.1500671295247713, 0.1403307496149613920, -13.39321520033831447 ) ) ;
#16076 = CARTESIAN_POINT ( 'NONE',  ( 118.0151148109119816, 0.4262465694468514643, -12.03445270309931736 ) ) ;
#16077 = CARTESIAN_POINT ( 'NONE',  ( 113.0231681442453180, -10.15424416112533912, -14.75197769757731336 ) ) ;
#16078 = CARTESIAN_POINT ( 'NONE',  ( 67.37843845263206788, -0.1674546162330892152, -10.39321520033831625 ) ) ;
#16079 = DIRECTION ( 'NONE',  ( 1.000000000000000000, 0.000000000000000000, -0.000000000000000000 ) ) ;
#16081 = CARTESIAN_POINT ( 'NONE',  ( 123.5176014775786228, -9.261995988541697145, -16.69588392320189030 ) ) ;
#16080 = CARTESIAN_POINT ( 'NONE',  ( 79.00611218289952831, -44.99489077589586827, -23.89321520033831803 ) ) ;
#16082 = CARTESIAN_POINT ( 'NONE',  ( 124.0281414775786146, -7.643976991954077427, -18.09477374809248928 ) ) ;
#16083 = VERTEX_POINT ( 'NONE', #35345 ) ;
#16084 = DIRECTION ( 'NONE',  ( 0.000000000000000000, 0.6004852223388321697, -0.7996358532186279566 ) ) ;
#16085 = DIRECTION ( 'NONE',  ( 0.7871354856660167654, -0.6167752151498625546, -0.002461946824136807422 ) ) ;
#16086 = CARTESIAN_POINT ( 'NONE',  ( 112.1494421295248003, -9.868328341294093420, -13.39321520033831447 ) ) ;
#16087 = CARTESIAN_POINT ( 'NONE',  ( 120.9649014775786355, -6.222761293078241884, -8.102969835052219238 ) ) ;
#16088 = CARTESIAN_POINT ( 'NONE',  ( 118.1852948109119836, -4.153390946401325223, -8.397313243818185668 ) ) ;
#16089 = CARTESIAN_POINT ( 'NONE',  ( 124.9063227527188928, 1.280016537245024066, -17.97972868380785627 ) ) ;
#16090 = CARTESIAN_POINT ( 'NONE',  ( 113.4690515045247992, -6.936859964151250502, -18.39754474579286025 ) ) ;
#16091 = DIRECTION ( 'NONE',  ( 0.000000000000000000, -0.3818493186865927203, 0.9242245927363029745 ) ) ;
#16092 = CYLINDRICAL_SURFACE ( 'NONE', #1931, 4.999999999999997335 ) ;
#16093 = AXIS2_PLACEMENT_3D ( 'NONE', #39642, #15927, #22530 ) ;
#16094 = DIRECTION ( 'NONE',  ( 0.2768435750659360983, 0.3568721902840809590, -0.8921882507333046552 ) ) ;
#16095 = CARTESIAN_POINT ( 'NONE',  ( 110.6909265045248247, -7.250697342233347165, -19.15521520033831138 ) ) ;
#16096 = B_SPLINE_CURVE_WITH_KNOTS ( 'NONE', 3,
 ( #41519, #31230, #44716, #20977, #44940, #10276, #30792, #41301, #30564, #34850 ),
 .UNSPECIFIED., .F., .F.,
 ( 4, 3, 3, 4 ),
 ( 8.673617379884039324E-19, 0.0001671877560958089928, 0.0003343755126086570017, 0.0006438490228505489759 ),
 .UNSPECIFIED. ) ;
#16097 = EDGE_CURVE ( 'NONE', #24723, #5058, #42890, .T. ) ;
#16098 = CARTESIAN_POINT ( 'NONE',  ( 70.89841814381148311, -71.67679885123182260, -38.80507129598510119 ) ) ;
#16099 = CARTESIAN_POINT ( 'NONE',  ( 114.3719421295247827, 0.8980012041604618078, -13.39321520033831447 ) ) ;
#16100 = CARTESIAN_POINT ( 'NONE',  ( 120.9081748109119872, -5.638512984488999180, -18.83840828888717311 ) ) ;
#16101 = CARTESIAN_POINT ( 'NONE',  ( 123.2906948109119867, -8.166667518702819706, -8.995218007635861213 ) ) ;
#16102 = CARTESIAN_POINT ( 'NONE',  ( 105.8986608795248401, -8.938348069036489818, -9.318865927141430916 ) ) ;
#16103 = CARTESIAN_POINT ( 'NONE',  ( 117.2209414775786485, -7.893985811506177619, -18.51759400769804742 ) ) ;
#16104 = EDGE_CURVE ( 'NONE', #25316, #16340, #42667, .T. ) ;
#16105 = EDGE_CURVE ( 'NONE', #37436, #5895, #3804, .T. ) ;
#16106 = ORIENTED_EDGE ( 'NONE', *, *, #4499, .T. ) ;
#16107 = CARTESIAN_POINT ( 'NONE',  ( 109.3534539124563736, 0.06785227275816346770, -12.14321520033833046 ) ) ;
#16108 = CARTESIAN_POINT ( 'NONE',  ( 112.3991748109119868, -1.833838273342658809, -17.42832698103878286 ) ) ;
#16109 = CIRCLE ( 'NONE', #44526, 1.199999999999999512 ) ;
#16110 = CARTESIAN_POINT ( 'NONE',  ( 120.9081748109119872, -5.638512984488999180, -18.83840828888717311 ) ) ;
#16111 = CARTESIAN_POINT ( 'NONE',  ( 112.1155414775786454, 0.9020085738987339008, -11.91225656197089222 ) ) ;
#16112 = CARTESIAN_POINT ( 'NONE',  ( 114.1577014775786552, -3.505236298600246325, -18.68346056562440793 ) ) ;
#16113 = EDGE_LOOP ( 'NONE', ( #36253, #9446, #9201, #12564, #34732, #18755, #16636, #14427, #41885, #29446, #34768, #34851, #36758 ) ) ;
#16114 = VECTOR ( 'NONE', #32372, 1000.000000000000114 ) ;
#16115 = CARTESIAN_POINT ( 'NONE',  ( 112.5693548109119888, 0.4262465694468514643, -12.03445270309931736 ) ) ;
#16116 = CARTESIAN_POINT ( 'NONE',  ( 124.8790414775786246, -0.4660016031367893996, -10.09054647747474043 ) ) ;
#16117 = CARTESIAN_POINT ( 'NONE',  ( 110.9687390045248350, 0.8980012041604421569, -15.77991374673208469 ) ) ;
#16118 = CARTESIAN_POINT ( 'NONE',  ( 118.5823814775786360, -7.643976991954077427, -18.09477374809248928 ) ) ;
#16119 = CARTESIAN_POINT ( 'NONE',  ( 116.8155157646764479, -2.029803478747229661, -17.78032935472251097 ) ) ;
#16120 = CARTESIAN_POINT ( 'NONE',  ( 124.4862981477679824, -2.280480477428469488, -18.08254604495227014 ) ) ;
#16121 = VERTEX_POINT ( 'NONE', #8456 ) ;
#16122 = CARTESIAN_POINT ( 'NONE',  ( 121.8270485609119760, -0.08252387247370887580, -11.91645802438286417 ) ) ;
#16123 = CARTESIAN_POINT ( 'NONE',  ( 123.9146881442452894, 0.9020085738987339008, -11.91225656197089222 ) ) ;
#16124 = EDGE_CURVE ( 'NONE', #18680, #29964, #10371, .T. ) ;
#16125 = DIRECTION ( 'NONE',  ( -1.000000000000000000, 0.000000000000000000, 0.000000000000000000 ) ) ;
#16126 = CARTESIAN_POINT ( 'NONE',  ( 123.2697102440515238, -2.467220198592778413, -17.83387418641524391 ) ) ;
#16127 = CARTESIAN_POINT ( 'NONE',  ( 122.1743141859119817, -0.8832429491016114964, -18.19431474523657499 ) ) ;
#16128 = DIRECTION ( 'NONE',  ( -1.000000000000000000, 6.760077337439384200E-16, 0.000000000000000000 ) ) ;
#16129 = EDGE_CURVE ( 'NONE', #5448, #14305, #35098, .T. ) ;
#16130 = CARTESIAN_POINT ( 'NONE',  ( 108.1211608795247798, -1.325403438956436419, -16.93181055722141792 ) ) ;
#16131 = LINE ( 'NONE', #40756, #355 ) ;
#16132 = CARTESIAN_POINT ( 'NONE',  ( 124.9924948109119924, -5.574606645277164318, -18.38911715685844683 ) ) ;
#16133 = EDGE_CURVE ( 'NONE', #18524, #32644, #15517, .T. ) ;
#16134 = AXIS2_PLACEMENT_3D ( 'NONE', #3686, #50, #14630 ) ;
#16135 = CARTESIAN_POINT ( 'NONE',  ( 125.3368646685608923, -11.73513648066642290, -15.14777030654274803 ) ) ;
#16136 = CARTESIAN_POINT ( 'NONE',  ( 123.7054579359119941, -5.367357518394499927, -18.78171702160300782 ) ) ;
#16137 = CARTESIAN_POINT ( 'NONE',  ( 117.7882081442453170, -3.505236298600246325, -18.68346056562440793 ) ) ;
#16138 = DIRECTION ( 'NONE',  ( -1.000000000000000000, 0.000000000000000000, -0.000000000000000000 ) ) ;
#16139 = VERTEX_POINT ( 'NONE', #932 ) ;
#16140 = CARTESIAN_POINT ( 'NONE',  ( 121.4187148109119789, -6.344957434206665248, -7.627207830600338134 ) ) ;
#16142 = B_SPLINE_CURVE_WITH_KNOTS ( 'NONE', 3,
 ( #25368, #21936, #35375, #18964 ),
 .UNSPECIFIED., .F., .F.,
 ( 4, 4 ),
 ( 0.000000000000000000, 1.000000000000000000 ),
 .UNSPECIFIED. ) ;
#16141 = CARTESIAN_POINT ( 'NONE',  ( 116.0296814775786345, -8.166667518702817929, -8.995218007635861213 ) ) ;
#16143 = CARTESIAN_POINT ( 'NONE',  ( 113.4690515045247992, -6.936859964151250502, -18.39754474579286025 ) ) ;
#16144 = DIRECTION ( 'NONE',  ( 0.000000000000000000, -0.6004852223388321697, 0.7996358532186280677 ) ) ;
#16145 = CARTESIAN_POINT ( 'NONE',  ( 122.4965214775786251, 0.1319031606808879209, -14.10382304977623669 ) ) ;
#16146 = CARTESIAN_POINT ( 'NONE',  ( 122.8936081442453059, 0.2603800115204892296, -16.42320221600525088 ) ) ;
#16147 = CARTESIAN_POINT ( 'NONE',  ( 114.8581140045248361, -10.62599879583958717, -11.00651665394454604 ) ) ;
#16148 = CARTESIAN_POINT ( 'NONE',  ( 107.1488171295248861, 0.1403307496149613920, -13.39321520033831447 ) ) ;
#16149 = CARTESIAN_POINT ( 'NONE',  ( 83.24289279524387553, -31.94143910891574123, -23.46319239529895384 ) ) ;
#16150 = CARTESIAN_POINT ( 'NONE',  ( 114.3846081442453197, 0.4262465694468514643, -12.03445270309931736 ) ) ;
#16151 = CARTESIAN_POINT ( 'NONE',  ( 116.3133148109120043, -2.084020599724406786, -8.691656652584148546 ) ) ;
#16152 = LINE ( 'NONE', #9533, #6592 ) ;
#16153 = CARTESIAN_POINT ( 'NONE',  ( 114.0246765045248196, -2.791137627527939813, -8.388885654883777576 ) ) ;
#16154 = ORIENTED_EDGE ( 'NONE', *, *, #40694, .T. ) ;
#16155 = ADVANCED_FACE ( 'NONE', ( #11653 ), #2589, .T. ) ;
#16156 = CARTESIAN_POINT ( 'NONE',  ( 70.89841814381148311, -68.89136543047671069, -37.69090763720760151 ) ) ;
#16157 = CARTESIAN_POINT ( 'NONE',  ( 126.0135748109119902, -1.833838273342660141, -17.42832698103878286 ) ) ;
#16158 = CARTESIAN_POINT ( 'NONE',  ( 119.8129079359119942, -4.360204210389833968, -8.000047426360245240 ) ) ;
#16159 = CARTESIAN_POINT ( 'NONE',  ( 121.3408766859119794, -0.06289925094097943703, -9.412459353600674206 ) ) ;
#16160 = ADVANCED_FACE ( 'NONE', ( #41008 ), #20916, .F. ) ;
#16161 = EDGE_CURVE ( 'NONE', #17596, #16972, #17486, .T. ) ;
#16162 = EDGE_LOOP ( 'NONE', ( #32988, #929, #20522, #34000 ) ) ;
#16163 = DIRECTION ( 'NONE',  ( 0.000000000000000000, 0.3818493186865927203, -0.9242245927363029745 ) ) ;
#16164 = CARTESIAN_POINT ( 'NONE',  ( 111.4665458264767750, -1.295815253274133161, -16.89579513612386563 ) ) ;
#16165 = ORIENTED_EDGE ( 'NONE', *, *, #18214, .T. ) ;
#16166 = CARTESIAN_POINT ( 'NONE',  ( 119.6034614775786196, -6.344957434206665248, -7.627207830600338134 ) ) ;
#16167 = VECTOR ( 'NONE', #38812, 1000.000000000000000 ) ;
#16168 = CARTESIAN_POINT ( 'NONE',  ( 122.8936081442453059, -9.565557343593413364, -10.61323700422348004 ) ) ;
#16169 = CARTESIAN_POINT ( 'NONE',  ( 113.1933481442453058, -5.574606645277164318, -18.38911715685844683 ) ) ;
#16170 = CARTESIAN_POINT ( 'NONE',  ( 116.0872410407382347, -2.419733177069680607, -17.89711025544712442 ) ) ;
#16171 = CARTESIAN_POINT ( 'NONE',  ( 71.91396631829535124, -25.73035770285813939, -4.893215200338314474 ) ) ;
#16172 = CARTESIAN_POINT ( 'NONE',  ( 116.3700414775786527, -5.638512984488999180, -18.83840828888717311 ) ) ;
#16173 = CARTESIAN_POINT ( 'NONE',  ( 114.0246765045248196, -2.791137627527939813, -8.388885654883777576 ) ) ;
#16174 = VECTOR ( 'NONE', #28704, 1000.000000000000227 ) ;
#16175 = CARTESIAN_POINT ( 'NONE',  ( 124.8223148109119762, 0.9020085738987339008, -11.91225656197089222 ) ) ;
#16176 =( NAMED_UNIT ( * ) SI_UNIT ( $, .STERADIAN. ) SOLID_ANGLE_UNIT ( ) );
#16177 = ORIENTED_EDGE ( 'NONE', *, *, #21711, .T. ) ;
#16178 = CARTESIAN_POINT ( 'NONE',  ( 115.8027748109119841, -0.4660016031367893996, -10.09054647747474043 ) ) ;
#16179 = CARTESIAN_POINT ( 'NONE',  ( 115.4056881442453459, -2.084020599724406786, -8.691656652584148546 ) ) ;
#16180 = DIRECTION ( 'NONE',  ( 0.000000000000000000, 0.000000000000000000, -1.000000000000000000 ) ) ;
#16181 = CARTESIAN_POINT ( 'NONE',  ( 125.5030348109119558, -6.222761293078241884, -8.102969835052219238 ) ) ;
#16182 = ORIENTED_EDGE ( 'NONE', *, *, #28917, .T. ) ;
#16183 = CARTESIAN_POINT ( 'NONE',  ( 123.0637881442452937, -0.4660016031367893996, -10.09054647747474043 ) ) ;
#16184 = CARTESIAN_POINT ( 'NONE',  ( 60.06931813437629586, -14.72076136720887085, -8.603412892520118760 ) ) ;
#16185 = CARTESIAN_POINT ( 'NONE',  ( 109.7880358795247986, -8.402594152722736354, -9.854619843455244776 ) ) ;
#16186 = LINE ( 'NONE', #40352, #12017 ) ;
#16187 = CARTESIAN_POINT ( 'NONE',  ( 137.0134976903340203, -3.008273255399957158, -8.264431575293873067 ) ) ;
#16188 = CARTESIAN_POINT ( 'NONE',  ( 113.8173414775786512, -9.565557343593413364, -10.61323700422348004 ) ) ;
#16189 = CARTESIAN_POINT ( 'NONE',  ( 75.95778847736481509, -3.256761025687722189, -18.79321520033831661 ) ) ;
#16190 = AXIS2_PLACEMENT_3D ( 'NONE', #44649, #13411, #10211 ) ;
#16191 = FACE_OUTER_BOUND ( 'NONE', #3799, .T. ) ;
#16192 = CARTESIAN_POINT ( 'NONE',  ( 114.9518748109119883, -7.643976991954077427, -18.09477374809248928 ) ) ;
#16193 = CARTESIAN_POINT ( 'NONE',  ( 114.1009748109119784, -4.089484607189486809, -7.948022111789456723 ) ) ;
#16194 = CARTESIAN_POINT ( 'NONE',  ( 122.4521266859119635, -9.033780868592240054, -16.85052413769862056 ) ) ;
#16195 = CARTESIAN_POINT ( 'NONE',  ( 113.8740681442453138, 0.5811942927096154232, -14.16772938898807155 ) ) ;
#16196 = CARTESIAN_POINT ( 'NONE',  ( 116.7671281442453335, -7.643976991954077427, -18.09477374809248928 ) ) ;
#16197 = CARTESIAN_POINT ( 'NONE',  ( 123.3474214775786209, -9.988377603198976828, -10.36322818467138340 ) ) ;
#16198 = B_SPLINE_CURVE_WITH_KNOTS ( 'NONE', 3,
 ( #25928, #29119, #33194, #8820, #15668, #22500, #36621, #29569, #12704, #40289, #1301, #33412, #32528, #2192, #30021, #16119, #9280, #23188, #43031, #15213, #37066, #30248, #6070, #17251, #6763, #10408, #23876, #34332, #13602, #20672, #45062, #27291, #41650, #41430, #44621, #33877, #3106, #40744, #13387, #44393, #12935, #41204, #2646, #16578, #31139, #10187, #24093, #23645, #37987, #34548, #17033, #9502 ),
 .UNSPECIFIED., .F., .F.,
 ( 4, 2, 2, 2, 1, 1, 2, 2, 2, 2, 2, 1, 1, 1, 2, 2, 2, 2, 1, 1, 1, 2, 2, 2, 2, 2, 1, 1, 2, 2, 4 ),
 ( 0.000000000000000000, 0.1250000000000105471, 0.1875000000000157652, 0.2187500000000184019, 0.2343750000000194844, 0.2421875000000199563, 0.2460937500000202061, 0.2500000000000204281, 0.3750000000000289213, 0.4375000000000331402, 0.4687500000000358047, 0.4843750000000378031, 0.4921875000000388023, 0.4960937500000392464, 0.4980468750000394684, 0.5000000000000396350, 0.5625000000000532907, 0.5937500000000599520, 0.6093750000000628386, 0.6171875000000638378, 0.6210937500000648370, 0.6230468750000655032, 0.6250000000000660583, 0.6875000000000504041, 0.7187500000000430767, 0.7343750000000398570, 0.7421875000000383027, 0.7460937500000374145, 0.7480468750000370814, 0.7500000000000366374, 1.000000000000000000 ),
 .UNSPECIFIED. ) ;
#16199 = ADVANCED_FACE ( 'NONE', ( #31383 ), #6557, .T. ) ;
#16200 = CARTESIAN_POINT ( 'NONE',  ( 120.1140014775786398, -1.561330072975668504, -17.79121239304076951 ) ) ;
#16201 = EDGE_LOOP ( 'NONE', ( #3815, #10712, #26968, #21041, #32970 ) ) ;
#16202 = CARTESIAN_POINT ( 'NONE',  ( 112.5693548109119888, -10.63000616557722466, -14.87417383870573495 ) ) ;
#16203 = CARTESIAN_POINT ( 'NONE',  ( 110.5520202545248054, -10.62599879583958717, -15.77991374673208469 ) ) ;
#16204 = CARTESIAN_POINT ( 'NONE',  ( 107.9128015045248219, -6.936859964151250502, -18.39754474579286025 ) ) ;
#16205 = VECTOR ( 'NONE', #14097, 1000.000000000000000 ) ;
#16206 = CARTESIAN_POINT ( 'NONE',  ( 109.5796765045248122, -2.791137627527939813, -8.388885654883777576 ) ) ;
#16207 = CARTESIAN_POINT ( 'NONE',  ( 127.7425183523502881, -7.050714571525749541, -18.72418924296322729 ) ) ;
#16208 = CARTESIAN_POINT ( 'NONE',  ( 120.1140014775786398, -1.561330072975668504, -17.79121239304076951 ) ) ;
#16209 = ORIENTED_EDGE ( 'NONE', *, *, #32304, .T. ) ;
#16210 = CARTESIAN_POINT ( 'NONE',  ( 114.3339130180080758, 0.7607806665038616689, -14.64321520033833579 ) ) ;
#16211 = CARTESIAN_POINT ( 'NONE',  ( 109.2294508954661154, -7.975540152821279705, -8.597489492498922914 ) ) ;
#16212 = CYLINDRICAL_SURFACE ( 'NONE', #33618, 1.999999999999998890 ) ;
#16213 = CARTESIAN_POINT ( 'NONE',  ( 116.0296814775786345, -1.833838273342658809, -17.42832698103878286 ) ) ;
#16214 = CARTESIAN_POINT ( 'NONE',  ( 105.6208483795248299, -8.402594152722688392, -16.93181055722141792 ) ) ;
#16215 = CARTESIAN_POINT ( 'NONE',  ( 118.1852948109119836, -5.638512984488999180, -18.83840828888717311 ) ) ;
#16216 = CARTESIAN_POINT ( 'NONE',  ( 105.4819421295248247, 0.8980012041604618078, -13.39321520033831447 ) ) ;
#16217 = DIRECTION ( 'NONE',  ( 0.000000000000000000, 0.3713878862591642460, -0.9284778069183722282 ) ) ;
#16218 = ORIENTED_EDGE ( 'NONE', *, *, #9439, .T. ) ;
#16219 = CARTESIAN_POINT ( 'NONE',  ( 121.2485348109119769, -8.899110576539744244, -16.42337572283485514 ) ) ;
#16220 = CARTESIAN_POINT ( 'NONE',  ( 123.0637881442452937, -8.899110576539710493, -16.42337572283490132 ) ) ;
#16221 = CARTESIAN_POINT ( 'NONE',  ( 120.5678148109119832, -8.166667518702819706, -8.995218007635861213 ) ) ;
#16222 = CARTESIAN_POINT ( 'NONE',  ( 112.5693548109119888, 0.4262465694468514643, -12.03445270309931736 ) ) ;
#16223 = CARTESIAN_POINT ( 'NONE',  ( 114.8951481442453115, -0.4660016031367893996, -10.09054647747474043 ) ) ;
#16224 = CARTESIAN_POINT ( 'NONE',  ( 119.1871698793805194, -2.191907684172563986, -18.20049396185734025 ) ) ;
#16225 = EDGE_CURVE ( 'NONE', #1124, #16653, #20249, .T. ) ;
#16226 = CARTESIAN_POINT ( 'NONE',  ( 126.2184548109108135, -0.9345830046690825066, -10.29922024082877030 ) ) ;
#16227 = CARTESIAN_POINT ( 'NONE',  ( 120.3409081442453044, -8.899110576539710493, -16.42337572283490132 ) ) ;
#16228 = ORIENTED_EDGE ( 'NONE', *, *, #27906, .F. ) ;
#16229 = AXIS2_PLACEMENT_3D ( 'NONE', #24407, #17564, #31238 ) ;
#16230 = CARTESIAN_POINT ( 'NONE',  ( 119.7169148109119874, -9.988377603198960841, -10.36322818467135853 ) ) ;
#16231 = TOROIDAL_SURFACE ( 'NONE', #32216, 8.800000000000000711, 1.199999999999999956 ) ;
#16232 = CARTESIAN_POINT ( 'NONE',  ( 114.1577014775786552, -6.344957434206662583, -7.627207830600332805 ) ) ;
#16233 = CARTESIAN_POINT ( 'NONE',  ( 121.5321681442453183, -0.1624402480850797581, -16.17319339645315424 ) ) ;
#16234 = ORIENTED_EDGE ( 'NONE', *, *, #6940, .F. ) ;
#16235 = CARTESIAN_POINT ( 'NONE',  ( 122.5215798109119874, -7.200787124940443817, -17.81845355600750835 ) ) ;
#16236 = CARTESIAN_POINT ( 'NONE',  ( 116.9940348109119839, -9.988377603198976828, -10.36322818467138340 ) ) ;
#16237 = CARTESIAN_POINT ( 'NONE',  ( 113.8857702545248003, -10.62599879583958717, -15.77991374673208469 ) ) ;
#16238 = CARTESIAN_POINT ( 'NONE',  ( 115.3489614775786407, -0.8288870151387760510, -10.36305467784173118 ) ) ;
#16239 = ORIENTED_EDGE ( 'NONE', *, *, #9432, .T. ) ;
#16240 = VECTOR ( 'NONE', #37535, 1000.000000000000000 ) ;
#16241 = VERTEX_POINT ( 'NONE', #3135 ) ;
#16242 = CARTESIAN_POINT ( 'NONE',  ( 126.5808414775786446, -9.859900752359378018, -12.68260735090039759 ) ) ;
#16243 = CARTESIAN_POINT ( 'NONE',  ( 121.6456214775786293, 0.4262465694468514643, -12.03445270309931736 ) ) ;
#16244 =( NAMED_UNIT ( * ) PLANE_ANGLE_UNIT ( ) SI_UNIT ( $, .RADIAN. ) );
#16245 = PLANE ( 'NONE',  #43990 ) ;
#16246 = CARTESIAN_POINT ( 'NONE',  ( 118.6958348109119754, -6.344957434206665248, -7.627207830600338134 ) ) ;
#16247 = CARTESIAN_POINT ( 'NONE',  ( 107.5655358795247736, -0.7896495226426338832, -17.46756447353520159 ) ) ;
#16248 = CARTESIAN_POINT ( 'NONE',  ( 114.4980614775786592, -7.893985811506177619, -18.51759400769804742 ) ) ;
#16250 = CARTESIAN_POINT ( 'NONE',  ( 116.7104014775786425, -8.899110576539710493, -16.42337572283490132 ) ) ;
#16249 = CARTESIAN_POINT ( 'NONE',  ( 116.9940348109119839, -9.988377603198976828, -10.36322818467138340 ) ) ;
#16251 = FACE_OUTER_BOUND ( 'NONE', #32364, .T. ) ;
#16252 = CARTESIAN_POINT ( 'NONE',  ( 114.0442481442453300, -1.834011780172310813, -8.268836392978581529 ) ) ;
#16253 = ORIENTED_EDGE ( 'NONE', *, *, #24211, .T. ) ;
#16254 = CARTESIAN_POINT ( 'NONE',  ( 123.4608748109119745, 0.4262465694468514643, -12.03445270309931736 ) ) ;
#16255 = CYLINDRICAL_SURFACE ( 'NONE', #23470, 8.000000000000001776 ) ;
#16256 = AXIS2_PLACEMENT_3D ( 'NONE', #41256, #16624, #40794 ) ;
#16257 = CARTESIAN_POINT ( 'NONE',  ( 120.8160396737536928, -8.611453504372539314, -17.77011218421760574 ) ) ;
#16258 = CARTESIAN_POINT ( 'NONE',  ( 113.8163171295247764, -10.62599879583958540, -13.39321520033831447 ) ) ;
#16259 = AXIS2_PLACEMENT_3D ( 'NONE', #23839, #40938, #482 ) ;
#16260 = CARTESIAN_POINT ( 'NONE',  ( 113.3301452545248083, -9.868328341294098749, -15.46607636864997204 ) ) ;
#16261 = CARTESIAN_POINT ( 'NONE',  ( 109.9269421295247753, 0.8980012041604618078, -13.39321520033831447 ) ) ;
#16262 = CARTESIAN_POINT ( 'NONE',  ( 122.3830681442452857, -8.166667518702819706, -8.995218007635861213 ) ) ;
#16263 = ORIENTED_EDGE ( 'NONE', *, *, #1047, .T. ) ;
#16264 = CARTESIAN_POINT ( 'NONE',  ( 119.2063748109119814, -1.561330072975668504, -17.79121239304076951 ) ) ;
#16265 = DIRECTION ( 'NONE',  ( 0.9609149988134837450, -0.1028163501681639419, 0.2570431154366518145 ) ) ;
#16266 = CARTESIAN_POINT ( 'NONE',  ( 121.0783548109119749, 0.2603800115204892296, -16.42320221600525088 ) ) ;
#16267 = CARTESIAN_POINT ( 'NONE',  ( 122.2696148109119889, -4.089484607189486809, -7.948022111789456723 ) ) ;
#16268 = CARTESIAN_POINT ( 'NONE',  ( 61.69084222814998242, -4.863998795839590272, -13.39321520033831447 ) ) ;
#16269 = CARTESIAN_POINT ( 'NONE',  ( 125.3895814775786448, -2.084020599724406786, -8.691656652584148546 ) ) ;
#16270 = CARTESIAN_POINT ( 'NONE',  ( 115.8027748109119841, -0.4660016031367859024, -10.09054647747474398 ) ) ;
#16271 = CARTESIAN_POINT ( 'NONE',  ( 120.9241579359119925, -4.360204210389833968, -8.000047426360245240 ) ) ;
#16272 = VERTEX_POINT ( 'NONE', #34135 ) ;
#16273 = CIRCLE ( 'NONE', #29376, 1.300000000000000044 ) ;
#16274 = DIRECTION ( 'NONE',  ( -0.4461977533474357771, -0.3417300876246960328, 0.8271203734159368048 ) ) ;
#16275 = CARTESIAN_POINT ( 'NONE',  ( 85.70478001548416103, -25.99489077589524300, -13.39321520033831447 ) ) ;
#16276 = CARTESIAN_POINT ( 'NONE',  ( 124.5386814775786206, -4.153390946401325223, -8.397313243818185668 ) ) ;
#16277 = EDGE_CURVE ( 'NONE', #42739, #12720, #38662, .T. ) ;
#16278 = CARTESIAN_POINT ( 'NONE',  ( 109.4407702545248355, 0.1403307496149616695, -11.32035403202665336 ) ) ;
#16279 = CARTESIAN_POINT ( 'NONE',  ( 110.6909265045248247, -2.791137627527939813, -8.388885654883777576 ) ) ;
#16280 = CARTESIAN_POINT ( 'NONE',  ( 117.1074881442453233, 0.4262465694468514643, -12.03445270309931736 ) ) ;
#16281 = DIRECTION ( 'NONE',  ( 1.000000000000000000, 0.000000000000000000, -0.000000000000000000 ) ) ;
#16282 = CARTESIAN_POINT ( 'NONE',  ( 68.68839935636917460, -25.95913848132418522, -5.893215200338315363 ) ) ;
#16283 = CARTESIAN_POINT ( 'NONE',  ( 126.0135748109119902, -8.166667518702819706, -8.995218007635861213 ) ) ;
#16284 = CARTESIAN_POINT ( 'NONE',  ( 123.7445081442452874, -1.561330072975668948, -17.79121239304076951 ) ) ;
#16285 = ORIENTED_EDGE ( 'NONE', *, *, #16097, .F. ) ;
#16286 = CARTESIAN_POINT ( 'NONE',  ( 123.4041481442452834, 0.1319031606808879209, -14.10382304977623669 ) ) ;
#16287 = CARTESIAN_POINT ( 'NONE',  ( 113.7606148109119886, -1.561330072975668060, -17.79121239304076596 ) ) ;
#16288 = CARTESIAN_POINT ( 'NONE',  ( 124.4819548109119722, -7.893985811506177619, -18.51759400769804742 ) ) ;
#16289 = CARTESIAN_POINT ( 'NONE',  ( 124.4819548109119722, -2.084020599724406786, -8.691656652584148546 ) ) ;
#16290 = VERTEX_POINT ( 'NONE', #154 ) ;
#16291 = CARTESIAN_POINT ( 'NONE',  ( 123.5053694832010365, -2.324775150319219108, -18.02356106541841996 ) ) ;
#16292 = CIRCLE ( 'NONE', #22110, 2.000000000000001776 ) ;
#16293 = CARTESIAN_POINT ( 'NONE',  ( 123.0637881442452937, -0.4660016031367893996, -10.09054647747474043 ) ) ;
#16294 = EDGE_CURVE ( 'NONE', #44020, #23032, #16958, .T. ) ;
#16295 = CARTESIAN_POINT ( 'NONE',  ( 113.9307948109119764, -10.15424416112533912, -14.75197769757731336 ) ) ;
#16296 = CARTESIAN_POINT ( 'NONE',  ( 124.7655881442452852, 0.5811942927096110934, -14.16772938898807510 ) ) ;
#16297 = CARTESIAN_POINT ( 'NONE',  ( 108.2600671295247992, -10.62599879583958540, -13.39321520033831447 ) ) ;
#16298 = CARTESIAN_POINT ( 'NONE',  ( 65.52504830115719869, -2.484121567297625788, -10.46358271731430989 ) ) ;
#16299 = ORIENTED_EDGE ( 'NONE', *, *, #20436, .F. ) ;
#16300 = CARTESIAN_POINT ( 'NONE',  ( 136.6129451145462212, -0.8699563032188813994, -17.46288999909464934 ) ) ;
#16301 = CARTESIAN_POINT ( 'NONE',  ( 109.9963952545248134, -9.868328341294098749, -15.46607636864997204 ) ) ;
#16302 = CARTESIAN_POINT ( 'NONE',  ( 109.2294421295247844, -49.76310523276723785, -19.39321520033831447 ) ) ;
#16303 = CARTESIAN_POINT ( 'NONE',  ( 120.8514481442452961, -2.084020599724406786, -8.691656652584148546 ) ) ;
#16304 = CARTESIAN_POINT ( 'NONE',  ( 112.2857214775786474, -5.574606645277164318, -18.38911715685844683 ) ) ;
#16305 = CARTESIAN_POINT ( 'NONE',  ( 126.4603288065483042, -6.163241521340323992, -18.34700366797996196 ) ) ;
#16306 = ORIENTED_EDGE ( 'NONE', *, *, #16975, .T. ) ;
#16307 = CARTESIAN_POINT ( 'NONE',  ( 116.5281640045247684, -9.863998795839588496, -11.32214738847284075 ) ) ;
#16308 = CARTESIAN_POINT ( 'NONE',  ( 115.9162281442453235, -5.574606645277164318, -18.38911715685844683 ) ) ;
#16309 = DIRECTION ( 'NONE',  ( -0.000000000000000000, -0.9284778069183721172, -0.3713878862591650232 ) ) ;
#16310 = DIRECTION ( 'NONE',  ( 0.000000000000000000, 0.000000000000000000, -1.000000000000000000 ) ) ;
#16311 = CARTESIAN_POINT ( 'NONE',  ( 111.6050014775786536, 0.1319031606808879209, -14.10382304977623669 ) ) ;
#16313 = CARTESIAN_POINT ( 'NONE',  ( 124.3117748109119844, -10.30919188438810075, -12.61870101168855918 ) ) ;
#16312 = CARTESIAN_POINT ( 'NONE',  ( 64.46696884417693241, -15.35047623415474405, -15.89321305673442986 ) ) ;
#16314 = CARTESIAN_POINT ( 'NONE',  ( 112.6260814775786514, -9.261995988541697145, -16.69588392320189030 ) ) ;
#16315 = ORIENTED_EDGE ( 'NONE', *, *, #7152, .T. ) ;
#16316 = CARTESIAN_POINT ( 'NONE',  ( 77.25325688895158294, -4.012910213732562070, -7.993215200338315007 ) ) ;
#16317 = CARTESIAN_POINT ( 'NONE',  ( 126.9932531981160224, 0.2252732323729688124, -15.16052778375922117 ) ) ;
#16318 = CARTESIAN_POINT ( 'NONE',  ( 112.0799890045248475, -9.868328341294098749, -11.32035403202665869 ) ) ;
#16319 = CARTESIAN_POINT ( 'NONE',  ( 124.8223148109119762, -10.15424416112533912, -14.75197769757731336 ) ) ;
#16321 = CIRCLE ( 'NONE', #27974, 2.000000000000000888 ) ;
#16320 = CARTESIAN_POINT ( 'NONE',  ( 120.2841814775786276, -10.15424416112533912, -14.75197769757731336 ) ) ;
#16322 = CARTESIAN_POINT ( 'NONE',  ( 125.0211000582883685, 2.260053046519062026, -15.91956964709736333 ) ) ;
#16323 = CARTESIAN_POINT ( 'NONE',  ( 113.5385046295247804, -4.863998795839590272, -18.39754474579285315 ) ) ;
#16324 = DIRECTION ( 'NONE',  ( -0.2768435750659241079, -0.3568721902840695792, 0.8921882507333129819 ) ) ;
#16325 = LINE ( 'NONE', #34527, #34703 ) ;
#16326 = FACE_OUTER_BOUND ( 'NONE', #25816, .T. ) ;
#16327 = CARTESIAN_POINT ( 'NONE',  ( 110.8992858795247827, -0.7896495226426338832, -17.46756447353520159 ) ) ;
#16328 = CARTESIAN_POINT ( 'NONE',  ( 114.2330358795247776, -0.7896495226426338832, -17.46756447353520159 ) ) ;
#16329 = CARTESIAN_POINT ( 'NONE',  ( 120.3976348109119812, -1.834011780172310813, -8.268836392978581529 ) ) ;
#16330 = CARTESIAN_POINT ( 'NONE',  ( 122.7801548109119665, -3.383040157471821630, -19.15922257007629170 ) ) ;
#16331 = DIRECTION ( 'NONE',  ( -1.000000000000000000, 0.000000000000000000, 0.000000000000000000 ) ) ;
#16332 = CARTESIAN_POINT ( 'NONE',  ( 116.3133148109119759, -7.893985811506177619, -18.51759400769804742 ) ) ;
#16333 = DIRECTION ( 'NONE',  ( 0.000000000000000000, -0.6004852223388327248, 0.7996358532186277346 ) ) ;
#16334 = ORIENTED_EDGE ( 'NONE', *, *, #27250, .F. ) ;
#16335 = CARTESIAN_POINT ( 'NONE',  ( 112.5126281442453120, 0.1319031606808879209, -14.10382304977623669 ) ) ;
#16336 = CARTESIAN_POINT ( 'NONE',  ( 126.2404814775786264, -9.261995988541697145, -16.69588392320189030 ) ) ;
#16337 = CARTESIAN_POINT ( 'NONE',  ( 119.3198281442452924, 0.5811942927096110934, -14.16772938898807510 ) ) ;
#16338 = CARTESIAN_POINT ( 'NONE',  ( 112.8529881442453302, -1.561330072975668060, -17.79121239304076596 ) ) ;
#16339 = CARTESIAN_POINT ( 'NONE',  ( 126.1270281442452870, -10.30919188438810075, -12.61870101168855918 ) ) ;
#16340 = VERTEX_POINT ( 'NONE', #6788 ) ;
#16341 = CARTESIAN_POINT ( 'NONE',  ( 119.2063748109119814, -7.894159318335828068, -9.358103419637847864 ) ) ;
#16342 = CARTESIAN_POINT ( 'NONE',  ( 111.4348214775786801, -3.505236298600246325, -18.68346056562440793 ) ) ;
#16343 = CARTESIAN_POINT ( 'NONE',  ( 109.0240515045248202, -2.477300249445798297, -7.631215200338321125 ) ) ;
#16344 = CARTESIAN_POINT ( 'NONE',  ( 121.3619881442452879, -5.574606645277164318, -18.38911715685844683 ) ) ;
#16345 = CARTESIAN_POINT ( 'NONE',  ( 90.45092582798827152, -25.99489077589524300, -13.39321520033831625 ) ) ;
#16346 = CARTESIAN_POINT ( 'NONE',  ( 124.6329298793804981, -2.191907684172563986, -18.20049396185734025 ) ) ;
#16347 = ORIENTED_EDGE ( 'NONE', *, *, #7871, .T. ) ;
#16348 = AXIS2_PLACEMENT_3D ( 'NONE', #32374, #688, #29411 ) ;
#16349 = CARTESIAN_POINT ( 'NONE',  ( 122.7299391859119737, -1.406689858478933353, -17.56299727309130887 ) ) ;
#16350 = CARTESIAN_POINT ( 'NONE',  ( 122.0994348109119443, 0.9020085738987339008, -11.91225656197089222 ) ) ;
#16351 = CYLINDRICAL_SURFACE ( 'NONE', #1451, 8.000000000000001776 ) ;
#16352 = CARTESIAN_POINT ( 'NONE',  ( 112.3424481442453384, -6.344957434206662583, -7.627207830600332805 ) ) ;
#16353 = CARTESIAN_POINT ( 'NONE',  ( 74.66232006577804725, -2.500611837642884527, -7.993215200338315007 ) ) ;
#16354 = LINE ( 'NONE', #44182, #39106 ) ;
#16355 = CARTESIAN_POINT ( 'NONE',  ( 108.0517077545248696, -2.791137627527939813, -18.39754474579286025 ) ) ;
#16356 = EDGE_CURVE ( 'NONE', #17364, #13419, #21290, .T. ) ;
#16357 = CARTESIAN_POINT ( 'NONE',  ( 121.1325173109119788, 0.2312338769422696283, -16.08380026872395874 ) ) ;
#16358 = CARTESIAN_POINT ( 'NONE',  ( 137.1968316989235461, -4.676744372166964148, -18.70090856814179503 ) ) ;
#16359 = DIRECTION ( 'NONE',  ( -1.000000000000000000, 0.000000000000000000, -0.000000000000000000 ) ) ;
#16360 = CARTESIAN_POINT ( 'NONE',  ( 124.3305360609119816, -6.339478340643663223, -8.615877017535705562 ) ) ;
#16361 = CARTESIAN_POINT ( 'NONE',  ( 123.0070614775786169, -10.15424416112533912, -14.75197769757731336 ) ) ;
#16362 = CARTESIAN_POINT ( 'NONE',  ( 119.7434548109119561, 0.4099171239737569583, -13.35943364252451460 ) ) ;
#16363 = EDGE_LOOP ( 'NONE', ( #36882, #3034, #34835, #32341, #43710 ) ) ;
#16364 = CARTESIAN_POINT ( 'NONE',  ( 124.4819548109119722, -7.893985811506177619, -18.51759400769804742 ) ) ;
#16365 = CARTESIAN_POINT ( 'NONE',  ( 116.3133148109119759, -7.893985811506177619, -18.51759400769804742 ) ) ;
#16366 = CARTESIAN_POINT ( 'NONE',  ( 114.9275671295247889, 0.1403307496149613920, -13.39321520033831447 ) ) ;
#16367 = CARTESIAN_POINT ( 'NONE',  ( 113.0231681442453180, -10.15424416112533912, -14.75197769757731336 ) ) ;
#16368 = CARTESIAN_POINT ( 'NONE',  ( 111.7751814775786556, -7.893985811506177619, -18.51759400769804742 ) ) ;
#16369 = CARTESIAN_POINT ( 'NONE',  ( 125.1059481442452750, -8.166667518702819706, -8.995218007635861213 ) ) ;
#16370 = CARTESIAN_POINT ( 'NONE',  ( 114.1635827545248389, -2.477300249445798297, -19.15521520033831138 ) ) ;
#16371 = CARTESIAN_POINT ( 'NONE',  ( 110.3436608795247764, -1.325403438956436419, -16.93181055722141792 ) ) ;
#16372 = CARTESIAN_POINT ( 'NONE',  ( 116.4555358795247884, -0.7896495226426338832, -17.46756447353520159 ) ) ;
#16373 = AXIS2_PLACEMENT_3D ( 'NONE', #4002, #20688, #17924 ) ;
#16374 = CARTESIAN_POINT ( 'NONE',  ( 116.5402214775786405, -9.565557343593413364, -10.61323700422348004 ) ) ;
#16375 = CARTESIAN_POINT ( 'NONE',  ( 115.8595014775786609, -7.643976991954077427, -18.09477374809248928 ) ) ;
#16376 = CARTESIAN_POINT ( 'NONE',  ( 137.1126581146637307, -2.246346642084271927, -18.12800035012696398 ) ) ;
#16377 = CARTESIAN_POINT ( 'NONE',  ( 113.5385046295247804, -4.863998795839590272, -18.39754474579285315 ) ) ;
#16378 = EDGE_LOOP ( 'NONE', ( #31883, #37777, #38203, #289, #13334 ) ) ;
#16379 = CARTESIAN_POINT ( 'NONE',  ( 109.2296175750677918, -0.1364591305989521774, -15.31803853156103479 ) ) ;
#16380 = CARTESIAN_POINT ( 'NONE',  ( 124.7655881442452852, -9.859900752359378018, -12.68260735090039759 ) ) ;
#16381 = CARTESIAN_POINT ( 'NONE',  ( 123.5633766859119760, -0.06289925094097943703, -9.412459353600674206 ) ) ;
#16382 = CARTESIAN_POINT ( 'NONE',  ( 120.9936110609119737, -6.340755971794695078, -8.611740276972781771 ) ) ;
#16383 = ORIENTED_EDGE ( 'NONE', *, *, #32967, .F. ) ;
#16384 = CARTESIAN_POINT ( 'NONE',  ( 67.30914723170953096, -57.67209112348172084, -37.16615245940312207 ) ) ;
#16385 = AXIS2_PLACEMENT_3D ( 'NONE', #43724, #15455, #36856 ) ;
#16386 = CARTESIAN_POINT ( 'NONE',  ( 117.1051842552189868, -11.31802912314491394, -21.73478718693168688 ) ) ;
#16387 = EDGE_CURVE ( 'NONE', #43753, #38363, #27850, .T. ) ;
#16388 = ORIENTED_EDGE ( 'NONE', *, *, #9786, .T. ) ;
#16389 = CARTESIAN_POINT ( 'NONE',  ( 119.0929214775786278, -5.638512984488999180, -18.83840828888717311 ) ) ;
#16390 = CARTESIAN_POINT ( 'NONE',  ( 124.7088614775786226, -9.565557343593413364, -10.61323700422348004 ) ) ;
#16391 = CARTESIAN_POINT ( 'NONE',  ( 115.1787814775786387, -0.1624402480850797581, -16.17319339645315424 ) ) ;
#16392 = FILL_AREA_STYLE_COLOUR ( '', #27134 ) ;
#16393 = CARTESIAN_POINT ( 'NONE',  ( 67.84197459855160162, -60.15404070048191443, -37.99358876332483703 ) ) ;
#16394 = CARTESIAN_POINT ( 'NONE',  ( 122.5532481442453019, -10.63000616557722466, -14.87417383870573495 ) ) ;
#16395 = EDGE_CURVE ( 'NONE', #9155, #7716, #5335, .T. ) ;
#16396 = CARTESIAN_POINT ( 'NONE',  ( 115.0086014775786509, -4.089484607189486809, -7.948022111789456723 ) ) ;
#16397 = EDGE_CURVE ( 'NONE', #21643, #31933, #33011, .T. ) ;
#16398 = CARTESIAN_POINT ( 'NONE',  ( 112.0799890045248475, -9.868328341294098749, -11.32035403202665869 ) ) ;
#16399 = CARTESIAN_POINT ( 'NONE',  ( 124.7088614775786226, 0.2603800115204892296, -16.42320221600525088 ) ) ;
#16400 = CARTESIAN_POINT ( 'NONE',  ( 71.02242295334774269, -99.02728775972636299, -55.91838671430374319 ) ) ;
#16401 = VERTEX_POINT ( 'NONE', #17711 ) ;
#16402 = CARTESIAN_POINT ( 'NONE',  ( 116.4267681442453153, -3.383040157471821630, -19.15922257007629170 ) ) ;
#16403 = CARTESIAN_POINT ( 'NONE',  ( 112.9664414775786412, -9.859900752359374465, -12.68260735090039404 ) ) ;
#16404 = DIRECTION ( 'NONE',  ( 0.000000000000000000, -0.3713878862591650232, 0.9284778069183718952 ) ) ;
#16405 = CARTESIAN_POINT ( 'NONE',  ( 126.6375681442452930, -10.15424416112533912, -14.75197769757731336 ) ) ;
#16406 = CIRCLE ( 'NONE', #1092, 4.500000000000003553 ) ;
#16407 = VERTEX_POINT ( 'NONE', #35467 ) ;
#16408 = CARTESIAN_POINT ( 'NONE',  ( 123.5176014775786228, -9.261995988541697145, -16.69588392320189030 ) ) ;
#16409 = CARTESIAN_POINT ( 'NONE',  ( 61.69189222814998175, -49.76310523276723785, -19.39321520033831447 ) ) ;
#16410 = CARTESIAN_POINT ( 'NONE',  ( 110.4384831777918805, -0.01829820670803256055, -14.64321520033831447 ) ) ;
#16411 = EDGE_CURVE ( 'NONE', #21347, #37027, #33643, .T. ) ;
#16412 = CARTESIAN_POINT ( 'NONE',  ( 128.2184548109119930, -4.863998795839242995, -13.39321520033831447 ) ) ;
#16413 = CARTESIAN_POINT ( 'NONE',  ( 114.7249681442453237, -9.565557343593413364, -10.61323700422348004 ) ) ;
#16414 = EDGE_CURVE ( 'NONE', #30603, #31353, #7664, .T. ) ;
#16415 = ADVANCED_FACE ( 'NONE', ( #25458 ), #19833, .T. ) ;
#16416 = CARTESIAN_POINT ( 'NONE',  ( 112.3781902440515665, -2.467220198592768199, -17.83387418641523325 ) ) ;
#16417 = AXIS2_PLACEMENT_3D ( 'NONE', #13767, #3047, #17190 ) ;
#16418 = CARTESIAN_POINT ( 'NONE',  ( 118.0151148109119816, 0.4262465694468514643, -12.03445270309931736 ) ) ;
#16419 = CARTESIAN_POINT ( 'NONE',  ( 71.57611010347959279, -63.26350616798967508, -43.68287050948689654 ) ) ;
#16420 = FACE_OUTER_BOUND ( 'NONE', #26863, .T. ) ;
#16421 = CARTESIAN_POINT ( 'NONE',  ( 116.0296814775786345, -1.833838273342658809, -17.42832698103878286 ) ) ;
#16422 = CARTESIAN_POINT ( 'NONE',  ( 114.2711548109119803, -9.988377603198976828, -10.36322818467138340 ) ) ;
#16423 = CARTESIAN_POINT ( 'NONE',  ( 120.0212673109119805, 0.2312338769422704887, -16.08380026872395874 ) ) ;
#16424 = CARTESIAN_POINT ( 'NONE',  ( 126.1270281442452870, 0.1319031606808879209, -14.10382304977623669 ) ) ;
#16425 = CARTESIAN_POINT ( 'NONE',  ( 115.7460481442453357, -10.15424416112533912, -14.75197769757731336 ) ) ;
#16426 = CARTESIAN_POINT ( 'NONE',  ( 121.5321681442453183, -9.988377603198976828, -10.36322818467138340 ) ) ;
#16427 = CARTESIAN_POINT ( 'NONE',  ( 122.6099748109119929, -9.261995988541697145, -16.69588392320189030 ) ) ;
#16428 = ORIENTED_EDGE ( 'NONE', *, *, #20834, .F. ) ;
#16429 = CARTESIAN_POINT ( 'NONE',  ( 114.1577014775786552, -6.344957434206662583, -7.627207830600332805 ) ) ;
#16430 = CARTESIAN_POINT ( 'NONE',  ( 112.1494421295248003, 0.8980012041604618078, -13.39321520033831447 ) ) ;
#16431 = CARTESIAN_POINT ( 'NONE',  ( 107.6349890045248401, -9.868328341294098749, -11.32035403202665869 ) ) ;
#16432 = CARTESIAN_POINT ( 'NONE',  ( 90.06246830635160450, -25.38011337280982715, -14.88121679464376257 ) ) ;
#16433 = CARTESIAN_POINT ( 'NONE',  ( 109.7185827545248600, -2.477300249445798297, -19.15521520033832203 ) ) ;
#16434 = CARTESIAN_POINT ( 'NONE',  ( 118.6391081442452986, -4.089484607189486809, -7.948022111789456723 ) ) ;
#16435 = ORIENTED_EDGE ( 'NONE', *, *, #10396, .T. ) ;
#16436 = DIRECTION ( 'NONE',  ( -0.1736481776669309696, -0.9848077530122079093, 0.000000000000000000 ) ) ;
#16437 = CARTESIAN_POINT ( 'NONE',  ( 138.2184548109119930, -6.243778871467079661, -12.80482167309617125 ) ) ;
#16438 = CARTESIAN_POINT ( 'NONE',  ( 112.9097148109120070, -9.565557343593413364, -10.61323700422348004 ) ) ;
#16439 = CARTESIAN_POINT ( 'NONE',  ( 123.4939235609119663, 0.6414057260225851653, -11.69287257290601723 ) ) ;
#16440 = CARTESIAN_POINT ( 'NONE',  ( 119.8303681442453126, -10.63000616557722466, -14.87417383870573495 ) ) ;
#16441 = CARTESIAN_POINT ( 'NONE',  ( 106.8710046295248759, -4.863998795839590272, -7.631215200338315796 ) ) ;
#16442 = DIRECTION ( 'NONE',  ( 1.000000000000000000, 0.000000000000000000, 0.000000000000000000 ) ) ;
#16443 = AXIS2_PLACEMENT_3D ( 'NONE', #6660, #44747, #21006 ) ;
#16444 = ORIENTED_EDGE ( 'NONE', *, *, #38125, .T. ) ;
#16445 = CARTESIAN_POINT ( 'NONE',  ( 71.62928943233082180, 0.3619606153155430217, -19.39321520033831447 ) ) ;
#16446 = CARTESIAN_POINT ( 'NONE',  ( 121.0783548109119749, -9.565557343593413364, -10.61323700422348004 ) ) ;
#16447 = CARTESIAN_POINT ( 'NONE',  ( 121.3619881442452879, -4.089484607189486809, -7.948022111789456723 ) ) ;
#16448 = CARTESIAN_POINT ( 'NONE',  ( 113.0798948109119948, -8.899110576539710493, -16.42337572283490132 ) ) ;
#16449 = CARTESIAN_POINT ( 'NONE',  ( 115.4624148109119943, -5.638512984488999180, -18.83840828888717311 ) ) ;
#16450 = CARTESIAN_POINT ( 'NONE',  ( 118.3179530757767566, -0.9924539043446216624, -17.29976612834909133 ) ) ;
#16451 = CARTESIAN_POINT ( 'NONE',  ( 126.3444272079795354, -1.084470278792948328, -10.02424450363365338 ) ) ;
#16452 = CARTESIAN_POINT ( 'NONE',  ( 119.5467348109119712, -5.574606645277164318, -18.38911715685844683 ) ) ;
#16453 = ORIENTED_EDGE ( 'NONE', *, *, #27284, .T. ) ;
#16454 = AXIS2_PLACEMENT_3D ( 'NONE', #26328, #12886, #5788 ) ;
#16455 = CARTESIAN_POINT ( 'NONE',  ( 122.6604860609119640, -6.564341423271550902, -7.887810678476487425 ) ) ;
#16456 = CARTESIAN_POINT ( 'NONE',  ( 114.7249681442453237, 0.2603800115204892296, -16.42320221600525088 ) ) ;
#16457 = CARTESIAN_POINT ( 'NONE',  ( 120.8514481442452961, -2.084020599724406786, -8.691656652584148546 ) ) ;
#16458 = ORIENTED_EDGE ( 'NONE', *, *, #28971, .T. ) ;
#16459 = CARTESIAN_POINT ( 'NONE',  ( 121.1325173109119788, -9.289237151508434209, -11.05642687123711276 ) ) ;
#16460 = CARTESIAN_POINT ( 'NONE',  ( 119.2063748109119814, -1.561330072975668504, -17.79121239304076951 ) ) ;
#16461 = CARTESIAN_POINT ( 'NONE',  ( 110.8992858795247827, -0.7896495226426338832, -17.46756447353520159 ) ) ;
#16462 = CARTESIAN_POINT ( 'NONE',  ( 115.6325948109119821, -9.565557343593413364, -10.61323700422348004 ) ) ;
#16463 = VERTEX_POINT ( 'NONE', #21580 ) ;
#16464 = ORIENTED_EDGE ( 'NONE', *, *, #20284, .F. ) ;
#16465 = CARTESIAN_POINT ( 'NONE',  ( 124.7088614775786226, -9.565557343593413364, -10.61323700422348004 ) ) ;
#16466 = AXIS2_PLACEMENT_3D ( 'NONE', #31335, #2852, #38181 ) ;
#16467 = CARTESIAN_POINT ( 'NONE',  ( 120.2274548109119934, -9.859900752359378018, -12.68260735090039759 ) ) ;
#16468 = CARTESIAN_POINT ( 'NONE',  ( 72.54180985774836188, -56.01452643456254776, -34.87945145442834871 ) ) ;
#16469 = EDGE_CURVE ( 'NONE', #7750, #39662, #38998, .T. ) ;
#16470 = DIRECTION ( 'NONE',  ( 0.000000000000000000, 0.000000000000000000, -1.000000000000000000 ) ) ;
#16471 = CARTESIAN_POINT ( 'NONE',  ( 119.2631014775786298, 0.2603800115204892296, -16.42320221600525088 ) ) ;
#16472 = CARTESIAN_POINT ( 'NONE',  ( 105.6903015045248253, -2.477300249445798297, -7.631215200338321125 ) ) ;
#16473 = CARTESIAN_POINT ( 'NONE',  ( 118.2987481442453088, -1.561330072975668504, -17.79121239304076951 ) ) ;
#16475 = CARTESIAN_POINT ( 'NONE',  ( 119.2631014775786298, -9.565557343593413364, -10.61323700422348004 ) ) ;
#16474 = CARTESIAN_POINT ( 'NONE',  ( 116.3133148109119759, -7.893985811506177619, -18.51759400769804742 ) ) ;
#16476 = EDGE_CURVE ( 'NONE', #19714, #40981, #10193, .T. ) ;
#16477 = PRODUCT_DEFINITION ( 'UNKNOWN', '', #20609, #37918 ) ;
#16478 = CARTESIAN_POINT ( 'NONE',  ( 125.2194014775786286, 0.1319031606808879209, -14.10382304977623669 ) ) ;
#16479 = CARTESIAN_POINT ( 'NONE',  ( 112.3424481442453384, -6.344957434206662583, -7.627207830600332805 ) ) ;
#16480 = VERTEX_POINT ( 'NONE', #36818 ) ;
#16481 = VECTOR ( 'NONE', #15789, 1000.000000000000000 ) ;
#16482 = CARTESIAN_POINT ( 'NONE',  ( 121.7590748109119687, -2.084020599724406786, -8.691656652584148546 ) ) ;
#16483 = LINE ( 'NONE', #24604, #24919 ) ;
#16484 = CARTESIAN_POINT ( 'NONE',  ( 120.9590811593281785, -8.517053830703083861, -17.59134500557228620 ) ) ;
#16485 = CARTESIAN_POINT ( 'NONE',  ( 109.7880358795247986, -0.7896495226426338832, -17.46756447353520159 ) ) ;
#16486 = CARTESIAN_POINT ( 'NONE',  ( 113.8163171295247764, 0.1403307496149613920, -13.39321520033831447 ) ) ;
#16487 = CARTESIAN_POINT ( 'NONE',  ( 109.2324108795247923, -8.938348069036489818, -9.318865927141430916 ) ) ;
#16488 = TOROIDAL_SURFACE ( 'NONE', #24484, 6.500000000000000000, 1.500000000000000000 ) ;
#16489 = CARTESIAN_POINT ( 'NONE',  ( 122.8936081442453059, 0.2603800115204892296, -16.42320221600525088 ) ) ;
#16490 = CARTESIAN_POINT ( 'NONE',  ( 123.0637881442452937, -8.899110576539710493, -16.42337572283490132 ) ) ;
#16491 = VERTEX_POINT ( 'NONE', #11772 ) ;
#16492 = CARTESIAN_POINT ( 'NONE',  ( 125.2194014775786286, -10.30919188438810075, -12.61870101168855918 ) ) ;
#16493 = CARTESIAN_POINT ( 'NONE',  ( 31.33087284928346605, -19.31933043625826585, -19.39321520033831447 ) ) ;
#16494 = CARTESIAN_POINT ( 'NONE',  ( 109.2294421295247844, -8.865838614420134434, -9.247624522711900497 ) ) ;
#16495 = CARTESIAN_POINT ( 'NONE',  ( 121.6456214775786293, -10.63000616557722466, -14.87417383870573495 ) ) ;
#16496 = CARTESIAN_POINT ( 'NONE',  ( 122.6667014775786413, -7.893985811506177619, -18.51759400769804742 ) ) ;
#16497 = CARTESIAN_POINT ( 'NONE',  ( 110.2184548109119788, -1.904930392188239452, -16.08466725871020842 ) ) ;
#16498 = CARTESIAN_POINT ( 'NONE',  ( 122.7801548109119665, -6.222761293078241884, -8.102969835052219238 ) ) ;
#16499 = CARTESIAN_POINT ( 'NONE',  ( 124.6894688159050872, -8.253847584685239269, -17.09290432062678278 ) ) ;
#16500 = CARTESIAN_POINT ( 'NONE',  ( 69.36136150295220659, -101.1685209014307674, -50.56525720990386219 ) ) ;
#16501 = ORIENTED_EDGE ( 'NONE', *, *, #24355, .T. ) ;
#16502 = DIRECTION ( 'NONE',  ( 1.000000000000000000, 0.000000000000000000, -0.000000000000000000 ) ) ;
#16503 = LINE ( 'NONE', #23335, #13609 ) ;
#16504 = CARTESIAN_POINT ( 'NONE',  ( 123.7445081442452874, -7.894159318335828068, -9.358103419637847864 ) ) ;
#16505 = AXIS2_PLACEMENT_3D ( 'NONE', #24240, #34260, #44774 ) ;
#16506 = CARTESIAN_POINT ( 'NONE',  ( 107.6349890045248401, -9.868328341294098749, -11.32035403202665869 ) ) ;
#16507 = CARTESIAN_POINT ( 'NONE',  ( 110.1353015045248469, -6.936859964151250502, -18.39754474579286025 ) ) ;
#16508 = CARTESIAN_POINT ( 'NONE',  ( 118.4122014775786340, -9.859900752359374465, -12.68260735090039404 ) ) ;
#16509 = CARTESIAN_POINT ( 'NONE',  ( 70.84837298282427298, -25.38184484516613892, -5.473262044462615883 ) ) ;
#16510 = CARTESIAN_POINT ( 'NONE',  ( 117.4478481442453131, -9.565557343593413364, -10.61323700422348004 ) ) ;
#16511 = CARTESIAN_POINT ( 'NONE',  ( 122.2696148109119889, -4.089484607189486809, -7.948022111789456723 ) ) ;
#16512 = ORIENTED_EDGE ( 'NONE', *, *, #23236, .T. ) ;
#16513 = CONICAL_SURFACE ( 'NONE', #25218, 2.999999999999999556, 0.9599310885968830309 ) ;
#16514 = CARTESIAN_POINT ( 'NONE',  ( 123.7445081442452874, -7.894159318335828068, -9.358103419637847864 ) ) ;
#16515 = CARTESIAN_POINT ( 'NONE',  ( 118.8660148109119774, -10.30919188438810075, -12.61870101168855918 ) ) ;
#16516 = CARTESIAN_POINT ( 'NONE',  ( 124.1415948109119540, -6.344957434206665248, -7.627207830600338134 ) ) ;
#16517 = CARTESIAN_POINT ( 'NONE',  ( 124.9924948109119924, -5.574606645277164318, -18.38911715685844683 ) ) ;
#16518 = ORIENTED_EDGE ( 'NONE', *, *, #24251, .F. ) ;
#16519 = CARTESIAN_POINT ( 'NONE',  ( 123.3875309814547023, -2.395992375830759524, -17.92872468182853396 ) ) ;
#16520 = EDGE_CURVE ( 'NONE', #45059, #12393, #31473, .T. ) ;
#16521 = CIRCLE ( 'NONE', #19427, 2.000000000000000444 ) ;
#16522 = CARTESIAN_POINT ( 'NONE',  ( 125.3328548109119964, -9.261995988541697145, -16.69588392320189030 ) ) ;
#16523 = CARTESIAN_POINT ( 'NONE',  ( 114.9518748109119883, -7.643976991954077427, -18.09477374809248928 ) ) ;
#16524 = CARTESIAN_POINT ( 'NONE',  ( 111.9453614775786434, -7.894159318335828068, -9.358103419637847864 ) ) ;
#16525 = CARTESIAN_POINT ( 'NONE',  ( 108.3295202545248657, -10.62599879583958717, -15.77991374673208469 ) ) ;
#16526 = CARTESIAN_POINT ( 'NONE',  ( 122.6604860609119640, -3.387241619883791355, -18.17469012370385073 ) ) ;
#16527 = ORIENTED_EDGE ( 'NONE', *, *, #44843, .T. ) ;
#16528 = CARTESIAN_POINT ( 'NONE',  ( 70.19189222814998175, -55.76308905022629858, -35.50805039322867884 ) ) ;
#16529 = CARTESIAN_POINT ( 'NONE',  ( 107.8433483795247838, -8.402594152722688392, -16.93181055722141792 ) ) ;
#16530 = EDGE_CURVE ( 'NONE', #1359, #37342, #28680, .T. ) ;
#16531 = AXIS2_PLACEMENT_3D ( 'NONE', #17123, #26923, #38290 ) ;
#16532 = CARTESIAN_POINT ( 'NONE',  ( 94.20708369096698220, -25.99489077589524300, -13.39321520033831447 ) ) ;
#16533 = CARTESIAN_POINT ( 'NONE',  ( 118.9227414775786542, 0.4262465694468514643, -12.03445270309931736 ) ) ;
#16534 = CARTESIAN_POINT ( 'NONE',  ( 112.3991748109119868, -1.833838273342658809, -17.42832698103878286 ) ) ;
#16535 = CARTESIAN_POINT ( 'NONE',  ( 125.3895814775786448, -2.084020599724410339, -8.691656652584146769 ) ) ;
#16536 = ORIENTED_EDGE ( 'NONE', *, *, #21018, .F. ) ;
#16537 = CARTESIAN_POINT ( 'NONE',  ( 121.9470836909669913, -25.99489077589524300, -13.39321520033831447 ) ) ;
#16538 = CARTESIAN_POINT ( 'NONE',  ( 120.5110881442453206, -3.505236298600246325, -18.68346056562440793 ) ) ;
#16539 = CARTESIAN_POINT ( 'NONE',  ( 113.9875214775786532, -8.899110576539710493, -16.42337572283490132 ) ) ;
#16540 = VECTOR ( 'NONE', #16436, 1000.000000000000114 ) ;
#16541 = CARTESIAN_POINT ( 'NONE',  ( 86.34560043013698305, -9.320000780048239619, -8.143215200338314474 ) ) ;
#16542 = CARTESIAN_POINT ( 'NONE',  ( 89.01247232317646763, -27.84333996136784961, -14.15691383771150136 ) ) ;
#16544 = CARTESIAN_POINT ( 'NONE',  ( 123.3474214775786209, -9.988377603198976828, -10.36322818467138340 ) ) ;
#16543 = CARTESIAN_POINT ( 'NONE',  ( 114.1453860982116737, 0.3867979994853637526, -12.14321520033831625 ) ) ;
#16545 = CARTESIAN_POINT ( 'NONE',  ( 113.0231681442453322, 0.9020085738987339008, -11.91225656197089222 ) ) ;
#16546 = EDGE_LOOP ( 'NONE', ( #20503, #19886, #23350, #36231 ) ) ;
#16547 = DIRECTION ( 'NONE',  ( 0.000000000000000000, 0.000000000000000000, 1.000000000000000000 ) ) ;
#16548 = CARTESIAN_POINT ( 'NONE',  ( 55.39394582045726168, -26.25884925591183716, -19.39321520033831447 ) ) ;
#16549 = CARTESIAN_POINT ( 'NONE',  ( 116.1777233795247781, -8.938348069036489818, -17.46756447353520159 ) ) ;
#16550 = CARTESIAN_POINT ( 'NONE',  ( 111.9453614775786434, -1.561330072975668060, -17.79121239304076596 ) ) ;
#16551 = AXIS2_PLACEMENT_3D ( 'NONE', #15904, #26386, #29354 ) ;
#16552 = CARTESIAN_POINT ( 'NONE',  ( 120.0005481442453146, -4.153390946401325223, -8.397313243818185668 ) ) ;
#16553 = CYLINDRICAL_SURFACE ( 'NONE', #24972, 5.000000000000004441 ) ;
#16554 = CARTESIAN_POINT ( 'NONE',  ( 114.6497546295247929, -4.863998795839590272, -18.39754474579285315 ) ) ;
#16555 = CARTESIAN_POINT ( 'NONE',  ( 117.1074881442453233, -10.63000616557722111, -14.87417383870573850 ) ) ;
#16556 = DIRECTION ( 'NONE',  ( -0.7871354856660202071, 0.6167752151498580027, 0.002461946824133919541 ) ) ;
#16557 = CARTESIAN_POINT ( 'NONE',  ( 112.9097148109120070, -9.565557343593413364, -10.61323700422348004 ) ) ;
#16558 = CARTESIAN_POINT ( 'NONE',  ( 109.7185827545247889, -2.477300249445798297, -19.15521520033831138 ) ) ;
#16559 = CARTESIAN_POINT ( 'NONE',  ( 117.8449348109119938, -8.166667518702803719, -8.995218007635848778 ) ) ;
#16560 = CARTESIAN_POINT ( 'NONE',  ( 115.8304577545247582, -7.250697342233347165, -7.631215200338321125 ) ) ;
#16561 = CARTESIAN_POINT ( 'NONE',  ( 124.1415948109119540, -6.344957434206665248, -7.627207830600338134 ) ) ;
#16562 = CARTESIAN_POINT ( 'NONE',  ( 121.5321681442453183, -9.988377603198976828, -10.36322818467138340 ) ) ;
#16563 = CARTESIAN_POINT ( 'NONE',  ( 69.36136150295220659, -55.54473230423695185, -32.31590080742341797 ) ) ;
#16564 = CARTESIAN_POINT ( 'NONE',  ( 121.1918081442452859, 0.9020085738987339008, -11.91225656197089222 ) ) ;
#16565 = CARTESIAN_POINT ( 'NONE',  ( 112.1722681442453222, -0.4660016031367893996, -10.09054647747474043 ) ) ;
#16566 = ORIENTED_EDGE ( 'NONE', *, *, #28388, .F. ) ;
#16567 = CARTESIAN_POINT ( 'NONE',  ( 114.7249681442453237, -9.565557343593413364, -10.61323700422348004 ) ) ;
#16568 = CARTESIAN_POINT ( 'NONE',  ( 113.1366214775786432, -7.643976991954077427, -18.09477374809248928 ) ) ;
#16569 = CARTESIAN_POINT ( 'NONE',  ( 123.6877814775786533, -3.383040157471821630, -19.15922257007629170 ) ) ;
#16570 = CARTESIAN_POINT ( 'NONE',  ( 115.8595014775786609, -1.834011780172310813, -8.268836392978581529 ) ) ;
#16571 = AXIS2_PLACEMENT_3D ( 'NONE', #7354, #10350, #31524 ) ;
#16572 = CARTESIAN_POINT ( 'NONE',  ( 113.8740681442453138, -9.859900752359374465, -12.68260735090039404 ) ) ;
#16573 = ORIENTED_EDGE ( 'NONE', *, *, #42493, .F. ) ;
#16574 = CARTESIAN_POINT ( 'NONE',  ( 115.9729548109119861, -3.505236298600246325, -18.68346056562440793 ) ) ;
#16575 = CARTESIAN_POINT ( 'NONE',  ( 111.8319081442453182, -5.638512984488999180, -18.83840828888717311 ) ) ;
#16576 = CARTESIAN_POINT ( 'NONE',  ( 112.0105358795247810, -8.402594152722688392, -9.854619843455216355 ) ) ;
#16577 = CARTESIAN_POINT ( 'NONE',  ( 123.8012348109119642, -9.565557343593413364, -10.61323700422348004 ) ) ;
#16578 = CARTESIAN_POINT ( 'NONE',  ( 116.8560548885474901, -0.4970007677390160805, -16.32824759579170149 ) ) ;
#16579 = CARTESIAN_POINT ( 'NONE',  ( 112.1494421295248003, 0.8980012041604618078, -13.39321520033831447 ) ) ;
#16580 = ORIENTED_EDGE ( 'NONE', *, *, #28718, .F. ) ;
#16581 = CARTESIAN_POINT ( 'NONE',  ( 121.9659548109119811, -2.527210466738041728, -8.967976844669124148 ) ) ;
#16582 = CARTESIAN_POINT ( 'NONE',  ( 126.0703014775786102, -9.988377603198980381, -10.36322818467138518 ) ) ;
#16583 = LINE ( 'NONE', #26383, #20417 ) ;
#16584 = CARTESIAN_POINT ( 'NONE',  ( 109.2294421295247844, -11.83367149576868727, -7.393215200338315363 ) ) ;
#16585 = ADVANCED_FACE ( 'NONE', ( #22475 ), #34430, .T. ) ;
#16586 = CARTESIAN_POINT ( 'NONE',  ( 117.0895350763799456, 1.621925030527854528, -5.439520474528995564 ) ) ;
#16587 = CARTESIAN_POINT ( 'NONE',  ( 113.9533551332721828, 0.2334052082820642360, -14.64321520033831447 ) ) ;
#16588 =( BOUNDED_CURVE ( )  B_SPLINE_CURVE ( 2, ( #10219, #2681, #23452, #40779, #16612 ),
 .UNSPECIFIED., .F., .T. ) 
 B_SPLINE_CURVE_WITH_KNOTS ( ( 3, 2, 3 ),
 ( 0.8125000000000000000, 0.8203125000000000000, 0.8266217583431409999 ),
 .UNSPECIFIED. ) 
 CURVE ( )  GEOMETRIC_REPRESENTATION_ITEM ( )  RATIONAL_B_SPLINE_CURVE ( ( 1.000000000000000000, 0.9238795325112859613, 1.000000000000000000, 0.9385262470928680267, 0.9763430640195970289 ) ) 
 REPRESENTATION_ITEM ( '' )  );
#16589 = CARTESIAN_POINT ( 'NONE',  ( 107.5655358795247736, -8.402594152722688392, -9.854619843455216355 ) ) ;
#16590 = DIRECTION ( 'NONE',  ( 0.000000000000000000, 0.3818493186865927203, -0.9242245927363029745 ) ) ;
#16591 = CARTESIAN_POINT ( 'NONE',  ( 116.5402214775786405, 0.2603800115204892296, -16.42320221600525088 ) ) ;
#16592 = CARTESIAN_POINT ( 'NONE',  ( 135.8991650439206467, -4.137162889731972548, -19.29038791749874804 ) ) ;
#16593 = CARTESIAN_POINT ( 'NONE',  ( 63.74703025577719018, -40.95155355269160680, -10.89321520033831447 ) ) ;
#16595 = CARTESIAN_POINT ( 'NONE',  ( 124.4694423109119725, -9.285408612553634811, -11.05844856689041755 ) ) ;
#16594 = VECTOR ( 'NONE', #24042, 1000.000000000000000 ) ;
#16596 = CARTESIAN_POINT ( 'NONE',  ( 119.8870948109119752, -0.8288870151387760510, -10.36305467784173118 ) ) ;
#16597 = CARTESIAN_POINT ( 'NONE',  ( 119.7434548109119703, 0.4041035117704004365, -14.01369669089266168 ) ) ;
#16598 = EDGE_LOOP ( 'NONE', ( #6398, #13352, #13874, #11435, #30586 ) ) ;
#16599 = CARTESIAN_POINT ( 'NONE',  ( 123.5743281442453139, -7.893985811506177619, -18.51759400769804742 ) ) ;
#16600 = CARTESIAN_POINT ( 'NONE',  ( 120.0572748109119772, -3.383040157471821630, -19.15922257007629170 ) ) ;
#16601 = CARTESIAN_POINT ( 'NONE',  ( 125.9001214775786224, -4.089484607189486809, -7.948022111789456723 ) ) ;
#16602 = CARTESIAN_POINT ( 'NONE',  ( 112.3991748109119868, -1.833838273342658809, -17.42832698103878286 ) ) ;
#16603 = CARTESIAN_POINT ( 'NONE',  ( 122.8368814775786291, -1.561330072975668948, -17.79121239304076951 ) ) ;
#16604 = CARTESIAN_POINT ( 'NONE',  ( 110.2047546295247855, -4.863998795839590272, -7.631215200338315796 ) ) ;
#16605 = CARTESIAN_POINT ( 'NONE',  ( 104.9263171295248327, 0.1403307496149613920, -13.39321520033831447 ) ) ;
#16606 = CARTESIAN_POINT ( 'NONE',  ( 115.8304577545247582, -7.250697342233347165, -7.631215200338321125 ) ) ;
#16607 = CARTESIAN_POINT ( 'NONE',  ( 115.3489614775786407, -0.8288870151387760510, -10.36305467784173118 ) ) ;
#16608 = CARTESIAN_POINT ( 'NONE',  ( 117.8449348109119938, -1.833838273342659253, -17.42832698103878286 ) ) ;
#16609 = FACE_OUTER_BOUND ( 'NONE', #31325, .T. ) ;
#16610 = CARTESIAN_POINT ( 'NONE',  ( 113.8163171295247764, 0.1403307496149613920, -13.39321520033831447 ) ) ;
#16611 = ORIENTED_EDGE ( 'NONE', *, *, #20682, .F. ) ;
#16612 = CARTESIAN_POINT ( 'NONE',  ( 124.1773369107181821, -2.467220198592779301, -17.83387418641524391 ) ) ;
#16613 = CARTESIAN_POINT ( 'NONE',  ( 113.8740681442453138, 0.5811942927096154232, -14.16772938898807155 ) ) ;
#16614 = DIRECTION ( 'NONE',  ( 1.000000000000000000, 0.000000000000000000, -0.000000000000000000 ) ) ;
#16615 = CARTESIAN_POINT ( 'NONE',  ( 121.2019704359119743, -10.25716656981731489, -12.88942061488890545 ) ) ;
#16616 = CARTESIAN_POINT ( 'NONE',  ( 122.1743141859119817, -8.321307733199551748, -9.223433127585318303 ) ) ;
#16617 = ORIENTED_EDGE ( 'NONE', *, *, #17538, .F. ) ;
#16618 = DIRECTION ( 'NONE',  ( -0.2768435750659266059, -0.3568721902840680249, 0.8921882507333128709 ) ) ;
#16619 = CARTESIAN_POINT ( 'NONE',  ( 104.9263171295248327, 0.1403307496149613920, -13.39321520033831447 ) ) ;
#16620 = VERTEX_POINT ( 'NONE', #1718 ) ;
#16621 = CARTESIAN_POINT ( 'NONE',  ( 118.9227414775786400, -10.63000616557722466, -14.87417383870573495 ) ) ;
#16622 = CARTESIAN_POINT ( 'NONE',  ( 124.3117748109119844, 0.1319031606808879209, -14.10382304977623669 ) ) ;
#16623 = CARTESIAN_POINT ( 'NONE',  ( 119.6034614775786196, -3.505236298600246325, -18.68346056562440793 ) ) ;
#16624 = DIRECTION ( 'NONE',  ( -0.000000000000000000, -0.9284778069183721172, -0.3713878862591650232 ) ) ;
#16625 = CARTESIAN_POINT ( 'NONE',  ( 123.0070614775786169, 0.9020085738987339008, -11.91225656197089222 ) ) ;
#16626 = CARTESIAN_POINT ( 'NONE',  ( 119.7169148109119874, -9.988377603198976828, -10.36322818467138340 ) ) ;
#16627 = CARTESIAN_POINT ( 'NONE',  ( 109.8574890045247940, -9.868328341294098749, -11.32035403202665869 ) ) ;
#16628 = VECTOR ( 'NONE', #38730, 1000.000000000000114 ) ;
#16629 = CARTESIAN_POINT ( 'NONE',  ( 112.9097148109120070, -9.565557343593413364, -10.61323700422348004 ) ) ;
#16630 = LINE ( 'NONE', #19816, #9747 ) ;
#16631 = EDGE_LOOP ( 'NONE', ( #9317, #37647, #37655, #1066, #19423 ) ) ;
#16632 = CARTESIAN_POINT ( 'NONE',  ( 116.9940348109119839, -9.988377603198976828, -10.36322818467138340 ) ) ;
#16633 = CARTESIAN_POINT ( 'NONE',  ( 114.4980614775786734, -2.084020599724406786, -8.691656652584148546 ) ) ;
#16634 = CARTESIAN_POINT ( 'NONE',  ( 78.69189222814998175, -63.77884951796256274, -31.62409037935697143 ) ) ;
#16635 = CARTESIAN_POINT ( 'NONE',  ( 125.8433948109119456, -7.643976991954077427, -18.09477374809248928 ) ) ;
#16636 = ORIENTED_EDGE ( 'NONE', *, *, #39615, .F. ) ;
#16637 = CARTESIAN_POINT ( 'NONE',  ( 121.0783548109119749, 0.2603800115204892296, -16.42320221600525088 ) ) ;
#16638 = LINE ( 'NONE', #30308, #21609 ) ;
#16639 = FACE_OUTER_BOUND ( 'NONE', #19246, .T. ) ;
#16640 = CARTESIAN_POINT ( 'NONE',  ( 125.0483885810856890, -1.220279397241718966, -16.99638242193886484 ) ) ;
#16641 = CARTESIAN_POINT ( 'NONE',  ( 90.45092582798827152, -25.99489077589524300, -13.39321520033831625 ) ) ;
#16642 = CARTESIAN_POINT ( 'NONE',  ( 114.4980614775786734, -2.084020599724406786, -8.691656652584148546 ) ) ;
#16643 = CARTESIAN_POINT ( 'NONE',  ( 136.2632467228237374, -2.605123477878678706, -8.005467003093405864 ) ) ;
#16644 = CARTESIAN_POINT ( 'NONE',  ( 118.4689281442453250, -10.15424416112533912, -14.75197769757731336 ) ) ;
#16645 = PLANE ( 'NONE',  #26687 ) ;
#16646 = CARTESIAN_POINT ( 'NONE',  ( 115.0653281442453277, -3.505236298600246325, -18.68346056562440793 ) ) ;
#16647 = CARTESIAN_POINT ( 'NONE',  ( 117.3911214775786505, -1.561330072975668504, -17.79121239304076951 ) ) ;
#16648 = CARTESIAN_POINT ( 'NONE',  ( 120.3685329359119862, -4.283928203966213211, -7.183505701512925334 ) ) ;
#16649 = CARTESIAN_POINT ( 'NONE',  ( 112.0020881442453344, 0.2603800115204892296, -16.42320221600525088 ) ) ;
#16650 = CARTESIAN_POINT ( 'NONE',  ( 114.7816948109119863, -9.859900752359374465, -12.68260735090039404 ) ) ;
#16651 = CARTESIAN_POINT ( 'NONE',  ( 123.9146881442452894, 0.9020085738987339008, -11.91225656197089222 ) ) ;
#16652 = CARTESIAN_POINT ( 'NONE',  ( 115.4624148109119943, -4.153390946401321671, -8.397313243818183892 ) ) ;
#16653 = VERTEX_POINT ( 'NONE', #37737 ) ;
#16654 = CARTESIAN_POINT ( 'NONE',  ( 112.7395348109119766, -5.638512984488999180, -18.83840828888717311 ) ) ;
#16655 = EDGE_CURVE ( 'NONE', #25324, #13081, #2620, .T. ) ;
#16656 = CARTESIAN_POINT ( 'NONE',  ( 113.8163171295247764, -10.62599879583958540, -13.39321520033831447 ) ) ;
#16657 = FACE_OUTER_BOUND ( 'NONE', #29018, .T. ) ;
#16658 = CARTESIAN_POINT ( 'NONE',  ( 62.02687168119881278, -37.86334235074598098, -5.893215200338315363 ) ) ;
#16659 = DIRECTION ( 'NONE',  ( 0.6049664196031393493, -0.7962509850245451659, 0.000000000000000000 ) ) ;
#16660 = CARTESIAN_POINT ( 'NONE',  ( 120.5678148109119832, -8.166667518702819706, -8.995218007635861213 ) ) ;
#16661 = ORIENTED_EDGE ( 'NONE', *, *, #8588, .T. ) ;
#16662 = CARTESIAN_POINT ( 'NONE',  ( 125.7866681442452688, -0.4660016031367893996, -10.09054647747474043 ) ) ;
#16663 = CARTESIAN_POINT ( 'NONE',  ( 94.20708369096698220, -24.88943055980569241, -13.49371108670732333 ) ) ;
#16664 = CARTESIAN_POINT ( 'NONE',  ( 115.1220548109119761, -1.833838273342658809, -17.42832698103878286 ) ) ;
#16665 = CARTESIAN_POINT ( 'NONE',  ( 124.4252281442452812, -0.8288870151387603968, -10.36305467784175072 ) ) ;
#16666 = CARTESIAN_POINT ( 'NONE',  ( 124.7655881442452852, 0.5811942927096110934, -14.16772938898807510 ) ) ;
#16667 = CARTESIAN_POINT ( 'NONE',  ( 105.7597546295248350, -4.863998795839590272, -7.631215200338315796 ) ) ;
#16668 = CARTESIAN_POINT ( 'NONE',  ( 124.2928311593281876, -8.517053830703071426, -17.59134500557229330 ) ) ;
#16669 = ORIENTED_EDGE ( 'NONE', *, *, #40084, .T. ) ;
#16670 = CARTESIAN_POINT ( 'NONE',  ( 112.3991748109119868, -8.166667518702817929, -8.995218007635859436 ) ) ;
#16671 = CARTESIAN_POINT ( 'NONE',  ( 122.3263414775786373, -3.505236298600246325, -18.68346056562440793 ) ) ;
#16672 = CARTESIAN_POINT ( 'NONE',  ( 119.7169148109119874, -9.988377603198976828, -10.36322818467138340 ) ) ;
#16673 = CARTESIAN_POINT ( 'NONE',  ( 114.0442481442453300, -7.643976991954077427, -18.09477374809248928 ) ) ;
#16674 =( BOUNDED_CURVE ( )  B_SPLINE_CURVE ( 2, ( #9676, #6710, #21051, #16979, #27236, #20397, #34928, #44792, #13550, #20619, #34496, #42775, #11757, #18595, #4227, #11307, #8335 ),
 .UNSPECIFIED., .F., .T. ) 
 B_SPLINE_CURVE_WITH_KNOTS ( ( 3, 2, 2, 2, 2, 2, 2, 2, 3 ),
 ( 0.2045046674808919940, 0.2109375000000000000, 0.2187500000000000000, 0.2265625000000000000, 0.2343750000000000000, 0.2421875000000000000, 0.2500000000000000000, 0.2578125000000000000, 0.2642453325190585178 ),
 .UNSPECIFIED. ) 
 CURVE ( )  GEOMETRIC_REPRESENTATION_ITEM ( )  RATIONAL_B_SPLINE_CURVE ( ( 0.9778625265006459788, 0.9373222120152210346, 1.000000000000000000, 0.9238795325112869605, 1.000000000000000000, 0.9238795325112869605, 1.000000000000000000, 0.9238795325112869605, 1.000000000000000000, 0.9238795325112869605, 1.000000000000000000, 0.9238795325112869605, 1.000000000000000000, 0.9238795325112869605, 1.000000000000000000, 0.9373222120157009840, 0.9778625265000250311 ) ) 
 REPRESENTATION_ITEM ( '' )  );
#16675 = CARTESIAN_POINT ( 'NONE',  ( 114.9518748109119883, -1.834011780172310813, -8.268836392978581529 ) ) ;
#16676 = ADVANCED_FACE ( 'NONE', ( #41626 ), #16553, .F. ) ;
#16677 = DIRECTION ( 'NONE',  ( 0.000000000000000000, -0.3818493186865936084, 0.9242245927363024194 ) ) ;
#16678 = CARTESIAN_POINT ( 'NONE',  ( 127.7617783745703974, -1.248496758771796999, -8.893780266587674177 ) ) ;
#16679 = CARTESIAN_POINT ( 'NONE',  ( 120.0005481442453146, -4.153390946401325223, -8.397313243818185668 ) ) ;
#16680 = ORIENTED_EDGE ( 'NONE', *, *, #4956, .T. ) ;
#16681 = EDGE_CURVE ( 'NONE', #6720, #26554, #13338, .T. ) ;
#16682 = EDGE_CURVE ( 'NONE', #9245, #39715, #11861, .T. ) ;
#16683 = CARTESIAN_POINT ( 'NONE',  ( 123.0772048109119652, -7.554583864224885481, -18.48844787311982785 ) ) ;
#16684 = CARTESIAN_POINT ( 'NONE',  ( 112.4559014775786494, -9.988377603198976828, -10.36322818467138340 ) ) ;
#16685 = CARTESIAN_POINT ( 'NONE',  ( 123.0070614775786169, -10.15424416112533912, -14.75197769757731336 ) ) ;
#16686 = ORIENTED_EDGE ( 'NONE', *, *, #14309, .T. ) ;
#16687 = CARTESIAN_POINT ( 'NONE',  ( 121.5492360609119800, -3.387241619883791355, -18.17469012370385073 ) ) ;
#16688 = CARTESIAN_POINT ( 'NONE',  ( 136.5847729262691246, -1.254589541683206688, -8.968780776681423816 ) ) ;
#16689 = ADVANCED_BREP_SHAPE_REPRESENTATION ( '', ( #6206, #12375 ), #32596 ) ;
#16690 = CARTESIAN_POINT ( 'NONE',  ( 118.0151148109119816, -10.63000616557722466, -14.87417383870573495 ) ) ;
#16691 = CARTESIAN_POINT ( 'NONE',  ( 110.5520202545248054, -10.62599879583958717, -15.77991374673208469 ) ) ;
#16692 = CARTESIAN_POINT ( 'NONE',  ( 117.9583881442453048, 0.1319031606808879209, -14.10382304977623669 ) ) ;
#16693 = ORIENTED_EDGE ( 'NONE', *, *, #14485, .F. ) ;
#16694 = ORIENTED_EDGE ( 'NONE', *, *, #30585, .F. ) ;
#16695 = CARTESIAN_POINT ( 'NONE',  ( 126.1837548109119496, 0.4262465694468514643, -12.03445270309931736 ) ) ;
#16696 = CONICAL_SURFACE ( 'NONE', #21066, 2.445500000000004448, 0.9599310885968757034 ) ;
#16697 = CARTESIAN_POINT ( 'NONE',  ( 124.9924948109119924, -5.574606645277164318, -18.38911715685844683 ) ) ;
#16698 = DIRECTION ( 'NONE',  ( -0.07634843047859724008, -0.9970811988817435134, 0.000000000000000000 ) ) ;
#16699 = LINE ( 'NONE', #9860, #41816 ) ;
#16700 = CARTESIAN_POINT ( 'NONE',  ( 122.2128881442453263, -1.834011780172310813, -8.268836392978581529 ) ) ;
#16701 = EDGE_CURVE ( 'NONE', #15443, #24220, #20647, .T. ) ;
#16702 = CYLINDRICAL_SURFACE ( 'NONE', #34265, 1.999999999999998890 ) ;
#16703 = CARTESIAN_POINT ( 'NONE',  ( 143.3676850761856940, -82.08636712479707853, -32.64558696907351987 ) ) ;
#16704 = CARTESIAN_POINT ( 'NONE',  ( 120.5110881442453206, -6.344957434206665248, -7.627207830600338134 ) ) ;
#16706 = CARTESIAN_POINT ( 'NONE',  ( 120.3976348109119812, -7.643976991954077427, -18.09477374809248928 ) ) ;
#16705 = CARTESIAN_POINT ( 'NONE',  ( 119.5467348109119712, -4.089484607189486809, -7.948022111789456723 ) ) ;
#16707 = CARTESIAN_POINT ( 'NONE',  ( 125.7866681442452688, -8.899110576539710493, -16.42337572283490132 ) ) ;
#16708 = CARTESIAN_POINT ( 'NONE',  ( 112.2289948109119848, -1.834011780172310813, -8.268836392978581529 ) ) ;
#16709 = EDGE_CURVE ( 'NONE', #3183, #33968, #35853, .T. ) ;
#16710 = ORIENTED_EDGE ( 'NONE', *, *, #1152, .F. ) ;
#16711 = CARTESIAN_POINT ( 'NONE',  ( 123.9146881442452894, -10.15424416112533912, -14.75197769757731336 ) ) ;
#16712 = CARTESIAN_POINT ( 'NONE',  ( 122.2862319737025416, -1.196538596002817867, -17.02799684832028504 ) ) ;
#16713 = ADVANCED_FACE ( 'NONE', ( #9475 ), #16782, .T. ) ;
#16714 = CYLINDRICAL_SURFACE ( 'NONE', #25659, 1.500000000000001332 ) ;
#16715 = CARTESIAN_POINT ( 'NONE',  ( 108.6073327545248048, -2.477300249445798297, -19.15521520033831138 ) ) ;
#16716 = CARTESIAN_POINT ( 'NONE',  ( 113.2606921295247702, -9.868328341294093420, -13.39321520033831447 ) ) ;
#16717 = CARTESIAN_POINT ( 'NONE',  ( 107.3571765045248299, -7.250697342233347165, -19.15521520033831138 ) ) ;
#16718 = CARTESIAN_POINT ( 'NONE',  ( 122.0994348109119443, 0.9020085738987339008, -11.91225656197089222 ) ) ;
#16719 = CARTESIAN_POINT ( 'NONE',  ( 121.6456214775786293, 0.4262465694468514643, -12.03445270309931736 ) ) ;
#16720 = EDGE_LOOP ( 'NONE', ( #34362, #35711, #6677, #14637 ) ) ;
#16721 = CARTESIAN_POINT ( 'NONE',  ( 125.5597614775786326, -1.561330072975669392, -17.79121239304076951 ) ) ;
#16722 = DIRECTION ( 'NONE',  ( 0.9609149988134837450, -0.1028163501681639419, 0.2570431154366518145 ) ) ;
#16723 = CARTESIAN_POINT ( 'NONE',  ( 121.7590748109119687, -2.084020599724363265, -8.691656652584173415 ) ) ;
#16724 = CARTESIAN_POINT ( 'NONE',  ( 119.6034614775786196, -6.344957434206665248, -7.627207830600338134 ) ) ;
#16725 = CARTESIAN_POINT ( 'NONE',  ( 122.7801548109119665, -3.383040157471821630, -19.15922257007629170 ) ) ;
#16726 = CARTESIAN_POINT ( 'NONE',  ( 125.4584548109119737, -9.722663502801697888, -19.87444018218530317 ) ) ;
#16727 = CARTESIAN_POINT ( 'NONE',  ( 112.3424481442453384, -6.344957434206662583, -7.627207830600332805 ) ) ;
#16728 = CARTESIAN_POINT ( 'NONE',  ( 116.5944421295247793, -4.863998795839590272, -13.39321520033831447 ) ) ;
#16729 = ORIENTED_EDGE ( 'NONE', *, *, #13075, .T. ) ;
#16730 = DIRECTION ( 'NONE',  ( 1.000000000000000000, 0.000000000000000000, -0.000000000000000000 ) ) ;
#16731 = CARTESIAN_POINT ( 'NONE',  ( 112.9097148109120070, -9.565557343593413364, -10.61323700422348004 ) ) ;
#16732 = CARTESIAN_POINT ( 'NONE',  ( 124.9924948109119924, -5.574606645277164318, -18.38911715685844683 ) ) ;
#16733 = AXIS2_PLACEMENT_3D ( 'NONE', #34236, #13283, #3010 ) ;
#16734 = CARTESIAN_POINT ( 'NONE',  ( 108.9545983795247821, -8.402594152722688392, -16.93181055722141792 ) ) ;
#16735 = CARTESIAN_POINT ( 'NONE',  ( 109.7185827545247889, -6.936859964151250502, -8.388885654883777576 ) ) ;
#16737 = AXIS2_PLACEMENT_3D ( 'NONE', #42279, #14015, #38172 ) ;
#16736 = CARTESIAN_POINT ( 'NONE',  ( 117.9583881442453048, 0.1319031606808879209, -14.10382304977623669 ) ) ;
#16738 = CARTESIAN_POINT ( 'NONE',  ( 0.000000000000000000, 0.000000000000000000, 0.000000000000000000 ) ) ;
#16739 = CARTESIAN_POINT ( 'NONE',  ( 114.4413348109119823, -0.8288870151387760510, -10.36305467784173118 ) ) ;
#16740 = CARTESIAN_POINT ( 'NONE',  ( 124.0281414775786146, -1.834011780172310813, -8.268836392978581529 ) ) ;
#16741 = VERTEX_POINT ( 'NONE', #23851 ) ;
#16742 = ADVANCED_FACE ( 'NONE', ( #40716 ), #16231, .T. ) ;
#16743 = CARTESIAN_POINT ( 'NONE',  ( 121.1918081442452859, -10.15424416112533912, -14.75197769757731336 ) ) ;
#16744 = CARTESIAN_POINT ( 'NONE',  ( 117.3911214775786505, -1.561330072975668504, -17.79121239304076951 ) ) ;
#16745 = CARTESIAN_POINT ( 'NONE',  ( 125.5597614775786326, -1.561330072975669392, -17.79121239304076951 ) ) ;
#16746 = CARTESIAN_POINT ( 'NONE',  ( 125.2194014775786286, 0.1319031606808879209, -14.10382304977623669 ) ) ;
#16747 = ORIENTED_EDGE ( 'NONE', *, *, #13998, .F. ) ;
#16748 = CARTESIAN_POINT ( 'NONE',  ( 76.69189222814998175, -49.76310523276720232, -19.39321520033831447 ) ) ;
#16749 = CARTESIAN_POINT ( 'NONE',  ( 122.3830681442452857, -8.166667518702819706, -8.995218007635861213 ) ) ;
#16750 = CARTESIAN_POINT ( 'NONE',  ( 116.4834948109119779, -7.894159318335828068, -9.358103419637847864 ) ) ;
#16751 = CARTESIAN_POINT ( 'NONE',  ( 125.4463081442452932, -5.638512984488999180, -18.83840828888717311 ) ) ;
#16752 = CARTESIAN_POINT ( 'NONE',  ( 117.6791703192116927, -2.378957183258571639, -17.95140958770219086 ) ) ;
#16753 = CARTESIAN_POINT ( 'NONE',  ( 124.1190016859119680, -0.6942167230862511529, -9.935906262978006609 ) ) ;
#16754 = ORIENTED_EDGE ( 'NONE', *, *, #22270, .F. ) ;
#16755 = DIRECTION ( 'NONE',  ( 0.9609149988134837450, -0.1028163501681639419, 0.2570431154366518145 ) ) ;
#16756 = CARTESIAN_POINT ( 'NONE',  ( 62.70662433455723317, -3.428858449946674103, -7.602483789130480396 ) ) ;
#16757 = CARTESIAN_POINT ( 'NONE',  ( 107.9128015045248219, -6.936859964151250502, -18.39754474579286025 ) ) ;
#16758 = VECTOR ( 'NONE', #39183, 1000.000000000000227 ) ;
#16759 = DIRECTION ( 'NONE',  ( -0.000000000000000000, -0.9284778069183721172, -0.3713878862591650232 ) ) ;
#16760 = CARTESIAN_POINT ( 'NONE',  ( 123.6310548109119765, -4.153390946401325223, -8.397313243818185668 ) ) ;
#16761 = CARTESIAN_POINT ( 'NONE',  ( 114.1009748109119784, -5.574606645277164318, -18.38911715685844683 ) ) ;
#16762 = CARTESIAN_POINT ( 'NONE',  ( 126.5621572003788344, -0.3458538473703972604, -10.87540104374022576 ) ) ;
#16763 = ORIENTED_EDGE ( 'NONE', *, *, #15178, .F. ) ;
#16764 = CARTESIAN_POINT ( 'NONE',  ( 92.26512299712632625, -23.76310523276723785, -4.893215200338314474 ) ) ;
#16765 = CARTESIAN_POINT ( 'NONE',  ( 119.2063748109119814, -7.894159318335828068, -9.358103419637847864 ) ) ;
#16766 = CARTESIAN_POINT ( 'NONE',  ( 114.2144281442453178, -1.833838273342658809, -17.42832698103878286 ) ) ;
#16767 = AXIS2_PLACEMENT_3D ( 'NONE', #38234, #23909, #16842 ) ;
#16768 = LINE ( 'NONE', #24058, #24271 ) ;
#16769 = CARTESIAN_POINT ( 'NONE',  ( 111.7289948109120132, -2.109465145232937378, -8.734689011829464889 ) ) ;
#16771 = CARTESIAN_POINT ( 'NONE',  ( 124.7655881442452852, 0.5811942927096110934, -14.16772938898807510 ) ) ;
#16770 = CARTESIAN_POINT ( 'NONE',  ( 70.60074220370958642, -26.44921982560606466, -5.510037297638909592 ) ) ;
#16772 = CARTESIAN_POINT ( 'NONE',  ( 112.6828081442453282, -7.893985811506177619, -18.51759400769804742 ) ) ;
#16773 = ORIENTED_EDGE ( 'NONE', *, *, #35878, .T. ) ;
#16774 = AXIS2_PLACEMENT_3D ( 'NONE', #43493, #14774, #39161 ) ;
#16775 = CARTESIAN_POINT ( 'NONE',  ( 113.9307948109119906, 0.9020085738987339008, -11.91225656197089222 ) ) ;
#16776 = DIRECTION ( 'NONE',  ( 0.2588190451025180749, -0.9659258262890690894, 0.000000000000000000 ) ) ;
#16777 = CARTESIAN_POINT ( 'NONE',  ( 106.4542858795248179, -8.402594152722688392, -9.854619843455216355 ) ) ;
#16778 = B_SPLINE_CURVE_WITH_KNOTS ( 'NONE', 3,
 ( #2290, #36271, #15764, #43578, #12348, #39931, #26701, #9370, #37161, #26025 ),
 .UNSPECIFIED., .F., .F.,
 ( 4, 3, 3, 4 ),
 ( 0.000000000000000000, 0.0002476486447138875262, 0.0004952972925464190672, 0.0009604418836934809417 ),
 .UNSPECIFIED. ) ;
#16779 = EDGE_CURVE ( 'NONE', #17122, #33790, #3522, .T. ) ;
#16780 = CARTESIAN_POINT ( 'NONE',  ( 124.7655881442452852, -9.859900752359378018, -12.68260735090039759 ) ) ;
#16781 = CARTESIAN_POINT ( 'NONE',  ( 122.4397948109119767, -0.1624402480850797581, -16.17319339645315424 ) ) ;
#16782 = CYLINDRICAL_SURFACE ( 'NONE', #38796, 3.000000000000001776 ) ;
#16783 = CARTESIAN_POINT ( 'NONE',  ( 114.7192077545248594, -2.791137627527939813, -18.39754474579286025 ) ) ;
#16784 = DIRECTION ( 'NONE',  ( 0.000000000000000000, 0.6004852223388321697, -0.7996358532186279566 ) ) ;
#16785 = CARTESIAN_POINT ( 'NONE',  ( 113.2384448136183721, -3.929494816604734098, -18.62311481910882804 ) ) ;
#16786 = DIRECTION ( 'NONE',  ( 0.000000000000000000, 0.000000000000000000, -1.000000000000000000 ) ) ;
#16787 = CARTESIAN_POINT ( 'NONE',  ( 117.6747548109119776, -1.834011780172314143, -8.268836392978577976 ) ) ;
#16788 = CARTESIAN_POINT ( 'NONE',  ( 114.9970202545248412, -10.62599879583958717, -15.77991374673208469 ) ) ;
#16789 = CARTESIAN_POINT ( 'NONE',  ( 123.0070614775786169, 0.9020085738987339008, -11.91225656197089222 ) ) ;
#16790 = CARTESIAN_POINT ( 'NONE',  ( 123.5743281442453139, -7.893985811506177619, -18.51759400769804742 ) ) ;
#16791 = CARTESIAN_POINT ( 'NONE',  ( 151.2860562277021472, -3.410847707154505137, -16.57729307524250828 ) ) ;
#16792 = CARTESIAN_POINT ( 'NONE',  ( 119.3198281442452924, 0.5811942927096110934, -14.16772938898807510 ) ) ;
#16793 = FACE_OUTER_BOUND ( 'NONE', #16546, .T. ) ;
#16794 = ORIENTED_EDGE ( 'NONE', *, *, #20447, .T. ) ;
#16795 = CARTESIAN_POINT ( 'NONE',  ( 114.8384214775786489, -10.15424416112533912, -14.75197769757731336 ) ) ;
#16796 = CARTESIAN_POINT ( 'NONE',  ( 125.3895814775786448, -7.893985811506177619, -18.51759400769804742 ) ) ;
#16797 = CARTESIAN_POINT ( 'NONE',  ( 122.0994348109119443, 0.9020085738987339008, -11.91225656197089222 ) ) ;
#16798 = AXIS2_PLACEMENT_3D ( 'NONE', #16728, #6461, #13080 ) ;
#16799 = CARTESIAN_POINT ( 'NONE',  ( 114.3278814775786429, -10.30919188438810075, -12.61870101168855918 ) ) ;
#16800 = CARTESIAN_POINT ( 'NONE',  ( 111.3780948109119890, -5.574606645277164318, -18.38911715685844683 ) ) ;
#16801 = VERTEX_POINT ( 'NONE', #27264 ) ;
#16802 = EDGE_CURVE ( 'NONE', #7584, #2526, #1653, .T. ) ;
#16803 = CARTESIAN_POINT ( 'NONE',  ( 116.3700414775786527, -4.153390946401321671, -8.397313243818183892 ) ) ;
#16804 = CARTESIAN_POINT ( 'NONE',  ( 113.0231681442453322, 0.9020085738987339008, -11.91225656197089222 ) ) ;
#16805 = CIRCLE ( 'NONE', #27734, 2.999999999999999556 ) ;
#16806 = CARTESIAN_POINT ( 'NONE',  ( 110.7603796295247918, -4.863998795839590272, -8.388885654883775800 ) ) ;
#16807 = CARTESIAN_POINT ( 'NONE',  ( 122.3263414775786373, -3.505236298600246325, -18.68346056562440793 ) ) ;
#16808 = CARTESIAN_POINT ( 'NONE',  ( 70.19189222814998175, -64.81574766768041229, -39.12908228425553858 ) ) ;
#16809 = CARTESIAN_POINT ( 'NONE',  ( 111.8716296295247901, -4.863998795839590272, -19.15521520033831493 ) ) ;
#16810 = ORIENTED_EDGE ( 'NONE', *, *, #17527, .F. ) ;
#16811 = TOROIDAL_SURFACE ( 'NONE', #44462, 3.250000000000000000, 0.2500000000000000000 ) ;
#16812 = CARTESIAN_POINT ( 'NONE',  ( 61.98298312043991132, -3.705371713990854854, -7.393215200338315363 ) ) ;
#16813 = CARTESIAN_POINT ( 'NONE',  ( 111.2184548109119788, -2.495269033102075262, -17.79652296963211455 ) ) ;
#16814 = CARTESIAN_POINT ( 'NONE',  ( 31.16856251326852956, -20.50830283073288385, -8.593215200338315540 ) ) ;
#16815 = CARTESIAN_POINT ( 'NONE',  ( 112.0020881442453344, 0.2603800115204892296, -16.42320221600525088 ) ) ;
#16816 = CARTESIAN_POINT ( 'NONE',  ( 122.0046199480702569, -6.365377317481695663, -18.95617363400926081 ) ) ;
#16817 = CARTESIAN_POINT ( 'NONE',  ( 61.69189222814998175, -55.76310523276723785, -34.89321520033831092 ) ) ;
#16818 = CARTESIAN_POINT ( 'NONE',  ( 107.0099108795247815, -1.325403438956436419, -16.93181055722141792 ) ) ;
#16819 = CARTESIAN_POINT ( 'NONE',  ( 115.1430393777725385, -1.267766418764730840, -16.93314635290706605 ) ) ;
#16820 = CARTESIAN_POINT ( 'NONE',  ( 118.4122014775786340, 0.5811942927096110934, -14.16772938898807510 ) ) ;
#16821 = CARTESIAN_POINT ( 'NONE',  ( 136.6694018951665157, -6.970064029879566192, -18.66362485201299748 ) ) ;
#16822 = CIRCLE ( 'NONE', #35731, 2.000000000000000444 ) ;
#16823 = FACE_OUTER_BOUND ( 'NONE', #44337, .T. ) ;
#16824 = CARTESIAN_POINT ( 'NONE',  ( 124.4819548109119722, -7.893985811506177619, -18.51759400769804742 ) ) ;
#16825 = CARTESIAN_POINT ( 'NONE',  ( 122.1561614775786353, -8.899110576539710493, -16.42337572283490132 ) ) ;
#16826 = ORIENTED_EDGE ( 'NONE', *, *, #19491, .T. ) ;
#16827 = CARTESIAN_POINT ( 'NONE',  ( 125.6732148109119862, 0.5811942927096110934, -14.16772938898807510 ) ) ;
#16828 = CARTESIAN_POINT ( 'NONE',  ( 119.0929214775786278, -5.638512984488999180, -18.83840828888717311 ) ) ;
#16829 = CARTESIAN_POINT ( 'NONE',  ( 113.2226630180080775, 0.7607806665038616689, -14.64321520033831447 ) ) ;
#16830 = CARTESIAN_POINT ( 'NONE',  ( 116.4267681442453153, -6.222761293078241884, -8.102969835052219238 ) ) ;
#16831 = CARTESIAN_POINT ( 'NONE',  ( 122.6667014775786413, -7.893985811506177619, -18.51759400769804742 ) ) ;
#16832 = CARTESIAN_POINT ( 'NONE',  ( 112.7745202545247878, -10.62599879583958717, -15.77991374673208469 ) ) ;
#16833 = CARTESIAN_POINT ( 'NONE',  ( 104.9957702545248566, 0.1403307496149616695, -11.32035403202665336 ) ) ;
#16834 = CARTESIAN_POINT ( 'NONE',  ( 116.1777233795247781, -8.938348069036489818, -17.46756447353520159 ) ) ;
#16835 = CARTESIAN_POINT ( 'NONE',  ( 116.1998614775786507, 0.4262465694468514643, -12.03445270309931736 ) ) ;
#16836 = AXIS2_PLACEMENT_3D ( 'NONE', #41003, #6553, #34351 ) ;
#16837 = CARTESIAN_POINT ( 'NONE',  ( 117.3343948109119737, -6.222761293078241884, -8.102969835052219238 ) ) ;
#16838 = CARTESIAN_POINT ( 'NONE',  ( 113.0341360982116754, 0.3867979994853637526, -12.14321520033829493 ) ) ;
#16839 = CARTESIAN_POINT ( 'NONE',  ( 115.0664733795247798, -1.325403438956436419, -9.854619843455211026 ) ) ;
#16840 = ORIENTED_EDGE ( 'NONE', *, *, #41810, .T. ) ;
#16841 = AXIS2_PLACEMENT_3D ( 'NONE', #43781, #37135, #19152 ) ;
#16842 = DIRECTION ( 'NONE',  ( 0.000000000000000000, -1.000000000000000000, 0.000000000000000000 ) ) ;
#16843 = CARTESIAN_POINT ( 'NONE',  ( 113.0231681442453322, 0.9020085738987339008, -11.91225656197089222 ) ) ;
#16844 = CARTESIAN_POINT ( 'NONE',  ( 122.9742476054816080, -2.287189184988711155, -18.07361239780447448 ) ) ;
#16845 = CARTESIAN_POINT ( 'NONE',  ( 123.2855641859119942, -8.321307733199551748, -9.223433127585318303 ) ) ;
#16846 = CARTESIAN_POINT ( 'NONE',  ( 121.6186891859119896, -1.406689858478933353, -17.56299727309130887 ) ) ;
#16847 = ORIENTED_EDGE ( 'NONE', *, *, #28384, .F. ) ;
#16848 = CARTESIAN_POINT ( 'NONE',  ( 27.78057335388972504, -13.48551096636548330, -8.893215200338314474 ) ) ;
#16849 = CARTESIAN_POINT ( 'NONE',  ( 116.7323956815296668, -11.78763665103780944, -21.33811264340862124 ) ) ;
#16850 = ORIENTED_EDGE ( 'NONE', *, *, #29281, .T. ) ;
#16851 = CARTESIAN_POINT ( 'NONE',  ( 118.4122014775786340, 0.5811942927096110934, -14.16772938898807510 ) ) ;
#16852 = CARTESIAN_POINT ( 'NONE',  ( 113.5337081442453240, -9.261995988541697145, -16.69588392320189030 ) ) ;
#16853 = ADVANCED_FACE ( 'NONE', ( #17440 ), #3080, .T. ) ;
#16854 = CARTESIAN_POINT ( 'NONE',  ( 120.0005481442453146, -4.153390946401325223, -8.397313243818185668 ) ) ;
#16855 = CARTESIAN_POINT ( 'NONE',  ( 71.67504600870660170, -26.72445618319088823, -4.893215200338314474 ) ) ;
#16856 = CARTESIAN_POINT ( 'NONE',  ( 121.0216281442452981, -1.561330072975668948, -17.79121239304076951 ) ) ;
#16857 = CARTESIAN_POINT ( 'NONE',  ( 117.5045748109119756, 0.5811942927096110934, -14.16772938898807510 ) ) ;
#16858 = CARTESIAN_POINT ( 'NONE',  ( 106.0375671295248310, 0.1403307496149613920, -13.39321520033831447 ) ) ;
#16859 = AXIS2_PLACEMENT_3D ( 'NONE', #33226, #36206, #26181 ) ;
#16860 = CARTESIAN_POINT ( 'NONE',  ( 112.7962614775786676, -6.222761293078241884, -8.102969835052219238 ) ) ;
#16861 = DIRECTION ( 'NONE',  ( 0.000000000000000000, 0.000000000000000000, -1.000000000000000000 ) ) ;
#16862 = VERTEX_POINT ( 'NONE', #6737 ) ;
#16863 =( BOUNDED_SURFACE ( )  B_SPLINE_SURFACE ( 1, 2, ( 
 ( #4094, #25318, #39212, #7977, #31914, #14597, #21885, #18696, #28517, #35781, #28961, #24638, #38520, #7298, #23241, #8431, #32801, #22777, #22337, #18910, #26658, #43313, #25987, #5444, #12534, #12081, #12310, #15950, #36674, #26207, #43995, #1573, #5896, #33469, #26435, #1796, #9105, #36232, #19819, #39892, #40572, #33022, #15723, #19364, #4997, #30081, #5223, #12757, #40342, #8653, #9332, #8878, #29853, #33705, #2249, #23007, #37122, #15265, #15494, #29175, #29401, #33253, #36899, #22554, #43087, #19139, #5670, #19587, #11855, #25762, #39668, #36454, #16178, #29625, #43540, #40114, #2025, #43768, #12987, #33934, #10463, #41037, #2477, #16402, #20050, #27345, #27568, #41482, #10022, #24365, #24148, #41264, #17086, #16632, #30526, #2934, #27113, #34602, #13440, #38040, #30755, #10239, #31197, #17307, #16864, #20276, #23474, #2703, #44903, #40802, #20943, #44677, #37360, #23931, #37811, #6586, #3387, #9794, #6131, #6815, #13661, #44448, #20504, #20723, #13215, #45117, #13875, #23704, #34383, #3164, #30978, #37593, #6366, #27785, #41699, #34162, #38251, #7031, #30300, #44227, #26883, #9558, #28013, #7245, #42367, #41918, #38469, #1690, #17739, #405, #25028, #32696, #31636, #31862, #35496, #11128, #629, #19027, #21158, #26095, #8546, #1465, #8765, #35263, #38923, #35033, #10683, #12197, #14094, #25872, #31412, #24585, #7693, #4268, #18187, #15389, #178, #21608, #29292, #43206, #11973, #39776, #3816, #22447, #17962, #36339, #4041, #5110, #14320, #32912, #15609, #29516, #28236, #34817, #43430, #40000, #3600, #42143, #17513, #10904, #24804, #38696, #14541, #7462, #21380, #28458, #13101, #37477, #37012, #30422, #23134, #6251, #40463, #26551, #33360, #33823, #44342, #43648, #6012, #40690, #26782, #41150, #2593, #23593, #29969, #13328, #12655, #20172, #22671, #12424, #16296, #27003, #40921, #36567, #44115, #19702, #5343, #9443, #9675, #34056, #9225, #2822, #16751, #30647, #27235, #44565, #19260, #33139, #5781, #12881, #1911, #8999, #33590, #2365, #23355, #40232, #22895 ),
 ( #15839, #29737, #36790, #30196, #26325, #5560, #19480, #2133, #16063, #37241, #19936, #43884, #16524, #10577, #31305, #20831, #38582, #41381, #525, #28128, #21050, #28344, #41598, #3714, #3052, #14437, #27905, #3497, #31755, #9911, #6709, #17196, #16978, #34713, #78, #38365, #34927, #27684, #24475, #20618, #10355, #13991, #13549, #30869, #23824, #34279, #300, #6481, #44791, #41820, #7139, #17634, #31530, #20395, #14213, #42037, #10797, #24693, #7360, #10136, #21275, #38152, #35157, #24263, #3937, #34495, #17857, #17414, #37711, #3271, #27460, #24041, #37933, #31088, #45015, #13773, #6926, #4164, #11022, #25381, #25818, #29020, #32425, #32646, #11919, #11476, #4837, #42707, #39727, #14889, #973, #7821, #8267, #18757, #18081, #25601, #15111, #1198, #15555, #22172, #43150, #4390, #32865, #32200, #8494, #42257, #31975, #35839, #1414, #15332, #24922, #18534, #39278, #38817, #42930, #29242, #22397, #28800, #36292, #5060, #18976, #1635, #7586, #21500, #35387, #8042, #11692, #738, #28577, #21948, #4612, #39506, #14661, #42484, #25154, #36067, #11246, #39050, #21729, #35616, #18305, #26945, #43599, #40868, #43833, #19425, #9622, #12600, #19206, #5729, #12827, #12144, #5959, #23075, #12371, #26272, #29918, #8945, #16467, #40411, #19884, #26502, #37185, #13046, #44292, #9171, #2086, #5291, #1856, #26725, #22618, #2772, #36958, #33085, #19648, #33535, #2313, #30371, #22846, #15785, #33771, #40634, #40179, #16243, #2540, #36738, #23544, #37426, #29687, #30145, #44060, #9391, #5504, #33311, #23301, #6196, #16011, #20116, #34002, #29461, #43375, #26047, #39951, #36518, #8713, #24208, #9858, #20342, #28073, #44741, #27407, #6874, #13939, #13501, #13722, #17366, #38100, #27630, #248, #2998, #7305, #34874, #27852, #35100, #3221, #10522, #23767, #21223, #41328, #41981, #34442, #17148, #20783, #6431, #31475, #6653, #14156, #41762, #10086, #10746, #10306, #31255, #16697, #3662, #24423, #24645, #38529, #34225, #30590, #16923, #34662, #38313, #30818, #44509, #20563, #7090, #21000 ) ),
 .UNSPECIFIED., .F., .F., .T. ) 
 B_SPLINE_SURFACE_WITH_KNOTS ( ( 2, 2 ),
 ( 3, 2, 2, 2, 2, 2, 2, 2, 2, 2, 2, 2, 2, 2, 2, 2, 2, 2, 2, 2, 2, 2, 2, 2, 2, 2, 2, 2, 2, 2, 2, 2, 2, 2, 2, 2, 2, 2, 2, 2, 2, 2, 2, 2, 2, 2, 2, 2, 2, 2, 2, 2, 2, 2, 2, 2, 2, 2, 2, 2, 2, 2, 2, 2, 2, 2, 2, 2, 2, 2, 2, 2, 2, 2, 2, 2, 2, 2, 2, 2, 2, 2, 2, 2, 2, 2, 2, 2, 2, 2, 2, 2, 2, 2, 2, 2, 2, 2, 2, 2, 2, 2, 2, 2, 2, 2, 2, 2, 2, 2, 2, 2, 2, 2, 2, 2, 2, 2, 2, 2, 2, 2, 2, 2, 2, 2, 2, 2, 3 ),
 ( 0.000000000000000000, 1.000000000000000000 ),
 ( 0.000000000000000000, 0.007812500000000000000, 0.01562500000000000000, 0.02343750000000000000, 0.03125000000000000000, 0.03906250000000000000, 0.04687500000000000000, 0.05468750000000000000, 0.06250000000000000000, 0.07031250000000000000, 0.07812500000000000000, 0.08593750000000000000, 0.09375000000000000000, 0.1015625000000000000, 0.1093750000000000000, 0.1171875000000000000, 0.1250000000000000000, 0.1328125000000000000, 0.1406250000000000000, 0.1484375000000000000, 0.1562500000000000000, 0.1640625000000000000, 0.1718750000000000000, 0.1796875000000000000, 0.1875000000000000000, 0.1953125000000000000, 0.2031250000000000000, 0.2109375000000000000, 0.2187500000000000000, 0.2265625000000000000, 0.2343750000000000000, 0.2421875000000000000, 0.2500000000000000000, 0.2578125000000000000, 0.2656250000000000000, 0.2734375000000000000, 0.2812500000000000000, 0.2890625000000000000, 0.2968750000000000000, 0.3046875000000000000, 0.3125000000000000000, 0.3203125000000000000, 0.3281250000000000000, 0.3359375000000000000, 0.3437500000000000000, 0.3515625000000000000, 0.3593750000000000000, 0.3671875000000000000, 0.3750000000000000000, 0.3828125000000000000, 0.3906250000000000000, 0.3984375000000000000, 0.4062500000000000000, 0.4140625000000000000, 0.4218750000000000000, 0.4296875000000000000, 0.4375000000000000000, 0.4453125000000000000, 0.4531250000000000000, 0.4609375000000000000, 0.4687500000000000000, 0.4765625000000000000, 0.4843750000000000000, 0.4921875000000000000, 0.5000000000000000000, 0.5078125000000000000, 0.5156250000000000000, 0.5234375000000000000, 0.5312500000000000000, 0.5390625000000000000, 0.5468750000000000000, 0.5546875000000000000, 0.5625000000000000000, 0.5703125000000000000, 0.5781250000000000000, 0.5859375000000000000, 0.5937500000000000000, 0.6015625000000000000, 0.6093750000000000000, 0.6171875000000000000, 0.6250000000000000000, 0.6328125000000000000, 0.6406250000000000000, 0.6484375000000000000, 0.6562500000000000000, 0.6640625000000000000, 0.6718750000000000000, 0.6796875000000000000, 0.6875000000000000000, 0.6953125000000000000, 0.7031250000000000000, 0.7109375000000000000, 0.7187500000000000000, 0.7265625000000000000, 0.7343750000000000000, 0.7421875000000000000, 0.7500000000000000000, 0.7578125000000000000, 0.7656250000000000000, 0.7734375000000000000, 0.7812500000000000000, 0.7890625000000000000, 0.7968750000000000000, 0.8046875000000000000, 0.8125000000000000000, 0.8203125000000000000, 0.8281250000000000000, 0.8359375000000000000, 0.8437500000000000000, 0.8515625000000000000, 0.8593750000000000000, 0.8671875000000000000, 0.8750000000000000000, 0.8828125000000000000, 0.8906250000000000000, 0.8984375000000000000, 0.9062500000000000000, 0.9140625000000000000, 0.9218750000000000000, 0.9296875000000000000, 0.9375000000000000000, 0.9453125000000000000, 0.9531250000000000000, 0.9609375000000000000, 0.9687500000000000000, 0.9765625000000000000, 0.9843750000000000000, 0.9921875000000000000, 1.000000000000000000 ),
 .UNSPECIFIED. ) 
 GEOMETRIC_REPRESENTATION_ITEM ( )  RATIONAL_B_SPLINE_SURFACE ( (
 ( 1.000000000000000000, 0.9238795325112869605, 1.000000000000000000, 0.9238795325112869605, 1.000000000000000000, 0.9238795325112869605, 1.000000000000000000, 0.9238795325112869605, 1.000000000000000000, 0.9238795325112869605, 1.000000000000000000, 0.9238795325112869605, 1.000000000000000000, 0.9238795325112869605, 1.000000000000000000, 0.9238795325112869605, 1.000000000000000000, 0.9238795325112869605, 1.000000000000000000, 0.9238795325112869605, 1.000000000000000000, 0.9238795325112869605, 1.000000000000000000, 0.9238795325112869605, 1.000000000000000000, 0.9238795325112869605, 1.000000000000000000, 0.9238795325112869605, 1.000000000000000000, 0.9238795325112869605, 1.000000000000000000, 0.9238795325112869605, 1.000000000000000000, 0.9238795325112869605, 1.000000000000000000, 0.9238795325112869605, 1.000000000000000000, 0.9238795325112869605, 1.000000000000000000, 0.9238795325112869605, 1.000000000000000000, 0.9238795325112869605, 1.000000000000000000, 0.9238795325112869605, 1.000000000000000000, 0.9238795325112869605, 1.000000000000000000, 0.9238795325112869605, 1.000000000000000000, 0.9238795325112869605, 1.000000000000000000, 0.9238795325112869605, 1.000000000000000000, 0.9238795325112869605, 1.000000000000000000, 0.9238795325112869605, 1.000000000000000000, 0.9238795325112869605, 1.000000000000000000, 0.9238795325112869605, 1.000000000000000000, 0.9238795325112869605, 1.000000000000000000, 0.9238795325112869605, 1.000000000000000000, 0.9238795325112869605, 1.000000000000000000, 0.9238795325112869605, 1.000000000000000000, 0.9238795325112869605, 1.000000000000000000, 0.9238795325112869605, 1.000000000000000000, 0.9238795325112869605, 1.000000000000000000, 0.9238795325112869605, 1.000000000000000000, 0.9238795325112869605, 1.000000000000000000, 0.9238795325112869605, 1.000000000000000000, 0.9238795325112869605, 1.000000000000000000, 0.9238795325112869605, 1.000000000000000000, 0.9238795325112869605, 1.000000000000000000, 0.9238795325112869605, 1.000000000000000000, 0.9238795325112869605, 1.000000000000000000, 0.9238795325112869605, 1.000000000000000000, 0.9238795325112869605, 1.000000000000000000, 0.9238795325112869605, 1.000000000000000000, 0.9238795325112869605, 1.000000000000000000, 0.9238795325112869605, 1.000000000000000000, 0.9238795325112869605, 1.000000000000000000, 0.9238795325112869605, 1.000000000000000000, 0.9238795325112869605, 1.000000000000000000, 0.9238795325112869605, 1.000000000000000000, 0.9238795325112869605, 1.000000000000000000, 0.9238795325112869605, 1.000000000000000000, 0.9238795325112869605, 1.000000000000000000, 0.9238795325112869605, 1.000000000000000000, 0.9238795325112869605, 1.000000000000000000, 0.9238795325112869605, 1.000000000000000000, 0.9238795325112869605, 1.000000000000000000, 0.9238795325112869605, 1.000000000000000000, 0.9238795325112869605, 1.000000000000000000, 0.9238795325112869605, 1.000000000000000000, 0.9238795325112869605, 1.000000000000000000, 0.9238795325112869605, 1.000000000000000000, 0.9238795325112869605, 1.000000000000000000, 0.9238795325112869605, 1.000000000000000000, 0.9238795325112869605, 1.000000000000000000, 0.9238795325112869605, 1.000000000000000000, 0.9238795325112869605, 1.000000000000000000, 0.9238795325112869605, 1.000000000000000000, 0.9238795325112869605, 1.000000000000000000, 0.9238795325112869605, 1.000000000000000000, 0.9238795325112869605, 1.000000000000000000, 0.9238795325112869605, 1.000000000000000000, 0.9238795325112869605, 1.000000000000000000, 0.9238795325112869605, 1.000000000000000000, 0.9238795325112869605, 1.000000000000000000, 0.9238795325112869605, 1.000000000000000000, 0.9238795325112869605, 1.000000000000000000, 0.9238795325112869605, 1.000000000000000000, 0.9238795325112869605, 1.000000000000000000, 0.9238795325112869605, 1.000000000000000000, 0.9238795325112869605, 1.000000000000000000, 0.9238795325112869605, 1.000000000000000000, 0.9238795325112869605, 1.000000000000000000, 0.9238795325112869605, 1.000000000000000000, 0.9238795325112869605, 1.000000000000000000, 0.9238795325112869605, 1.000000000000000000, 0.9238795325112869605, 1.000000000000000000, 0.9238795325112869605, 1.000000000000000000, 0.9238795325112869605, 1.000000000000000000, 0.9238795325112869605, 1.000000000000000000, 0.9238795325112869605, 1.000000000000000000, 0.9238795325112869605, 1.000000000000000000, 0.9238795325112869605, 1.000000000000000000, 0.9238795325112869605, 1.000000000000000000, 0.9238795325112869605, 1.000000000000000000, 0.9238795325112869605, 1.000000000000000000, 0.9238795325112869605, 1.000000000000000000, 0.9238795325112869605, 1.000000000000000000, 0.9238795325112869605, 1.000000000000000000, 0.9238795325112869605, 1.000000000000000000, 0.9238795325112869605, 1.000000000000000000, 0.9238795325112869605, 1.000000000000000000, 0.9238795325112869605, 1.000000000000000000, 0.9238795325112869605, 1.000000000000000000, 0.9238795325112869605, 1.000000000000000000, 0.9238795325112869605, 1.000000000000000000, 0.9238795325112869605, 1.000000000000000000, 0.9238795325112869605, 1.000000000000000000, 0.9238795325112869605, 1.000000000000000000, 0.9238795325112869605, 1.000000000000000000, 0.9238795325112869605, 1.000000000000000000, 0.9238795325112869605, 1.000000000000000000, 0.9238795325112869605, 1.000000000000000000, 0.9238795325112869605, 1.000000000000000000, 0.9238795325112869605, 1.000000000000000000, 0.9238795325112869605, 1.000000000000000000, 0.9238795325112869605, 1.000000000000000000, 0.9238795325112869605, 1.000000000000000000, 0.9238795325112869605, 1.000000000000000000, 0.9238795325112869605, 1.000000000000000000, 0.9238795325112869605, 1.000000000000000000, 0.9238795325112869605, 1.000000000000000000, 0.9238795325112869605, 1.000000000000000000, 0.9238795325112869605, 1.000000000000000000),
 ( 1.000000000000000000, 0.9238795325112869605, 1.000000000000000000, 0.9238795325112869605, 1.000000000000000000, 0.9238795325112869605, 1.000000000000000000, 0.9238795325112869605, 1.000000000000000000, 0.9238795325112869605, 1.000000000000000000, 0.9238795325112869605, 1.000000000000000000, 0.9238795325112869605, 1.000000000000000000, 0.9238795325112869605, 1.000000000000000000, 0.9238795325112869605, 1.000000000000000000, 0.9238795325112869605, 1.000000000000000000, 0.9238795325112869605, 1.000000000000000000, 0.9238795325112869605, 1.000000000000000000, 0.9238795325112869605, 1.000000000000000000, 0.9238795325112869605, 1.000000000000000000, 0.9238795325112869605, 1.000000000000000000, 0.9238795325112869605, 1.000000000000000000, 0.9238795325112869605, 1.000000000000000000, 0.9238795325112869605, 1.000000000000000000, 0.9238795325112869605, 1.000000000000000000, 0.9238795325112869605, 1.000000000000000000, 0.9238795325112869605, 1.000000000000000000, 0.9238795325112869605, 1.000000000000000000, 0.9238795325112869605, 1.000000000000000000, 0.9238795325112869605, 1.000000000000000000, 0.9238795325112869605, 1.000000000000000000, 0.9238795325112869605, 1.000000000000000000, 0.9238795325112869605, 1.000000000000000000, 0.9238795325112869605, 1.000000000000000000, 0.9238795325112869605, 1.000000000000000000, 0.9238795325112869605, 1.000000000000000000, 0.9238795325112869605, 1.000000000000000000, 0.9238795325112869605, 1.000000000000000000, 0.9238795325112869605, 1.000000000000000000, 0.9238795325112869605, 1.000000000000000000, 0.9238795325112869605, 1.000000000000000000, 0.9238795325112869605, 1.000000000000000000, 0.9238795325112869605, 1.000000000000000000, 0.9238795325112869605, 1.000000000000000000, 0.9238795325112869605, 1.000000000000000000, 0.9238795325112869605, 1.000000000000000000, 0.9238795325112869605, 1.000000000000000000, 0.9238795325112869605, 1.000000000000000000, 0.9238795325112869605, 1.000000000000000000, 0.9238795325112869605, 1.000000000000000000, 0.9238795325112869605, 1.000000000000000000, 0.9238795325112869605, 1.000000000000000000, 0.9238795325112869605, 1.000000000000000000, 0.9238795325112869605, 1.000000000000000000, 0.9238795325112869605, 1.000000000000000000, 0.9238795325112869605, 1.000000000000000000, 0.9238795325112869605, 1.000000000000000000, 0.9238795325112869605, 1.000000000000000000, 0.9238795325112869605, 1.000000000000000000, 0.9238795325112869605, 1.000000000000000000, 0.9238795325112869605, 1.000000000000000000, 0.9238795325112869605, 1.000000000000000000, 0.9238795325112869605, 1.000000000000000000, 0.9238795325112869605, 1.000000000000000000, 0.9238795325112869605, 1.000000000000000000, 0.9238795325112869605, 1.000000000000000000, 0.9238795325112869605, 1.000000000000000000, 0.9238795325112869605, 1.000000000000000000, 0.9238795325112869605, 1.000000000000000000, 0.9238795325112869605, 1.000000000000000000, 0.9238795325112869605, 1.000000000000000000, 0.9238795325112869605, 1.000000000000000000, 0.9238795325112869605, 1.000000000000000000, 0.9238795325112869605, 1.000000000000000000, 0.9238795325112869605, 1.000000000000000000, 0.9238795325112869605, 1.000000000000000000, 0.9238795325112869605, 1.000000000000000000, 0.9238795325112869605, 1.000000000000000000, 0.9238795325112869605, 1.000000000000000000, 0.9238795325112869605, 1.000000000000000000, 0.9238795325112869605, 1.000000000000000000, 0.9238795325112869605, 1.000000000000000000, 0.9238795325112869605, 1.000000000000000000, 0.9238795325112869605, 1.000000000000000000, 0.9238795325112869605, 1.000000000000000000, 0.9238795325112869605, 1.000000000000000000, 0.9238795325112869605, 1.000000000000000000, 0.9238795325112869605, 1.000000000000000000, 0.9238795325112869605, 1.000000000000000000, 0.9238795325112869605, 1.000000000000000000, 0.9238795325112869605, 1.000000000000000000, 0.9238795325112869605, 1.000000000000000000, 0.9238795325112869605, 1.000000000000000000, 0.9238795325112869605, 1.000000000000000000, 0.9238795325112869605, 1.000000000000000000, 0.9238795325112869605, 1.000000000000000000, 0.9238795325112869605, 1.000000000000000000, 0.9238795325112869605, 1.000000000000000000, 0.9238795325112869605, 1.000000000000000000, 0.9238795325112869605, 1.000000000000000000, 0.9238795325112869605, 1.000000000000000000, 0.9238795325112869605, 1.000000000000000000, 0.9238795325112869605, 1.000000000000000000, 0.9238795325112869605, 1.000000000000000000, 0.9238795325112869605, 1.000000000000000000, 0.9238795325112869605, 1.000000000000000000, 0.9238795325112869605, 1.000000000000000000, 0.9238795325112869605, 1.000000000000000000, 0.9238795325112869605, 1.000000000000000000, 0.9238795325112869605, 1.000000000000000000, 0.9238795325112869605, 1.000000000000000000, 0.9238795325112869605, 1.000000000000000000, 0.9238795325112869605, 1.000000000000000000, 0.9238795325112869605, 1.000000000000000000, 0.9238795325112869605, 1.000000000000000000, 0.9238795325112869605, 1.000000000000000000, 0.9238795325112869605, 1.000000000000000000, 0.9238795325112869605, 1.000000000000000000, 0.9238795325112869605, 1.000000000000000000, 0.9238795325112869605, 1.000000000000000000, 0.9238795325112869605, 1.000000000000000000, 0.9238795325112869605, 1.000000000000000000, 0.9238795325112869605, 1.000000000000000000, 0.9238795325112869605, 1.000000000000000000, 0.9238795325112869605, 1.000000000000000000, 0.9238795325112869605, 1.000000000000000000, 0.9238795325112869605, 1.000000000000000000, 0.9238795325112869605, 1.000000000000000000, 0.9238795325112869605, 1.000000000000000000, 0.9238795325112869605, 1.000000000000000000, 0.9238795325112869605, 1.000000000000000000, 0.9238795325112869605, 1.000000000000000000, 0.9238795325112869605, 1.000000000000000000, 0.9238795325112869605, 1.000000000000000000) ) ) 
 REPRESENTATION_ITEM ( '' )  SURFACE ( )  );
#16864 = CARTESIAN_POINT ( 'NONE',  ( 117.6180281442453150, -0.4660016031367893996, -10.09054647747474043 ) ) ;
#16865 = CARTESIAN_POINT ( 'NONE',  ( 120.6463454359119822, -11.07370829466463569, -12.81314460846529002 ) ) ;
#16866 = CARTESIAN_POINT ( 'NONE',  ( 114.1577014775786552, -6.344957434206662583, -7.627207830600332805 ) ) ;
#16867 = ORIENTED_EDGE ( 'NONE', *, *, #23670, .F. ) ;
#16868 = AXIS2_PLACEMENT_3D ( 'NONE', #18505, #36263, #15524 ) ;
#16869 = CARTESIAN_POINT ( 'NONE',  ( 121.0216281442452981, -1.561330072975668948, -17.79121239304076951 ) ) ;
#16870 = DIRECTION ( 'NONE',  ( -1.000000000000000000, 0.000000000000000000, 0.000000000000000000 ) ) ;
#16871 = CARTESIAN_POINT ( 'NONE',  ( 113.3635281442453504, -0.1624402480850797581, -16.17319339645315424 ) ) ;
#16872 = CARTESIAN_POINT ( 'NONE',  ( 124.8912734719562110, -1.125321370491286332, -17.12283323191017814 ) ) ;
#16873 = CARTESIAN_POINT ( 'NONE',  ( 115.1787814775786387, -0.1624402480850797581, -16.17319339645315424 ) ) ;
#16874 = DIRECTION ( 'NONE',  ( 1.000000000000000000, 0.000000000000000000, -0.000000000000000000 ) ) ;
#16875 = CARTESIAN_POINT ( 'NONE',  ( 117.3911214775786505, -7.894159318335828068, -9.358103419637847864 ) ) ;
#16876 = LINE ( 'NONE', #13000, #43420 ) ;
#16877 = CARTESIAN_POINT ( 'NONE',  ( 117.3911214775786505, -7.894159318335828068, -9.358103419637847864 ) ) ;
#16878 = CARTESIAN_POINT ( 'NONE',  ( 115.5191414775786569, -3.383040157471821630, -19.15922257007629170 ) ) ;
#16879 = CARTESIAN_POINT ( 'NONE',  ( 122.8688454359119646, -11.07370829466463569, -12.81314460846529002 ) ) ;
#16880 = CARTESIAN_POINT ( 'NONE',  ( 115.2355081442453155, -10.30919188438810075, -12.61870101168855918 ) ) ;
#16881 = CARTESIAN_POINT ( 'NONE',  ( 113.9875214775786532, -8.899110576539710493, -16.42337572283490132 ) ) ;
#16882 = CARTESIAN_POINT ( 'NONE',  ( 126.2404814775786264, -9.261995988541697145, -16.69588392320189030 ) ) ;
#16883 = CARTESIAN_POINT ( 'NONE',  ( 115.6325948109119821, -9.565557343593413364, -10.61323700422348004 ) ) ;
#16884 = ORIENTED_EDGE ( 'NONE', *, *, #13360, .T. ) ;
#16885 = CARTESIAN_POINT ( 'NONE',  ( 112.2857214775786474, -4.089484607189486809, -7.948022111789456723 ) ) ;
#16886 = CARTESIAN_POINT ( 'NONE',  ( 108.6767858795247861, -0.7896495226426338832, -17.46756447353520159 ) ) ;
#16887 = CARTESIAN_POINT ( 'NONE',  ( 106.2459265045248173, -2.791137627527939813, -8.388885654883777576 ) ) ;
#16888 = DIRECTION ( 'NONE',  ( -0.000000000000000000, -0.9284778069183721172, -0.3713878862591650232 ) ) ;
#16889 = AXIS2_PLACEMENT_3D ( 'NONE', #41388, #24050, #37247 ) ;
#16890 = CARTESIAN_POINT ( 'NONE',  ( 64.33603543187328455, -36.45978439725600850, -5.630764011073099873 ) ) ;
#16891 = CARTESIAN_POINT ( 'NONE',  ( 117.7882081442453170, -6.344957434206665248, -7.627207830600338134 ) ) ;
#16892 = ORIENTED_EDGE ( 'NONE', *, *, #6433, .T. ) ;
#16893 = DIRECTION ( 'NONE',  ( 1.000000000000000000, 0.000000000000000000, 0.000000000000000000 ) ) ;
#16894 = CARTESIAN_POINT ( 'NONE',  ( 135.3184548109119874, -4.863998795839242995, -13.39321520033831447 ) ) ;
#16895 = CARTESIAN_POINT ( 'NONE',  ( 118.2987481442453088, -7.894159318335828068, -9.358103419637847864 ) ) ;
#16896 = CARTESIAN_POINT ( 'NONE',  ( 123.1158699480702410, -6.365377317481717867, -18.95617363400926081 ) ) ;
#16897 = CARTESIAN_POINT ( 'NONE',  ( 125.0492214775786266, -6.344957434206665248, -7.627207830600338134 ) ) ;
#16898 = CARTESIAN_POINT ( 'NONE',  ( 116.0388171295248014, 0.1403307496149613920, -13.39321520033831447 ) ) ;
#16899 = CARTESIAN_POINT ( 'NONE',  ( 91.11246428952674137, -25.23119213852205789, -15.24166438581092109 ) ) ;
#16900 = ORIENTED_EDGE ( 'NONE', *, *, #25693, .F. ) ;
#16901 = CARTESIAN_POINT ( 'NONE',  ( 112.9097148109120070, 0.2603800115204892296, -16.42320221600525088 ) ) ;
#16902 = CIRCLE ( 'NONE', #18314, 2.999999999999999556 ) ;
#16903 = CARTESIAN_POINT ( 'NONE',  ( 121.2485348109119769, -8.899110576539710493, -16.42337572283490132 ) ) ;
#16904 = CARTESIAN_POINT ( 'NONE',  ( 118.3554748109119998, 0.2603800115204892296, -16.42320221600525088 ) ) ;
#16905 = CARTESIAN_POINT ( 'NONE',  ( 116.4834948109119779, -7.894159318335828068, -9.358103419637847864 ) ) ;
#16906 = CARTESIAN_POINT ( 'NONE',  ( 119.5467348109119712, -4.089484607189486809, -7.948022111789456723 ) ) ;
#16907 = DIRECTION ( 'NONE',  ( 0.5735764363510499342, 0.3127926500124801890, -0.7570804645221008711 ) ) ;
#16908 = DIRECTION ( 'NONE',  ( 0.000000000000000000, 0.000000000000000000, -1.000000000000000000 ) ) ;
#16909 = CARTESIAN_POINT ( 'NONE',  ( 124.3685014775786328, 0.4262465694468514643, -12.03445270309931736 ) ) ;
#16910 = ORIENTED_EDGE ( 'NONE', *, *, #7152, .F. ) ;
#16911 = FACE_OUTER_BOUND ( 'NONE', #43941, .T. ) ;
#16912 = CARTESIAN_POINT ( 'NONE',  ( 118.6391081442452986, -4.089484607189486809, -7.948022111789456723 ) ) ;
#16913 = CARTESIAN_POINT ( 'NONE',  ( 125.2194014775786286, 0.1319031606808879209, -14.10382304977623669 ) ) ;
#16914 = ORIENTED_EDGE ( 'NONE', *, *, #18985, .F. ) ;
#16915 = CARTESIAN_POINT ( 'NONE',  ( 123.7717360609119623, -3.387241619883791355, -18.17469012370385073 ) ) ;
#16916 = CARTESIAN_POINT ( 'NONE',  ( 61.28923319885182508, -12.47826754884034983, -9.611157264325234095 ) ) ;
#16917 = CARTESIAN_POINT ( 'NONE',  ( 119.0361948109119652, -7.893985811506177619, -18.51759400769804742 ) ) ;
#16918 = CARTESIAN_POINT ( 'NONE',  ( 106.5931921295248372, 0.8980012041604618078, -13.39321520033831447 ) ) ;
#16919 = CARTESIAN_POINT ( 'NONE',  ( 118.7525614775786380, -1.833838273342659253, -17.42832698103878286 ) ) ;
#16920 = ORIENTED_EDGE ( 'NONE', *, *, #19432, .F. ) ;
#16921 = ORIENTED_EDGE ( 'NONE', *, *, #28963, .T. ) ;
#16922 = CARTESIAN_POINT ( 'NONE',  ( 126.1270281442452870, 0.1319031606808879209, -14.10382304977623669 ) ) ;
#16923 = CARTESIAN_POINT ( 'NONE',  ( 125.3895814775786448, -2.084020599724406786, -8.691656652584148546 ) ) ;
#16924 = DIRECTION ( 'NONE',  ( 0.9609149988134837450, -0.1028163501681639419, 0.2570431154366518145 ) ) ;
#16925 = LINE ( 'NONE', #6876, #25069 ) ;
#16926 = CARTESIAN_POINT ( 'NONE',  ( 122.7801548109119665, -3.383040157471821630, -19.15922257007629170 ) ) ;
#16927 = CARTESIAN_POINT ( 'NONE',  ( 123.9584548109119737, -4.863998795839242995, -13.39321520033831447 ) ) ;
#16928 = CARTESIAN_POINT ( 'NONE',  ( 71.31713442278437753, 2.423123680056944007, -15.89321520033831447 ) ) ;
#16929 = CARTESIAN_POINT ( 'NONE',  ( 118.6391081442452986, -4.089484607189486809, -7.948022111789456723 ) ) ;
#16931 = CARTESIAN_POINT ( 'NONE',  ( 118.4689281442453392, -10.15424416112533912, -14.75197769757731336 ) ) ;
#16930 = CARTESIAN_POINT ( 'NONE',  ( 118.9227414775786400, -10.63000616557722466, -14.87417383870573495 ) ) ;
#16932 = CARTESIAN_POINT ( 'NONE',  ( 125.1059481442452750, -1.833838273342660141, -17.42832698103878286 ) ) ;
#16933 = CARTESIAN_POINT ( 'NONE',  ( 117.5045748109119756, 0.5811942927096110934, -14.16772938898807510 ) ) ;
#16934 = EDGE_CURVE ( 'NONE', #5517, #9582, #44652, .T. ) ;
#16935 = ORIENTED_EDGE ( 'NONE', *, *, #27338, .T. ) ;
#16936 = CARTESIAN_POINT ( 'NONE',  ( 125.2194014775786286, 0.1319031606808879209, -14.10382304977623669 ) ) ;
#16937 = CARTESIAN_POINT ( 'NONE',  ( 116.0840026197984827, -0.01983013475163192263, -12.14321520033831625 ) ) ;
#16938 = CARTESIAN_POINT ( 'NONE',  ( 106.7320983795247855, -0.7896495226426338832, -9.318865927141430916 ) ) ;
#16939 = CARTESIAN_POINT ( 'NONE',  ( 114.0246765045248196, -2.791137627527939813, -8.388885654883777576 ) ) ;
#16940 = CARTESIAN_POINT ( 'NONE',  ( 108.0517077545248696, -7.250697342233347165, -7.631215200338321125 ) ) ;
#16941 = CARTESIAN_POINT ( 'NONE',  ( 121.0216281442452981, -1.561330072975668948, -17.79121239304076951 ) ) ;
#16942 = CARTESIAN_POINT ( 'NONE',  ( 123.4608748109119745, 0.4262465694468514643, -12.03445270309931736 ) ) ;
#16943 =( BOUNDED_SURFACE ( )  B_SPLINE_SURFACE ( 1, 2, ( 
 ( #23515, #41076, #34418, #44485, #31012, #10063, #13699, #2973, #20093, #27607, #20315, #31232, #16670, #30345, #44718, #37402, #13252, #17342, #41521, #24183, #27154, #16901, #30794, #13478, #6853, #20760, #4, #27824, #10500, #32121, #31451, #220, #10722, #14580, #889, #14358, #28271, #21198, #17556, #21644, #3857, #31672, #31898, #18000, #21870, #25072, #25301, #35304, #14133, #35533, #14809, #28497, #664, #38505, #4305, #18227, #7068, #4076, #7282, #35075, #42628, #28722, #11392, #42180, #39193, #7959, #42403, #28049, #20979, #34852, #3638, #11167, #38965, #41957, #10940, #7734, #24622, #17779, #442, #24843, #38734, #7505, #21420, #17474, #31371, #16591, #37772, #27973, #7201, #23658, #17045, #6545, #143, #30938, #17265, #30713, #14057, #45074, #24329, #41441, #20685, #10199, #24546, #21114, #44635, #9977, #9746, #27525, #37999, #2659, #27749, #10641, #24106, #40994, #6993, #41879, #3345, #6775, #16820, #38215, #20905, #30484, #34562, #13400, #27302, #38433, #34778, #3561, #20461, #44405, #13170, #31154, #37544, #10422, #27072, #6318, #44861, #13834, #20235, #34122, #13616, #41665, #2891, #41217, #23888, #34343, #3121, #2927, #26877, #13654, #34156, #30294, #44671, #13868, #34377, #13433, #44220, #40795, #3380, #23466, #20043, #10455, #30748, #33925, #16856, #37805, #27336, #41257, #20716, #37352, #27779, #10233, #3158, #37116, #23698, #2696, #41030, #17299, #34596, #30520, #2469, #31191, #6580, #9550, #6809, #27108, #45110, #17079, #30971, #10014, #44895, #16394, #27560, #9784, #12981, #6124, #5888, #37585, #33699, #16625, #41475, #44442, #13209, #6357, #24140, #23923, #20270, #41692, #19810, #20496, #38032, #3594, #35025, #35487, #28898, #42359, #31630, #34808, #10676, #21825, #11342, #14984, #28450, #38915, #18180, #25253, #4491, #31854, #1072, #842, #4033, #38463, #7686, #172, #17955, #3808, #18413, #42809, #21600, #4261, #17506, #24358, #38689, #11121, #14313, #14088, #38245, #39150, #17732, #28005, #14762, #7454, #28677, #24578, #7024, #7236, #7915 ),
 ( #21152, #20934, #32075, #32305, #21373, #28229, #42136, #31404, #41913, #398, #35256, #10897, #35719, #623, #42579, #24797, #14535, #25021, #33190, #5160, #29565, #19077, #33408, #16115, #8369, #18850, #18634, #36389, #1740, #40048, #43701, #32742, #1516, #1965, #43256, #22052, #12021, #15435, #2185, #35945, #15892, #8148, #25924, #29789, #43483, #29114, #32963, #39830, #32522, #29342, #15663, #22275, #12250, #26146, #8816, #8596, #11794, #22717, #22494, #22947, #25701, #25477, #36616, #30015, #1297, #9047, #5391, #19309, #15209, #4714, #39383, #43026, #39608, #12474, #36169, #26373, #11570, #40283, #4935, #36840, #5608, #19532, #13599, #16574, #2642, #9496, #23184, #34329, #37295, #33872, #16803, #2873, #17246, #23873, #6758, #20219, #37062, #3101, #27509, #44617, #30468, #44388, #24089, #3325, #19757, #13152, #27055, #41427, #40973, #13383, #26828, #10183, #41200, #20445, #37527, #30698, #6300, #20668, #43934, #40739, #6064, #5835, #23640, #34105, #27285, #30921, #19983, #9729, #17029, #9959, #9276, #37758, #6528, #34543, #33639, #44844, #40513, #37983, #12700, #26600, #16341, #2415, #30244, #44166, #12930, #23411, #41865, #17906, #7406, #21324, #348, #31354, #35211, #34973, #42533, #129, #45060, #10846, #4441, #38199, #28623, #11068, #575, #6976, #27733, #13820, #20885, #41648, #14262, #10403, #38631, #35668, #32024, #34762, #3543, #17458, #31804, #789, #3761, #17683, #10626, #24314, #21548, #24529, #21095, #3983, #14484, #31136, #24970, #39099, #28394, #14040, #35437, #14711, #42305, #38866, #27957, #7635, #4214, #38416, #18130, #7186, #31581, #11293, #25202, #7869, #28178, #21777, #42086, #24742, #39329, #26092, #40228, #1905, #32693, #39771, #36786, #4658, #1462, #15384, #8542, #29289, #8992, #18579, #22892, #1685, #12420, #43202, #32250, #25868, #18359, #19257, #25427, #8096, #32471, #19022, #33135, #36115, #22219, #29064, #42759, #8761, #11742, #8318, #36336, #22444, #1020, #43426, #26320, #5106, #11523, #22667, #15834, #32909, #15606, #1247, #39996 ) ),
 .UNSPECIFIED., .F., .F., .T. ) 
 B_SPLINE_SURFACE_WITH_KNOTS ( ( 2, 2 ),
 ( 3, 2, 2, 2, 2, 2, 2, 2, 2, 2, 2, 2, 2, 2, 2, 2, 2, 2, 2, 2, 2, 2, 2, 2, 2, 2, 2, 2, 2, 2, 2, 2, 2, 2, 2, 2, 2, 2, 2, 2, 2, 2, 2, 2, 2, 2, 2, 2, 2, 2, 2, 2, 2, 2, 2, 2, 2, 2, 2, 2, 2, 2, 2, 2, 2, 2, 2, 2, 2, 2, 2, 2, 2, 2, 2, 2, 2, 2, 2, 2, 2, 2, 2, 2, 2, 2, 2, 2, 2, 2, 2, 2, 2, 2, 2, 2, 2, 2, 2, 2, 2, 2, 2, 2, 2, 2, 2, 2, 2, 2, 2, 2, 2, 2, 2, 2, 2, 2, 2, 2, 2, 2, 2, 2, 2, 2, 2, 2, 3 ),
 ( 0.000000000000000000, 1.000000000000000000 ),
 ( 0.000000000000000000, 0.007812500000000000000, 0.01562500000000000000, 0.02343750000000000000, 0.03125000000000000000, 0.03906250000000000000, 0.04687500000000000000, 0.05468750000000000000, 0.06250000000000000000, 0.07031250000000000000, 0.07812500000000000000, 0.08593750000000000000, 0.09375000000000000000, 0.1015625000000000000, 0.1093750000000000000, 0.1171875000000000000, 0.1250000000000000000, 0.1328125000000000000, 0.1406250000000000000, 0.1484375000000000000, 0.1562500000000000000, 0.1640625000000000000, 0.1718750000000000000, 0.1796875000000000000, 0.1875000000000000000, 0.1953125000000000000, 0.2031250000000000000, 0.2109375000000000000, 0.2187500000000000000, 0.2265625000000000000, 0.2343750000000000000, 0.2421875000000000000, 0.2500000000000000000, 0.2578125000000000000, 0.2656250000000000000, 0.2734375000000000000, 0.2812500000000000000, 0.2890625000000000000, 0.2968750000000000000, 0.3046875000000000000, 0.3125000000000000000, 0.3203125000000000000, 0.3281250000000000000, 0.3359375000000000000, 0.3437500000000000000, 0.3515625000000000000, 0.3593750000000000000, 0.3671875000000000000, 0.3750000000000000000, 0.3828125000000000000, 0.3906250000000000000, 0.3984375000000000000, 0.4062500000000000000, 0.4140625000000000000, 0.4218750000000000000, 0.4296875000000000000, 0.4375000000000000000, 0.4453125000000000000, 0.4531250000000000000, 0.4609375000000000000, 0.4687500000000000000, 0.4765625000000000000, 0.4843750000000000000, 0.4921875000000000000, 0.5000000000000000000, 0.5078125000000000000, 0.5156250000000000000, 0.5234375000000000000, 0.5312500000000000000, 0.5390625000000000000, 0.5468750000000000000, 0.5546875000000000000, 0.5625000000000000000, 0.5703125000000000000, 0.5781250000000000000, 0.5859375000000000000, 0.5937500000000000000, 0.6015625000000000000, 0.6093750000000000000, 0.6171875000000000000, 0.6250000000000000000, 0.6328125000000000000, 0.6406250000000000000, 0.6484375000000000000, 0.6562500000000000000, 0.6640625000000000000, 0.6718750000000000000, 0.6796875000000000000, 0.6875000000000000000, 0.6953125000000000000, 0.7031250000000000000, 0.7109375000000000000, 0.7187500000000000000, 0.7265625000000000000, 0.7343750000000000000, 0.7421875000000000000, 0.7500000000000000000, 0.7578125000000000000, 0.7656250000000000000, 0.7734375000000000000, 0.7812500000000000000, 0.7890625000000000000, 0.7968750000000000000, 0.8046875000000000000, 0.8125000000000000000, 0.8203125000000000000, 0.8281250000000000000, 0.8359375000000000000, 0.8437500000000000000, 0.8515625000000000000, 0.8593750000000000000, 0.8671875000000000000, 0.8750000000000000000, 0.8828125000000000000, 0.8906250000000000000, 0.8984375000000000000, 0.9062500000000000000, 0.9140625000000000000, 0.9218750000000000000, 0.9296875000000000000, 0.9375000000000000000, 0.9453125000000000000, 0.9531250000000000000, 0.9609375000000000000, 0.9687500000000000000, 0.9765625000000000000, 0.9843750000000000000, 0.9921875000000000000, 1.000000000000000000 ),
 .UNSPECIFIED. ) 
 GEOMETRIC_REPRESENTATION_ITEM ( )  RATIONAL_B_SPLINE_SURFACE ( (
 ( 1.000000000000000000, 0.9238795325112869605, 1.000000000000000000, 0.9238795325112869605, 1.000000000000000000, 0.9238795325112869605, 1.000000000000000000, 0.9238795325112869605, 1.000000000000000000, 0.9238795325112869605, 1.000000000000000000, 0.9238795325112869605, 1.000000000000000000, 0.9238795325112869605, 1.000000000000000000, 0.9238795325112869605, 1.000000000000000000, 0.9238795325112869605, 1.000000000000000000, 0.9238795325112869605, 1.000000000000000000, 0.9238795325112869605, 1.000000000000000000, 0.9238795325112869605, 1.000000000000000000, 0.9238795325112869605, 1.000000000000000000, 0.9238795325112869605, 1.000000000000000000, 0.9238795325112869605, 1.000000000000000000, 0.9238795325112869605, 1.000000000000000000, 0.9238795325112869605, 1.000000000000000000, 0.9238795325112869605, 1.000000000000000000, 0.9238795325112869605, 1.000000000000000000, 0.9238795325112869605, 1.000000000000000000, 0.9238795325112869605, 1.000000000000000000, 0.9238795325112869605, 1.000000000000000000, 0.9238795325112869605, 1.000000000000000000, 0.9238795325112869605, 1.000000000000000000, 0.9238795325112869605, 1.000000000000000000, 0.9238795325112869605, 1.000000000000000000, 0.9238795325112869605, 1.000000000000000000, 0.9238795325112869605, 1.000000000000000000, 0.9238795325112869605, 1.000000000000000000, 0.9238795325112869605, 1.000000000000000000, 0.9238795325112869605, 1.000000000000000000, 0.9238795325112869605, 1.000000000000000000, 0.9238795325112869605, 1.000000000000000000, 0.9238795325112869605, 1.000000000000000000, 0.9238795325112869605, 1.000000000000000000, 0.9238795325112869605, 1.000000000000000000, 0.9238795325112869605, 1.000000000000000000, 0.9238795325112869605, 1.000000000000000000, 0.9238795325112869605, 1.000000000000000000, 0.9238795325112869605, 1.000000000000000000, 0.9238795325112869605, 1.000000000000000000, 0.9238795325112869605, 1.000000000000000000, 0.9238795325112869605, 1.000000000000000000, 0.9238795325112869605, 1.000000000000000000, 0.9238795325112869605, 1.000000000000000000, 0.9238795325112869605, 1.000000000000000000, 0.9238795325112869605, 1.000000000000000000, 0.9238795325112869605, 1.000000000000000000, 0.9238795325112869605, 1.000000000000000000, 0.9238795325112869605, 1.000000000000000000, 0.9238795325112869605, 1.000000000000000000, 0.9238795325112869605, 1.000000000000000000, 0.9238795325112869605, 1.000000000000000000, 0.9238795325112869605, 1.000000000000000000, 0.9238795325112869605, 1.000000000000000000, 0.9238795325112869605, 1.000000000000000000, 0.9238795325112869605, 1.000000000000000000, 0.9238795325112869605, 1.000000000000000000, 0.9238795325112869605, 1.000000000000000000, 0.9238795325112869605, 1.000000000000000000, 0.9238795325112869605, 1.000000000000000000, 0.9238795325112869605, 1.000000000000000000, 0.9238795325112869605, 1.000000000000000000, 0.9238795325112869605, 1.000000000000000000, 0.9238795325112869605, 1.000000000000000000, 0.9238795325112869605, 1.000000000000000000, 0.9238795325112869605, 1.000000000000000000, 0.9238795325112869605, 1.000000000000000000, 0.9238795325112869605, 1.000000000000000000, 0.9238795325112869605, 1.000000000000000000, 0.9238795325112869605, 1.000000000000000000, 0.9238795325112869605, 1.000000000000000000, 0.9238795325112869605, 1.000000000000000000, 0.9238795325112869605, 1.000000000000000000, 0.9238795325112869605, 1.000000000000000000, 0.9238795325112869605, 1.000000000000000000, 0.9238795325112869605, 1.000000000000000000, 0.9238795325112869605, 1.000000000000000000, 0.9238795325112869605, 1.000000000000000000, 0.9238795325112869605, 1.000000000000000000, 0.9238795325112869605, 1.000000000000000000, 0.9238795325112869605, 1.000000000000000000, 0.9238795325112869605, 1.000000000000000000, 0.9238795325112869605, 1.000000000000000000, 0.9238795325112869605, 1.000000000000000000, 0.9238795325112869605, 1.000000000000000000, 0.9238795325112869605, 1.000000000000000000, 0.9238795325112869605, 1.000000000000000000, 0.9238795325112869605, 1.000000000000000000, 0.9238795325112869605, 1.000000000000000000, 0.9238795325112869605, 1.000000000000000000, 0.9238795325112869605, 1.000000000000000000, 0.9238795325112869605, 1.000000000000000000, 0.9238795325112869605, 1.000000000000000000, 0.9238795325112869605, 1.000000000000000000, 0.9238795325112869605, 1.000000000000000000, 0.9238795325112869605, 1.000000000000000000, 0.9238795325112869605, 1.000000000000000000, 0.9238795325112869605, 1.000000000000000000, 0.9238795325112869605, 1.000000000000000000, 0.9238795325112869605, 1.000000000000000000, 0.9238795325112869605, 1.000000000000000000, 0.9238795325112869605, 1.000000000000000000, 0.9238795325112869605, 1.000000000000000000, 0.9238795325112869605, 1.000000000000000000, 0.9238795325112869605, 1.000000000000000000, 0.9238795325112869605, 1.000000000000000000, 0.9238795325112869605, 1.000000000000000000, 0.9238795325112869605, 1.000000000000000000, 0.9238795325112869605, 1.000000000000000000, 0.9238795325112869605, 1.000000000000000000, 0.9238795325112869605, 1.000000000000000000, 0.9238795325112869605, 1.000000000000000000, 0.9238795325112869605, 1.000000000000000000, 0.9238795325112869605, 1.000000000000000000, 0.9238795325112869605, 1.000000000000000000, 0.9238795325112869605, 1.000000000000000000, 0.9238795325112869605, 1.000000000000000000, 0.9238795325112869605, 1.000000000000000000, 0.9238795325112869605, 1.000000000000000000, 0.9238795325112869605, 1.000000000000000000, 0.9238795325112869605, 1.000000000000000000, 0.9238795325112869605, 1.000000000000000000, 0.9238795325112869605, 1.000000000000000000, 0.9238795325112869605, 1.000000000000000000, 0.9238795325112869605, 1.000000000000000000, 0.9238795325112869605, 1.000000000000000000, 0.9238795325112869605, 1.000000000000000000),
 ( 1.000000000000000000, 0.9238795325112869605, 1.000000000000000000, 0.9238795325112869605, 1.000000000000000000, 0.9238795325112869605, 1.000000000000000000, 0.9238795325112869605, 1.000000000000000000, 0.9238795325112869605, 1.000000000000000000, 0.9238795325112869605, 1.000000000000000000, 0.9238795325112869605, 1.000000000000000000, 0.9238795325112869605, 1.000000000000000000, 0.9238795325112869605, 1.000000000000000000, 0.9238795325112869605, 1.000000000000000000, 0.9238795325112869605, 1.000000000000000000, 0.9238795325112869605, 1.000000000000000000, 0.9238795325112869605, 1.000000000000000000, 0.9238795325112869605, 1.000000000000000000, 0.9238795325112869605, 1.000000000000000000, 0.9238795325112869605, 1.000000000000000000, 0.9238795325112869605, 1.000000000000000000, 0.9238795325112869605, 1.000000000000000000, 0.9238795325112869605, 1.000000000000000000, 0.9238795325112869605, 1.000000000000000000, 0.9238795325112869605, 1.000000000000000000, 0.9238795325112869605, 1.000000000000000000, 0.9238795325112869605, 1.000000000000000000, 0.9238795325112869605, 1.000000000000000000, 0.9238795325112869605, 1.000000000000000000, 0.9238795325112869605, 1.000000000000000000, 0.9238795325112869605, 1.000000000000000000, 0.9238795325112869605, 1.000000000000000000, 0.9238795325112869605, 1.000000000000000000, 0.9238795325112869605, 1.000000000000000000, 0.9238795325112869605, 1.000000000000000000, 0.9238795325112869605, 1.000000000000000000, 0.9238795325112869605, 1.000000000000000000, 0.9238795325112869605, 1.000000000000000000, 0.9238795325112869605, 1.000000000000000000, 0.9238795325112869605, 1.000000000000000000, 0.9238795325112869605, 1.000000000000000000, 0.9238795325112869605, 1.000000000000000000, 0.9238795325112869605, 1.000000000000000000, 0.9238795325112869605, 1.000000000000000000, 0.9238795325112869605, 1.000000000000000000, 0.9238795325112869605, 1.000000000000000000, 0.9238795325112869605, 1.000000000000000000, 0.9238795325112869605, 1.000000000000000000, 0.9238795325112869605, 1.000000000000000000, 0.9238795325112869605, 1.000000000000000000, 0.9238795325112869605, 1.000000000000000000, 0.9238795325112869605, 1.000000000000000000, 0.9238795325112869605, 1.000000000000000000, 0.9238795325112869605, 1.000000000000000000, 0.9238795325112869605, 1.000000000000000000, 0.9238795325112869605, 1.000000000000000000, 0.9238795325112869605, 1.000000000000000000, 0.9238795325112869605, 1.000000000000000000, 0.9238795325112869605, 1.000000000000000000, 0.9238795325112869605, 1.000000000000000000, 0.9238795325112869605, 1.000000000000000000, 0.9238795325112869605, 1.000000000000000000, 0.9238795325112869605, 1.000000000000000000, 0.9238795325112869605, 1.000000000000000000, 0.9238795325112869605, 1.000000000000000000, 0.9238795325112869605, 1.000000000000000000, 0.9238795325112869605, 1.000000000000000000, 0.9238795325112869605, 1.000000000000000000, 0.9238795325112869605, 1.000000000000000000, 0.9238795325112869605, 1.000000000000000000, 0.9238795325112869605, 1.000000000000000000, 0.9238795325112869605, 1.000000000000000000, 0.9238795325112869605, 1.000000000000000000, 0.9238795325112869605, 1.000000000000000000, 0.9238795325112869605, 1.000000000000000000, 0.9238795325112869605, 1.000000000000000000, 0.9238795325112869605, 1.000000000000000000, 0.9238795325112869605, 1.000000000000000000, 0.9238795325112869605, 1.000000000000000000, 0.9238795325112869605, 1.000000000000000000, 0.9238795325112869605, 1.000000000000000000, 0.9238795325112869605, 1.000000000000000000, 0.9238795325112869605, 1.000000000000000000, 0.9238795325112869605, 1.000000000000000000, 0.9238795325112869605, 1.000000000000000000, 0.9238795325112869605, 1.000000000000000000, 0.9238795325112869605, 1.000000000000000000, 0.9238795325112869605, 1.000000000000000000, 0.9238795325112869605, 1.000000000000000000, 0.9238795325112869605, 1.000000000000000000, 0.9238795325112869605, 1.000000000000000000, 0.9238795325112869605, 1.000000000000000000, 0.9238795325112869605, 1.000000000000000000, 0.9238795325112869605, 1.000000000000000000, 0.9238795325112869605, 1.000000000000000000, 0.9238795325112869605, 1.000000000000000000, 0.9238795325112869605, 1.000000000000000000, 0.9238795325112869605, 1.000000000000000000, 0.9238795325112869605, 1.000000000000000000, 0.9238795325112869605, 1.000000000000000000, 0.9238795325112869605, 1.000000000000000000, 0.9238795325112869605, 1.000000000000000000, 0.9238795325112869605, 1.000000000000000000, 0.9238795325112869605, 1.000000000000000000, 0.9238795325112869605, 1.000000000000000000, 0.9238795325112869605, 1.000000000000000000, 0.9238795325112869605, 1.000000000000000000, 0.9238795325112869605, 1.000000000000000000, 0.9238795325112869605, 1.000000000000000000, 0.9238795325112869605, 1.000000000000000000, 0.9238795325112869605, 1.000000000000000000, 0.9238795325112869605, 1.000000000000000000, 0.9238795325112869605, 1.000000000000000000, 0.9238795325112869605, 1.000000000000000000, 0.9238795325112869605, 1.000000000000000000, 0.9238795325112869605, 1.000000000000000000, 0.9238795325112869605, 1.000000000000000000, 0.9238795325112869605, 1.000000000000000000, 0.9238795325112869605, 1.000000000000000000, 0.9238795325112869605, 1.000000000000000000, 0.9238795325112869605, 1.000000000000000000, 0.9238795325112869605, 1.000000000000000000, 0.9238795325112869605, 1.000000000000000000, 0.9238795325112869605, 1.000000000000000000, 0.9238795325112869605, 1.000000000000000000, 0.9238795325112869605, 1.000000000000000000, 0.9238795325112869605, 1.000000000000000000, 0.9238795325112869605, 1.000000000000000000, 0.9238795325112869605, 1.000000000000000000, 0.9238795325112869605, 1.000000000000000000, 0.9238795325112869605, 1.000000000000000000, 0.9238795325112869605, 1.000000000000000000) ) ) 
 REPRESENTATION_ITEM ( '' )  SURFACE ( )  );
#16944 = ORIENTED_EDGE ( 'NONE', *, *, #351, .T. ) ;
#16945 = CARTESIAN_POINT ( 'NONE',  ( 123.0070614775786169, 0.9020085738987339008, -11.91225656197089222 ) ) ;
#16946 = CARTESIAN_POINT ( 'NONE',  ( 113.5385046295247804, -4.863998795839590272, -7.631215200338315796 ) ) ;
#16947 = CARTESIAN_POINT ( 'NONE',  ( 112.7962614775786676, -6.222761293078241884, -8.102969835052219238 ) ) ;
#16948 = CARTESIAN_POINT ( 'NONE',  ( 91.38554522942851577, -25.38011337280982715, -14.88121679464376257 ) ) ;
#16949 = CARTESIAN_POINT ( 'NONE',  ( 124.6521348109119884, -1.561330072975668948, -17.79121239304076951 ) ) ;
#16950 = CARTESIAN_POINT ( 'NONE',  ( 120.2274548109119934, 0.5811942927096110934, -14.16772938898807510 ) ) ;
#16951 = CARTESIAN_POINT ( 'NONE',  ( 119.3235610609119846, -3.388519251035092328, -18.17055338314101220 ) ) ;
#16952 = CARTESIAN_POINT ( 'NONE',  ( 111.7751814775786556, -7.893985811506177619, -18.51759400769804742 ) ) ;
#16953 = CARTESIAN_POINT ( 'NONE',  ( 122.5215798109119874, -7.200787124940443817, -17.81845355600750835 ) ) ;
#16954 = CARTESIAN_POINT ( 'NONE',  ( 115.4831921295247952, -9.868328341294093420, -13.39321520033831447 ) ) ;
#16955 = VERTEX_POINT ( 'NONE', #13800 ) ;
#16956 = FACE_OUTER_BOUND ( 'NONE', #6871, .T. ) ;
#16957 = CARTESIAN_POINT ( 'NONE',  ( 113.4202548109119846, 0.1319031606808879209, -14.10382304977623669 ) ) ;
#16958 = CIRCLE ( 'NONE', #16190, 3.853420195439741125 ) ;
#16959 = CARTESIAN_POINT ( 'NONE',  ( 123.5743281442453139, -2.084020599724406786, -8.691656652584148546 ) ) ;
#16960 = CARTESIAN_POINT ( 'NONE',  ( 108.5378796295247810, -4.863998795839590272, -8.388885654883775800 ) ) ;
#16961 = CARTESIAN_POINT ( 'NONE',  ( 107.5655358795247736, -8.402594152722688392, -9.854619843455216355 ) ) ;
#16962 = CARTESIAN_POINT ( 'NONE',  ( 121.1350814775786233, -9.859900752359378018, -12.68260735090039759 ) ) ;
#16963 = CARTESIAN_POINT ( 'NONE',  ( 114.6682414775786469, -7.894159318335828068, -9.358103419637847864 ) ) ;
#16964 = CARTESIAN_POINT ( 'NONE',  ( 112.5693548109119888, 0.4262465694468514643, -12.03445270309931736 ) ) ;
#16965 = VERTEX_POINT ( 'NONE', #30897 ) ;
#16966 = AXIS2_PLACEMENT_3D ( 'NONE', #32521, #11793, #1296 ) ;
#16967 = EDGE_CURVE ( 'NONE', #14657, #8089, #12341, .T. ) ;
#16968 = CARTESIAN_POINT ( 'NONE',  ( 123.9714148109119805, -8.899110576539710493, -16.42337572283490132 ) ) ;
#16969 = VECTOR ( 'NONE', #37596, 1000.000000000000227 ) ;
#16970 = CARTESIAN_POINT ( 'NONE',  ( 119.2631014775786298, 0.2603800115204892296, -16.42320221600525088 ) ) ;
#16971 = CARTESIAN_POINT ( 'NONE',  ( 121.9470836909669913, -24.14644159042263993, -12.62951656296512937 ) ) ;
#16972 = VERTEX_POINT ( 'NONE', #6040 ) ;
#16973 = PLANE ( 'NONE',  #22343 ) ;
#16974 = EDGE_CURVE ( 'NONE', #21756, #32023, #35736, .T. ) ;
#16975 = EDGE_CURVE ( 'NONE', #22908, #21045, #25406, .T. ) ;
#16976 = EDGE_LOOP ( 'NONE', ( #43388, #29988, #42955, #4406, #27823 ) ) ;
#16977 = CARTESIAN_POINT ( 'NONE',  ( 114.8384214775786489, -10.15424416112533912, -14.75197769757731336 ) ) ;
#16978 = CARTESIAN_POINT ( 'NONE',  ( 113.0798948109119948, -8.899110576539710493, -16.42337572283490132 ) ) ;
#16979 = CARTESIAN_POINT ( 'NONE',  ( 114.8384214775786489, 0.9020085738987311252, -11.91225656197088867 ) ) ;
#16980 = CARTESIAN_POINT ( 'NONE',  ( 120.0212673109119805, 0.2312338769422704887, -16.08380026872395874 ) ) ;
#16981 = ORIENTED_EDGE ( 'NONE', *, *, #13329, .T. ) ;
#16982 = EDGE_CURVE ( 'NONE', #42225, #17020, #21753, .T. ) ;
#16983 = CONICAL_SURFACE ( 'NONE', #42457, 2.445500000000001339, 0.7853981633974680410 ) ;
#16984 = DIRECTION ( 'NONE',  ( -0.000000000000000000, -0.9284778069183720062, -0.3713878862591650232 ) ) ;
#16985 = CARTESIAN_POINT ( 'NONE',  ( 67.84197459855160162, -54.58317385897167640, -35.76526144576984478 ) ) ;
#16986 = CARTESIAN_POINT ( 'NONE',  ( 115.5526452545247622, 0.8980012041604421569, -11.00651665394454071 ) ) ;
#16987 = DIRECTION ( 'NONE',  ( -0.000000000000000000, -0.9284778069183718952, -0.3713878862591649677 ) ) ;
#16988 = EDGE_CURVE ( 'NONE', #12295, #27606, #32228, .T. ) ;
#16989 = CARTESIAN_POINT ( 'NONE',  ( 124.4252281442452812, -0.8288870151387760510, -10.36305467784173118 ) ) ;
#16990 = CARTESIAN_POINT ( 'NONE',  ( 112.9664414775786412, -9.859900752359374465, -12.68260735090039404 ) ) ;
#16991 = CARTESIAN_POINT ( 'NONE',  ( 70.19189222814998175, -60.76597359474132531, -37.50918677187066663 ) ) ;
#16992 = EDGE_CURVE ( 'NONE', #9431, #20329, #9682, .T. ) ;
#16993 = ADVANCED_FACE ( 'NONE', ( #10605 ), #33676, .T. ) ;
#16994 = ORIENTED_EDGE ( 'NONE', *, *, #17855, .F. ) ;
#16995 = LINE ( 'NONE', #44353, #3288 ) ;
#16996 = DIRECTION ( 'NONE',  ( -0.1352586133457952255, -0.9908103287288504424, 0.000000000000000000 ) ) ;
#16997 = CARTESIAN_POINT ( 'NONE',  ( 83.44708369096697709, -25.38011337280982715, -14.88121679464376257 ) ) ;
#16998 = CARTESIAN_POINT ( 'NONE',  ( 111.7184548109119788, -0.8288870151387760510, -10.36305467784173118 ) ) ;
#17000 = LINE ( 'NONE', #41835, #29799 ) ;
#16999 = CARTESIAN_POINT ( 'NONE',  ( 64.53261755725110049, -37.43192534259661386, -5.214988841577086198 ) ) ;
#17001 = CARTESIAN_POINT ( 'NONE',  ( 112.0588148109119828, 0.5811942927096154232, -14.16772938898807155 ) ) ;
#17002 = ORIENTED_EDGE ( 'NONE', *, *, #490, .F. ) ;
#17003 = CARTESIAN_POINT ( 'NONE',  ( 114.8951481442453115, -0.4660016031367893996, -10.09054647747474043 ) ) ;
#17004 = CARTESIAN_POINT ( 'NONE',  ( 126.4262034846959324, 0.08385758931630681035, -14.64587210211922930 ) ) ;
#17005 = CARTESIAN_POINT ( 'NONE',  ( 116.5249890045247980, 0.8980012041604421569, -15.77991374673208469 ) ) ;
#17006 = CARTESIAN_POINT ( 'NONE',  ( 125.5597614775786326, -7.894159318335828068, -9.358103419637847864 ) ) ;
#17007 = CARTESIAN_POINT ( 'NONE',  ( 123.0070614775786169, -10.15424416112533912, -14.75197769757731336 ) ) ;
#17008 = DIRECTION ( 'NONE',  ( 1.000000000000000000, 0.000000000000000000, -0.000000000000000000 ) ) ;
#17009 = CARTESIAN_POINT ( 'NONE',  ( 115.3442858795247759, -8.402594152722688392, -9.854619843455216355 ) ) ;
#17010 = DIRECTION ( 'NONE',  ( -0.3127730236694482580, 0.9498278979187074755, 0.000000000000000000 ) ) ;
#17011 = CARTESIAN_POINT ( 'NONE',  ( 112.1722681442453222, -8.899110576539710493, -16.42337572283490132 ) ) ;
#17012 = CARTESIAN_POINT ( 'NONE',  ( 108.0517077545248696, -7.250697342233347165, -7.631215200338321125 ) ) ;
#17013 = CARTESIAN_POINT ( 'NONE',  ( 117.2294421295248270, -10.43749303616872837, -4.992153861205963494 ) ) ;
#17014 = CARTESIAN_POINT ( 'NONE',  ( 113.8163171295247764, -10.62599879583958540, -13.39321520033831447 ) ) ;
#17015 = CARTESIAN_POINT ( 'NONE',  ( 125.3895814775786448, -7.893985811506177619, -18.51759400769804742 ) ) ;
#17016 = CARTESIAN_POINT ( 'NONE',  ( 125.1059481442452750, -8.166667518702819706, -8.995218007635861213 ) ) ;
#17017 = CARTESIAN_POINT ( 'NONE',  ( 67.30914723170953096, -57.87957791055376333, -37.24914645096997390 ) ) ;
#17018 = CARTESIAN_POINT ( 'NONE',  ( 119.8870948109119752, -9.261995988541697145, -16.69588392320189030 ) ) ;
#17019 = CARTESIAN_POINT ( 'NONE',  ( 111.8319081442453182, -5.638512984488999180, -18.83840828888717311 ) ) ;
#17020 = VERTEX_POINT ( 'NONE', #28602 ) ;
#17021 = CARTESIAN_POINT ( 'NONE',  ( 113.4769814775786330, 0.4262465694468514643, -12.03445270309931736 ) ) ;
#17022 = VECTOR ( 'NONE', #17340, 1000.000000000000227 ) ;
#17023 = CARTESIAN_POINT ( 'NONE',  ( 125.5030348109119558, -3.383040157471821630, -19.15922257007629170 ) ) ;
#17024 = VECTOR ( 'NONE', #23912, 1000.000000000000114 ) ;
#17025 = CARTESIAN_POINT ( 'NONE',  ( 123.4608748109119745, -10.63000616557722466, -14.87417383870573495 ) ) ;
#17026 = CARTESIAN_POINT ( 'NONE',  ( 115.4624148109119943, -5.638512984488999180, -18.83840828888717311 ) ) ;
#17027 = CARTESIAN_POINT ( 'NONE',  ( 115.5758681442453053, -7.894159318335828068, -9.358103419637847864 ) ) ;
#17028 = ORIENTED_EDGE ( 'NONE', *, *, #44578, .T. ) ;
#17029 = CARTESIAN_POINT ( 'NONE',  ( 118.5256548109119876, -8.899110576539710493, -16.42337572283490132 ) ) ;
#17030 = CARTESIAN_POINT ( 'NONE',  ( 112.3991748109119868, -8.166667518702817929, -8.995218007635859436 ) ) ;
#17031 = TOROIDAL_SURFACE ( 'NONE', #38833, 3.640000000000000124, 0.3600000000000000422 ) ;
#17032 = CARTESIAN_POINT ( 'NONE',  ( 125.2761281442453054, 0.4262465694468514643, -12.03445270309931736 ) ) ;
#17033 = CARTESIAN_POINT ( 'NONE',  ( 116.8819505665422724, 0.1389869644409600646, -15.19553865127072889 ) ) ;
#17034 = CARTESIAN_POINT ( 'NONE',  ( 111.4549108795247747, -8.938348069036489818, -9.318865927141430916 ) ) ;
#17035 = ORIENTED_EDGE ( 'NONE', *, *, #34209, .F. ) ;
#17036 = LINE ( 'NONE', #30704, #31520 ) ;
#17037 = CARTESIAN_POINT ( 'NONE',  ( 125.1059481442452750, -8.166667518702819706, -8.995218007635861213 ) ) ;
#17038 = EDGE_CURVE ( 'NONE', #12295, #19939, #6019, .T. ) ;
#17039 = CARTESIAN_POINT ( 'NONE',  ( 88.07785292173620917, -25.38011337280982715, -14.88121679464376257 ) ) ;
#17040 = CARTESIAN_POINT ( 'NONE',  ( 122.9868014478796425, -9.877548923986811502, -16.68609415519377137 ) ) ;
#17041 = CARTESIAN_POINT ( 'NONE',  ( 121.8363908503701509, -8.552676153439012552, -17.65880394779906837 ) ) ;
#17042 = CARTESIAN_POINT ( 'NONE',  ( 109.0935046295247872, -4.863998795839590272, -18.39754474579285315 ) ) ;
#17043 = ADVANCED_FACE ( 'NONE', ( #31781 ), #14020, .T. ) ;
#17044 = FACE_OUTER_BOUND ( 'NONE', #21970, .T. ) ;
#17045 = CARTESIAN_POINT ( 'NONE',  ( 116.8238548109119819, -4.089484607189486809, -7.948022111789456723 ) ) ;
#17046 = CARTESIAN_POINT ( 'NONE',  ( 122.8688454359119646, 0.5291689781388270175, -13.89700978578772705 ) ) ;
#17047 = DIRECTION ( 'NONE',  ( 1.000000000000000000, 0.000000000000000000, -0.000000000000000000 ) ) ;
#17048 = CARTESIAN_POINT ( 'NONE',  ( 124.5357204359119834, -10.25716656981734332, -12.88942061488921098 ) ) ;
#17049 = CARTESIAN_POINT ( 'NONE',  ( 121.2485348109119769, -8.899110576539710493, -16.42337572283490132 ) ) ;
#17050 = ORIENTED_EDGE ( 'NONE', *, *, #5225, .T. ) ;
#17051 = CARTESIAN_POINT ( 'NONE',  ( 85.82015659721905365, -25.99489077589524300, -13.39321520033831625 ) ) ;
#17052 = ADVANCED_FACE ( 'NONE', ( #35185 ), #18334, .T. ) ;
#17053 = CARTESIAN_POINT ( 'NONE',  ( 119.0361948109119652, -7.893985811506177619, -18.51759400769804742 ) ) ;
#17054 = DIRECTION ( 'NONE',  ( 1.000000000000000000, 0.000000000000000000, -0.000000000000000000 ) ) ;
#17055 = CARTESIAN_POINT ( 'NONE',  ( 114.4980614775786734, -2.084020599724406786, -8.691656652584148546 ) ) ;
#17056 = CARTESIAN_POINT ( 'NONE',  ( 113.3068014775786594, -1.833838273342658809, -17.42832698103878286 ) ) ;
#17057 = CARTESIAN_POINT ( 'NONE',  ( 111.1770983795247787, -0.7896495226426338832, -9.318865927141430916 ) ) ;
#17058 = CARTESIAN_POINT ( 'NONE',  ( 105.1346765045248475, -2.791137627527939813, -8.388885654883777576 ) ) ;
#17059 = CARTESIAN_POINT ( 'NONE',  ( 115.2748327545248657, -2.477300249445798297, -19.15521520033831138 ) ) ;
#17060 = CARTESIAN_POINT ( 'NONE',  ( 118.2987481442453088, -7.894159318335828068, -9.358103419637847864 ) ) ;
#17061 = CARTESIAN_POINT ( 'NONE',  ( 120.0572748109119772, -6.222761293078241884, -8.102969835052219238 ) ) ;
#17062 = CARTESIAN_POINT ( 'NONE',  ( 109.2294422377198515, -7.708454464063350109, -8.449852329660794581 ) ) ;
#17063 = CARTESIAN_POINT ( 'NONE',  ( 119.9518141859119851, -0.8832429491016019485, -18.19431474523657855 ) ) ;
#17064 = CARTESIAN_POINT ( 'NONE',  ( 107.9128015045248219, -6.936859964151250502, -18.39754474579286025 ) ) ;
#17065 = ORIENTED_EDGE ( 'NONE', *, *, #34209, .T. ) ;
#17066 = CARTESIAN_POINT ( 'NONE',  ( 109.2294421296414129, -0.4681310589162339664, -15.92169685210972574 ) ) ;
#17067 = CARTESIAN_POINT ( 'NONE',  ( 113.7038881442453402, -3.383040157471821630, -19.15922257007629170 ) ) ;
#17068 = CARTESIAN_POINT ( 'NONE',  ( 114.8384214775786489, 0.9020085738987339008, -11.91225656197089222 ) ) ;
#17069 = CARTESIAN_POINT ( 'NONE',  ( 61.63318325272354770, -19.46990085680238636, -14.39321520033831625 ) ) ;
#17070 = CARTESIAN_POINT ( 'NONE',  ( 119.4656423109119743, -0.4387604401700512802, -15.73000352943951619 ) ) ;
#17071 = VERTEX_POINT ( 'NONE', #107 ) ;
#17072 = CARTESIAN_POINT ( 'NONE',  ( 113.6079577545248185, -7.250697342233347165, -7.631215200338321125 ) ) ;
#17073 = VERTEX_POINT ( 'NONE', #4190 ) ;
#17074 = CARTESIAN_POINT ( 'NONE',  ( 121.1918081442452859, 0.9020085738987339008, -11.91225656197089222 ) ) ;
#17075 = CARTESIAN_POINT ( 'NONE',  ( 113.2500748109119968, -6.344957434206662583, -7.627207830600332805 ) ) ;
#17076 = CARTESIAN_POINT ( 'NONE',  ( 118.4122014775786340, -9.859900752359374465, -12.68260735090039404 ) ) ;
#17077 = SHAPE_REPRESENTATION_RELATIONSHIP ( 'NONE' , 'NONE' ,  #21588, #24824 ) ;
#17078 = CARTESIAN_POINT ( 'NONE',  ( 71.04661719609278236, 0.4415030225992447321, -19.39321520033831447 ) ) ;
#17079 = CARTESIAN_POINT ( 'NONE',  ( 122.3263414775786373, -6.344957434206665248, -7.627207830600338134 ) ) ;
#17080 = CARTESIAN_POINT ( 'NONE',  ( 116.5402214775786405, 0.2603800115204892296, -16.42320221600525088 ) ) ;
#17081 = AXIS2_PLACEMENT_3D ( 'NONE', #4955, #28919, #7705 ) ;
#17082 = CARTESIAN_POINT ( 'NONE',  ( 107.6349890045248401, -9.868328341294098749, -11.32035403202665869 ) ) ;
#17083 = CARTESIAN_POINT ( 'NONE',  ( 111.3213681442453264, -7.643976991954077427, -18.09477374809248928 ) ) ;
#17084 = DIRECTION ( 'NONE',  ( -0.4225728684367167642, 0.9063289528979890930, 0.000000000000000000 ) ) ;
#17085 = ORIENTED_EDGE ( 'NONE', *, *, #37354, .T. ) ;
#17086 = CARTESIAN_POINT ( 'NONE',  ( 116.9373081442452929, -8.166667518702817929, -8.995218007635861213 ) ) ;
#17087 = EDGE_CURVE ( 'NONE', #41059, #38747, #7385, .T. ) ;
#17088 = CARTESIAN_POINT ( 'NONE',  ( 121.4797829359119987, -4.283928203966213211, -7.183505701512925334 ) ) ;
#17089 = CARTESIAN_POINT ( 'NONE',  ( 115.2922348109119781, -10.63000616557722466, -14.87417383870573495 ) ) ;
#17090 = EDGE_LOOP ( 'NONE', ( #43539, #5028, #3168, #72, #10155 ) ) ;
#17091 = CARTESIAN_POINT ( 'NONE',  ( 115.5526452545247622, 0.8980012041604421569, -11.00651665394454071 ) ) ;
#17092 = CARTESIAN_POINT ( 'NONE',  ( 126.2404814775786264, -9.261995988541697145, -16.69588392320189030 ) ) ;
#17093 = LINE ( 'NONE', #34167, #1200 ) ;
#17094 = CARTESIAN_POINT ( 'NONE',  ( 69.01908044833261613, -25.32952000468398879, -0.8932152003383146965 ) ) ;
#17095 = CARTESIAN_POINT ( 'NONE',  ( 78.39334728892299609, -58.37107721070194799, -0.4530934645980765896 ) ) ;
#17096 = CARTESIAN_POINT ( 'NONE',  ( 117.1642148109119859, -0.8288870151387760510, -10.36305467784173118 ) ) ;
#17097 = CARTESIAN_POINT ( 'NONE',  ( 111.7184548109119788, -9.142054238649166109, -15.98131134002176523 ) ) ;
#17098 = CARTESIAN_POINT ( 'NONE',  ( 119.6601881442453106, -1.833838273342659253, -17.42832698103878286 ) ) ;
#17099 = ADVANCED_FACE ( 'NONE', ( #32002 ), #38392, .T. ) ;
#17100 = FACE_BOUND ( 'NONE', #17187, .T. ) ;
#17101 = CARTESIAN_POINT ( 'NONE',  ( 114.8384214775786489, -10.15424416112533912, -14.75197769757731336 ) ) ;
#17102 = CARTESIAN_POINT ( 'NONE',  ( 124.1884548109119777, -7.554583864224885481, -18.48844787311982785 ) ) ;
#17103 = CARTESIAN_POINT ( 'NONE',  ( 114.3278814775786429, -10.30919188438810075, -12.61870101168855918 ) ) ;
#17104 =( GEOMETRIC_REPRESENTATION_CONTEXT ( 3 ) GLOBAL_UNCERTAINTY_ASSIGNED_CONTEXT ( ( #7345 ) ) GLOBAL_UNIT_ASSIGNED_CONTEXT ( ( #8867, #11616, #18464 ) ) REPRESENTATION_CONTEXT ( 'NONE', 'WORKASPACE' ) );
#17105 = CARTESIAN_POINT ( 'NONE',  ( 113.7038881442453402, -6.222761293078241884, -8.102969835052219238 ) ) ;
#17106 = AXIS2_PLACEMENT_3D ( 'NONE', #3830, #34393, #20287 ) ;
#17107 = CARTESIAN_POINT ( 'NONE',  ( 115.8027748109119841, -8.899110576539710493, -16.42337572283490132 ) ) ;
#17108 = EDGE_LOOP ( 'NONE', ( #36270, #16686, #14226, #23401, #21021, #20451 ) ) ;
#17109 = CARTESIAN_POINT ( 'NONE',  ( 115.5191414775786569, -3.383040157471821630, -19.15922257007629170 ) ) ;
#17110 = CARTESIAN_POINT ( 'NONE',  ( 107.3571765045248299, -7.250697342233347165, -19.15521520033831138 ) ) ;
#17111 = CARTESIAN_POINT ( 'NONE',  ( 70.19189222814998175, -84.91840466455968794, -47.17007500872661296 ) ) ;
#17112 = CARTESIAN_POINT ( 'NONE',  ( 104.9263171295248327, 0.1403307496149613920, -13.39321520033831447 ) ) ;
#17113 = CARTESIAN_POINT ( 'NONE',  ( 121.6186891859119754, -1.406689858478935573, -17.56299727309130887 ) ) ;
#17114 = CARTESIAN_POINT ( 'NONE',  ( 123.6877814775786533, -3.383040157471821630, -19.15922257007629170 ) ) ;
#17115 = ORIENTED_EDGE ( 'NONE', *, *, #23651, .T. ) ;
#17116 = CARTESIAN_POINT ( 'NONE',  ( 67.84197459855160162, -54.58317385897167640, -35.76526144576984478 ) ) ;
#17117 = CARTESIAN_POINT ( 'NONE',  ( 117.4478481442453131, -9.565557343593413364, -10.61323700422348004 ) ) ;
#17118 = CARTESIAN_POINT ( 'NONE',  ( 76.69189222814998175, -50.16718729050181480, 3.106784799661685526 ) ) ;
#17119 = CARTESIAN_POINT ( 'NONE',  ( 123.3474214775786209, -9.988377603198976828, -10.36322818467138340 ) ) ;
#17120 = CARTESIAN_POINT ( 'NONE',  ( 106.9404577545248145, -7.250697342233347165, -7.631215200338321125 ) ) ;
#17121 = CARTESIAN_POINT ( 'NONE',  ( 89.27853238427192650, -9.950806628697387524, -13.58228004074779705 ) ) ;
#17122 = VERTEX_POINT ( 'NONE', #21303 ) ;
#17123 = CARTESIAN_POINT ( 'NONE',  ( 125.4584548109119737, -13.11073630560948722, -15.94021774473354114 ) ) ;
#17124 = CARTESIAN_POINT ( 'NONE',  ( 111.8319081442453182, -5.638512984488999180, -18.83840828888717311 ) ) ;
#17125 = CARTESIAN_POINT ( 'NONE',  ( 122.2696148109119889, -4.089484607189486809, -7.948022111789456723 ) ) ;
#17126 = EDGE_CURVE ( 'NONE', #39715, #35887, #7968, .T. ) ;
#17127 = CARTESIAN_POINT ( 'NONE',  ( 115.4056881442453459, -2.084020599724406786, -8.691656652584148546 ) ) ;
#17128 = CARTESIAN_POINT ( 'NONE',  ( 82.53488078675573547, -31.62014037238083830, -22.36964567811433469 ) ) ;
#17129 = CARTESIAN_POINT ( 'NONE',  ( 120.5110881442453206, -6.344957434206665248, -7.627207830600338134 ) ) ;
#17130 = DIRECTION ( 'NONE',  ( -0.9609149988134837450, 0.1028163501681639419, -0.2570431154366518145 ) ) ;
#17131 =( BOUNDED_SURFACE ( )  B_SPLINE_SURFACE ( 1, 2, ( 
 ( #35568, #18261, #15285, #29192, #11874, #32157, #28754, #42659, #39685, #11430, #8450, #36247, #26457, #13229, #5460, #27130, #6149, #2043, #19604, #2266, #40359, #43556, #23027, #30542, #2722, #44014, #9348, #12776, #41054, #12550, #20069, #16194, #33488, #8898, #30098, #44464, #26224, #26901, #9811, #26678, #34176, #2494, #36690, #2952, #40589, #23720, #37379, #23257, #15966, #19380, #40822, #43785, #9123, #40133, #13003, #36914, #22796, #37141, #5915, #5685, #29870, #33268, #33955, #19837, #9577 ),
 ( #33724, #23493, #37610, #20292, #16423, #12324, #6384, #30319, #44245, #16648, #29642, #13677, #41280, #35052, #34831, #3835, #7048, #24163, #37827, #21400, #6833, #44696, #13456, #6605, #3616, #20738, #20518, #17534, #17755, #10256, #38055, #20959, #10040, #34618, #31652, #3405, #24821, #420, #24602, #17322, #38712, #28028, #27360, #31429, #35280, #16879, #31212, #30994, #13895, #30770, #34398, #45136, #27801, #38485, #21177, #196, #38267, #23947, #7260, #41936, #44920, #14336, #7481, #3179, #17102 ) ),
 .UNSPECIFIED., .F., .F., .T. ) 
 B_SPLINE_SURFACE_WITH_KNOTS ( ( 2, 2 ),
 ( 3, 2, 2, 2, 2, 2, 2, 2, 2, 2, 2, 2, 2, 2, 2, 2, 2, 2, 2, 2, 2, 2, 2, 2, 2, 2, 2, 2, 2, 2, 2, 2, 3 ),
 ( 0.000000000000000000, 1.000000000000000000 ),
 ( 0.000000000000000000, 0.03125000000000000000, 0.06250000000000000000, 0.09375000000000000000, 0.1250000000000000000, 0.1562500000000000000, 0.1875000000000000000, 0.2187500000000000000, 0.2500000000000000000, 0.2812500000000000000, 0.3125000000000000000, 0.3437500000000000000, 0.3750000000000000000, 0.4062500000000000000, 0.4375000000000000000, 0.4687500000000000000, 0.5000000000000000000, 0.5312500000000000000, 0.5625000000000000000, 0.5937500000000000000, 0.6250000000000000000, 0.6562500000000000000, 0.6875000000000000000, 0.7187500000000000000, 0.7500000000000000000, 0.7812500000000000000, 0.8125000000000000000, 0.8437500000000000000, 0.8750000000000000000, 0.9062500000000000000, 0.9375000000000000000, 0.9687500000000000000, 1.000000000000000000 ),
 .UNSPECIFIED. ) 
 GEOMETRIC_REPRESENTATION_ITEM ( )  RATIONAL_B_SPLINE_SURFACE ( (
 ( 1.000000000000000000, 0.9238795325112869605, 1.000000000000000000, 0.9238795325112869605, 1.000000000000000000, 0.9238795325112869605, 1.000000000000000000, 0.9238795325112869605, 1.000000000000000000, 0.9238795325112869605, 1.000000000000000000, 0.9238795325112869605, 1.000000000000000000, 0.9238795325112869605, 1.000000000000000000, 0.9238795325112869605, 1.000000000000000000, 0.9238795325112869605, 1.000000000000000000, 0.9238795325112869605, 1.000000000000000000, 0.9238795325112869605, 1.000000000000000000, 0.9238795325112869605, 1.000000000000000000, 0.9238795325112869605, 1.000000000000000000, 0.9238795325112869605, 1.000000000000000000, 0.9238795325112869605, 1.000000000000000000, 0.9238795325112869605, 1.000000000000000000, 0.9238795325112869605, 1.000000000000000000, 0.9238795325112869605, 1.000000000000000000, 0.9238795325112869605, 1.000000000000000000, 0.9238795325112869605, 1.000000000000000000, 0.9238795325112869605, 1.000000000000000000, 0.9238795325112869605, 1.000000000000000000, 0.9238795325112869605, 1.000000000000000000, 0.9238795325112869605, 1.000000000000000000, 0.9238795325112869605, 1.000000000000000000, 0.9238795325112869605, 1.000000000000000000, 0.9238795325112869605, 1.000000000000000000, 0.9238795325112869605, 1.000000000000000000, 0.9238795325112869605, 1.000000000000000000, 0.9238795325112869605, 1.000000000000000000, 0.9238795325112869605, 1.000000000000000000, 0.9238795325112869605, 1.000000000000000000),
 ( 1.000000000000000000, 0.9238795325112869605, 1.000000000000000000, 0.9238795325112869605, 1.000000000000000000, 0.9238795325112869605, 1.000000000000000000, 0.9238795325112869605, 1.000000000000000000, 0.9238795325112869605, 1.000000000000000000, 0.9238795325112869605, 1.000000000000000000, 0.9238795325112869605, 1.000000000000000000, 0.9238795325112869605, 1.000000000000000000, 0.9238795325112869605, 1.000000000000000000, 0.9238795325112869605, 1.000000000000000000, 0.9238795325112869605, 1.000000000000000000, 0.9238795325112869605, 1.000000000000000000, 0.9238795325112869605, 1.000000000000000000, 0.9238795325112869605, 1.000000000000000000, 0.9238795325112869605, 1.000000000000000000, 0.9238795325112869605, 1.000000000000000000, 0.9238795325112869605, 1.000000000000000000, 0.9238795325112869605, 1.000000000000000000, 0.9238795325112869605, 1.000000000000000000, 0.9238795325112869605, 1.000000000000000000, 0.9238795325112869605, 1.000000000000000000, 0.9238795325112869605, 1.000000000000000000, 0.9238795325112869605, 1.000000000000000000, 0.9238795325112869605, 1.000000000000000000, 0.9238795325112869605, 1.000000000000000000, 0.9238795325112869605, 1.000000000000000000, 0.9238795325112869605, 1.000000000000000000, 0.9238795325112869605, 1.000000000000000000, 0.9238795325112869605, 1.000000000000000000, 0.9238795325112869605, 1.000000000000000000, 0.9238795325112869605, 1.000000000000000000, 0.9238795325112869605, 1.000000000000000000) ) ) 
 REPRESENTATION_ITEM ( '' )  SURFACE ( )  );
#17132 = CARTESIAN_POINT ( 'NONE',  ( 124.1415948109119540, -3.505236298600246325, -18.68346056562440793 ) ) ;
#17133 = ORIENTED_EDGE ( 'NONE', *, *, #39109, .T. ) ;
#17134 = AXIS2_PLACEMENT_3D ( 'NONE', #21447, #35332, #18023 ) ;
#17135 = DIRECTION ( 'NONE',  ( -1.000000000000000000, 0.000000000000000000, 0.000000000000000000 ) ) ;
#17136 = CARTESIAN_POINT ( 'NONE',  ( 116.2565881442452991, -9.261995988541697145, -16.69588392320189030 ) ) ;
#17137 = CARTESIAN_POINT ( 'NONE',  ( 125.7866681442452688, -8.899110576539710493, -16.42337572283490132 ) ) ;
#17138 = VERTEX_POINT ( 'NONE', #18784 ) ;
#17139 = CARTESIAN_POINT ( 'NONE',  ( 124.1190016859119680, -9.665098340737509730, -17.37397104707595474 ) ) ;
#17140 = DIRECTION ( 'NONE',  ( 0.9063289528979890930, 0.4225728684367167087, 0.000000000000000000 ) ) ;
#17141 = CARTESIAN_POINT ( 'NONE',  ( 122.1561614775786353, -0.4660016031367893996, -10.09054647747474043 ) ) ;
#17142 = VECTOR ( 'NONE', #28471, 1000.000000000000000 ) ;
#17143 = CARTESIAN_POINT ( 'NONE',  ( 108.2600671295247992, -10.62599879583958540, -13.39321520033831447 ) ) ;
#17144 = CARTESIAN_POINT ( 'NONE',  ( 120.0005481442453146, -4.153390946401325223, -8.397313243818185668 ) ) ;
#17145 = ORIENTED_EDGE ( 'NONE', *, *, #31701, .T. ) ;
#17146 = ORIENTED_EDGE ( 'NONE', *, *, #3118, .T. ) ;
#17147 = CARTESIAN_POINT ( 'NONE',  ( 115.8027748109119841, -0.4660016031367893996, -10.09054647747474043 ) ) ;
#17148 = CARTESIAN_POINT ( 'NONE',  ( 124.3685014775786328, 0.4262465694468514643, -12.03445270309931736 ) ) ;
#17149 = CARTESIAN_POINT ( 'NONE',  ( 74.82520252044861309, -48.51951888521425360, -14.39321520033831625 ) ) ;
#17150 = DIRECTION ( 'NONE',  ( 0.000000000000000000, 0.6004852223388321697, -0.7996358532186279566 ) ) ;
#17151 = CARTESIAN_POINT ( 'NONE',  ( 121.4187148109119789, -6.344957434206665248, -7.627207830600338134 ) ) ;
#17152 = CARTESIAN_POINT ( 'NONE',  ( 66.06194382436763135, -14.97931106434683635, -19.39321520033831447 ) ) ;
#17153 = ADVANCED_FACE ( 'NONE', ( #26529 ), #43403, .T. ) ;
#17154 = CARTESIAN_POINT ( 'NONE',  ( 117.3719165460472027, -2.191907684172563986, -18.20049396185734025 ) ) ;
#17155 = CARTESIAN_POINT ( 'NONE',  ( 119.8303681442453126, -10.63000616557722466, -14.87417383870573495 ) ) ;
#17157 = CARTESIAN_POINT ( 'NONE',  ( 121.4187148109119789, -3.505236298600246325, -18.68346056562440793 ) ) ;
#17156 = CARTESIAN_POINT ( 'NONE',  ( 117.1074881442453233, -10.63000616557722466, -14.87417383870573495 ) ) ;
#17158 = DIRECTION ( 'NONE',  ( 0.000000000000000000, -0.9242245927363026414, -0.3818493186865934419 ) ) ;
#17159 = CARTESIAN_POINT ( 'NONE',  ( 117.2776681442452968, -5.638512984488999180, -18.83840828888717311 ) ) ;
#17160 = ORIENTED_EDGE ( 'NONE', *, *, #40060, .T. ) ;
#17161 = CARTESIAN_POINT ( 'NONE',  ( 125.5030348109119558, -6.222761293078241884, -8.102969835052219238 ) ) ;
#17162 = CARTESIAN_POINT ( 'NONE',  ( 125.1059481442453034, -1.833838273341870773, -17.42832698103818956 ) ) ;
#17163 = CARTESIAN_POINT ( 'NONE',  ( 107.3571765045248299, -7.250697342233347165, -19.15521520033831138 ) ) ;
#17164 = CARTESIAN_POINT ( 'NONE',  ( 110.8298327545248299, -6.936859964151250502, -8.388885654883777576 ) ) ;
#17165 = CARTESIAN_POINT ( 'NONE',  ( 108.9545983795247821, -0.7896495226426338832, -9.318865927141430916 ) ) ;
#17166 = CARTESIAN_POINT ( 'NONE',  ( 122.2128881442453263, -1.834011780172310813, -8.268836392978581529 ) ) ;
#17167 = CARTESIAN_POINT ( 'NONE',  ( 123.5743281442453139, -2.084020599724406786, -8.691656652584148546 ) ) ;
#17168 = VERTEX_POINT ( 'NONE', #1885 ) ;
#17169 = CARTESIAN_POINT ( 'NONE',  ( 125.6164881442453094, 0.2603800115204892296, -16.42320221600525088 ) ) ;
#17170 = CARTESIAN_POINT ( 'NONE',  ( 112.1494421295248003, 0.8980012041604618078, -13.39321520033831447 ) ) ;
#17171 = DIRECTION ( 'NONE',  ( 1.000000000000000000, 0.000000000000000000, -0.000000000000000000 ) ) ;
#17172 = CARTESIAN_POINT ( 'NONE',  ( 122.0994348109119443, 0.9020085738987339008, -11.91225656197089222 ) ) ;
#17173 = DIRECTION ( 'NONE',  ( 0.000000000000000000, 0.000000000000000000, 1.000000000000000000 ) ) ;
#17174 = CARTESIAN_POINT ( 'NONE',  ( 119.6708266859119760, -0.6978242514985085743, -9.938897388174442682 ) ) ;
#17175 = CARTESIAN_POINT ( 'NONE',  ( 112.4559014775786494, -9.988377603198976828, -10.36322818467138340 ) ) ;
#17176 = CYLINDRICAL_SURFACE ( 'NONE', #36450, 1.199999999999999067 ) ;
#17177 = CARTESIAN_POINT ( 'NONE',  ( 113.9552233795247815, -1.325403438956436419, -9.854619843455211026 ) ) ;
#17178 = ORIENTED_EDGE ( 'NONE', *, *, #43477, .F. ) ;
#17179 = CARTESIAN_POINT ( 'NONE',  ( 69.69189222814998175, -41.76310523276723785, -24.39321520033831447 ) ) ;
#17180 = CARTESIAN_POINT ( 'NONE',  ( 116.1998614775786507, 0.4262465694468514643, -12.03445270309931736 ) ) ;
#17181 = CARTESIAN_POINT ( 'NONE',  ( 112.6828081442453282, -7.893985811506177619, -18.51759400769804742 ) ) ;
#17182 = CARTESIAN_POINT ( 'NONE',  ( 107.0099108795247815, -1.325403438956436419, -16.93181055722141792 ) ) ;
#17183 = CARTESIAN_POINT ( 'NONE',  ( 107.6349890045248401, -9.868328341294098749, -11.32035403202665869 ) ) ;
#17184 = CARTESIAN_POINT ( 'NONE',  ( 121.4187148109119789, -3.505236298600246325, -18.68346056562440793 ) ) ;
#17185 = CARTESIAN_POINT ( 'NONE',  ( 115.3489614775786407, -0.8288870151387760510, -10.36305467784173118 ) ) ;
#17186 = CARTESIAN_POINT ( 'NONE',  ( 111.6617281442453304, 0.4262465694468514643, -12.03445270309931736 ) ) ;
#17187 = EDGE_LOOP ( 'NONE', ( #29798, #6651 ) ) ;
#17188 = CARTESIAN_POINT ( 'NONE',  ( 125.5597614775786326, -7.894159318335828068, -9.358103419637847864 ) ) ;
#17189 = CARTESIAN_POINT ( 'NONE',  ( 119.5467348109119712, -4.089484607189486809, -7.948022111789456723 ) ) ;
#17190 = DIRECTION ( 'NONE',  ( -1.000000000000000000, 0.000000000000000000, 0.000000000000000000 ) ) ;
#17191 = CARTESIAN_POINT ( 'NONE',  ( 113.1933481442453058, -5.574606645277164318, -18.38911715685844683 ) ) ;
#17192 = ORIENTED_EDGE ( 'NONE', *, *, #29791, .F. ) ;
#17193 = DIRECTION ( 'NONE',  ( 0.9908103287288505534, -0.1352586133457945317, 0.000000000000000000 ) ) ;
#17194 = ORIENTED_EDGE ( 'NONE', *, *, #844, .F. ) ;
#17195 = CARTESIAN_POINT ( 'NONE',  ( 116.7671281442453335, -7.643976991954077427, -18.09477374809248928 ) ) ;
#17196 = CARTESIAN_POINT ( 'NONE',  ( 113.0231681442453180, -10.15424416112533912, -14.75197769757731336 ) ) ;
#17197 = PLANE ( 'NONE',  #24592 ) ;
#17198 = VECTOR ( 'NONE', #37018, 1000.000000000000000 ) ;
#17199 = CARTESIAN_POINT ( 'NONE',  ( 122.3826735609119680, -9.645473719204776586, -14.86997237629376656 ) ) ;
#17200 = VERTEX_POINT ( 'NONE', #36766 ) ;
#17201 = FACE_OUTER_BOUND ( 'NONE', #39289, .T. ) ;
#17202 = CARTESIAN_POINT ( 'NONE',  ( 62.39342502807065216, -3.548534728824127793, -7.543532614991891982 ) ) ;
#17203 = CARTESIAN_POINT ( 'NONE',  ( 113.7468640045248236, -10.62599879583958717, -11.00651665394454604 ) ) ;
#17204 = CARTESIAN_POINT ( 'NONE',  ( 115.1359265045248321, -2.791137627527939813, -8.388885654883754484 ) ) ;
#17205 = CARTESIAN_POINT ( 'NONE',  ( 123.5176014775786228, -0.8288870151387760510, -10.36305467784173118 ) ) ;
#17206 = CARTESIAN_POINT ( 'NONE',  ( 114.7249681442453237, -9.565557343593413364, -10.61323700422348004 ) ) ;
#17207 = CARTESIAN_POINT ( 'NONE',  ( 114.1009748109119784, -5.574606645277172312, -18.38911715685844683 ) ) ;
#17208 = ORIENTED_EDGE ( 'NONE', *, *, #28469, .T. ) ;
#17209 = DIRECTION ( 'NONE',  ( 0.000000000000000000, 1.000000000000000000, 0.000000000000000000 ) ) ;
#17210 = CARTESIAN_POINT ( 'NONE',  ( 116.9940348109119839, -0.1624402480850797581, -16.17319339645315424 ) ) ;
#17211 = EDGE_CURVE ( 'NONE', #30513, #42470, #11766, .T. ) ;
#17212 = CARTESIAN_POINT ( 'NONE',  ( 111.7327388068194836, 0.1168444861213632779, -12.14321520033831625 ) ) ;
#17213 = CARTESIAN_POINT ( 'NONE',  ( 112.0693548109120030, -10.10582367741923093, -14.73954123521778925 ) ) ;
#17215 = CARTESIAN_POINT ( 'NONE',  ( 116.8404719737025630, -1.196538596002799215, -17.02799684832027083 ) ) ;
#17214 = CARTESIAN_POINT ( 'NONE',  ( 65.36445175461375356, -36.61467555475167757, -5.472084168854603803 ) ) ;
#17216 = CIRCLE ( 'NONE', #23023, 5.999999999999997335 ) ;
#17217 = CARTESIAN_POINT ( 'NONE',  ( 125.7866681442452688, -8.899110576539710493, -16.42337572283490132 ) ) ;
#17218 = EDGE_LOOP ( 'NONE', ( #8290, #8184, #33051, #7811, #23040 ) ) ;
#17219 = CARTESIAN_POINT ( 'NONE',  ( 112.0020881442453344, 0.2603800115204892296, -16.42320221600525088 ) ) ;
#17220 = DIRECTION ( 'NONE',  ( 0.000000000000000000, 0.000000000000000000, -1.000000000000000000 ) ) ;
#17221 = CARTESIAN_POINT ( 'NONE',  ( 114.6497546295247929, -4.863998795839590272, -7.631215200338315796 ) ) ;
#17222 = CARTESIAN_POINT ( 'NONE',  ( 126.6942948109119840, -8.899110576539710493, -16.42337572283490132 ) ) ;
#17223 = CARTESIAN_POINT ( 'NONE',  ( 124.0848681442452772, -5.574606645277164318, -18.38911715685844683 ) ) ;
#17224 = CARTESIAN_POINT ( 'NONE',  ( 124.9924948109119924, -5.574606645277164318, -18.38911715685844683 ) ) ;
#17225 = EDGE_CURVE ( 'NONE', #13929, #34025, #27614, .T. ) ;
#17226 = DIRECTION ( 'NONE',  ( -0.8636456077245086016, 0.5040994586965593660, 0.000000000000000000 ) ) ;
#17227 = CARTESIAN_POINT ( 'NONE',  ( 108.2600671295247992, 0.1403307496149613920, -13.39321520033831447 ) ) ;
#17228 = CARTESIAN_POINT ( 'NONE',  ( 120.4317020330015140, -1.172797794773259072, -17.05961127468926719 ) ) ;
#17229 = DIRECTION ( 'NONE',  ( 0.9609149988134837450, -0.1028163501681639419, 0.2570431154366518145 ) ) ;
#17230 = CARTESIAN_POINT ( 'NONE',  ( 112.2289948109119848, -7.643976991954077427, -18.09477374809248928 ) ) ;
#17231 = CARTESIAN_POINT ( 'NONE',  ( 107.5655358795247736, -0.7896495226426338832, -17.46756447353520159 ) ) ;
#17232 = CARTESIAN_POINT ( 'NONE',  ( 109.5102233795247884, -8.938348069036489818, -17.46756447353520159 ) ) ;
#17233 = CARTESIAN_POINT ( 'NONE',  ( 124.5954081442453116, -3.383040157471821630, -19.15922257007629170 ) ) ;
#17234 = CARTESIAN_POINT ( 'NONE',  ( 111.7751814775786556, -2.084020599724406786, -8.691656652584148546 ) ) ;
#17235 = CARTESIAN_POINT ( 'NONE',  ( 114.5108483795247878, -0.7896495226426338832, -9.318865927141425587 ) ) ;
#17236 = CARTESIAN_POINT ( 'NONE',  ( 118.8092881442453290, -9.988377603198976828, -10.36322818467138340 ) ) ;
#17237 = CARTESIAN_POINT ( 'NONE',  ( 115.2355081442453155, -10.30919188438810075, -12.61870101168855918 ) ) ;
#17238 = ORIENTED_EDGE ( 'NONE', *, *, #10709, .F. ) ;
#17239 = AXIS2_PLACEMENT_3D ( 'NONE', #3864, #11618, #8197 ) ;
#17240 = CARTESIAN_POINT ( 'NONE',  ( 113.3068014775786594, -1.833838273342658809, -17.42832698103878286 ) ) ;
#17241 = CARTESIAN_POINT ( 'NONE',  ( 123.9714148109119805, -0.4660016031367893996, -10.09054647747474043 ) ) ;
#17242 = CARTESIAN_POINT ( 'NONE',  ( 113.8173414775786512, 0.2603800115204892296, -16.42320221600525088 ) ) ;
#17243 = CARTESIAN_POINT ( 'NONE',  ( 116.3133148109120043, -2.084020599724406786, -8.691656652584148546 ) ) ;
#17244 = ORIENTED_EDGE ( 'NONE', *, *, #31713, .T. ) ;
#17245 = ADVANCED_FACE ( 'NONE', ( #23108 ), #36544, .F. ) ;
#17246 = CARTESIAN_POINT ( 'NONE',  ( 116.4834948109119779, -7.894159318335828068, -9.358103419637847864 ) ) ;
#17247 = EDGE_CURVE ( 'NONE', #36801, #26421, #22872, .T. ) ;
#17248 = EDGE_CURVE ( 'NONE', #26462, #28048, #22200, .T. ) ;
#17249 = CARTESIAN_POINT ( 'NONE',  ( 117.3343948109119737, -3.383040157471821630, -19.15922257007629170 ) ) ;
#17250 = CARTESIAN_POINT ( 'NONE',  ( 124.5386814775786206, -4.153390946401325223, -8.397313243818185668 ) ) ;
#17251 = CARTESIAN_POINT ( 'NONE',  ( 116.8251712076233417, -1.620372813598558004, -17.49680154955593991 ) ) ;
#17252 = CARTESIAN_POINT ( 'NONE',  ( 112.7050671295247923, -10.62599879583958540, -13.39321520033831447 ) ) ;
#17253 = ORIENTED_EDGE ( 'NONE', *, *, #13986, .T. ) ;
#17254 = DIRECTION ( 'NONE',  ( 0.7871354856660167654, -0.6167752151498625546, -0.002461946824136807422 ) ) ;
#17255 = DIRECTION ( 'NONE',  ( 0.000000000000000000, -0.3818493186865936084, 0.9242245927363024194 ) ) ;
#17256 = VECTOR ( 'NONE', #26809, 1000.000000000000227 ) ;
#17257 = FACE_OUTER_BOUND ( 'NONE', #28819, .T. ) ;
#17258 = CARTESIAN_POINT ( 'NONE',  ( 116.4834948109119779, -1.561330072975668504, -17.79121239304076951 ) ) ;
#17259 = CARTESIAN_POINT ( 'NONE',  ( 70.97035005826802490, 2.261436620216122240, -10.39321520033832158 ) ) ;
#17260 = CARTESIAN_POINT ( 'NONE',  ( 113.5337081442453240, -0.8288870151387760510, -10.36305467784173118 ) ) ;
#17261 = CARTESIAN_POINT ( 'NONE',  ( 111.1245697905468859, 0.6938714319018670640, -12.14321520033833579 ) ) ;
#17262 = CARTESIAN_POINT ( 'NONE',  ( 123.0027181407225783, -1.081026697600530051, -17.18181821144403898 ) ) ;
#17263 = CARTESIAN_POINT ( 'NONE',  ( 117.0806140045248185, 0.1403307496149616695, -15.46607636864997204 ) ) ;
#17264 = CIRCLE ( 'NONE', #25261, 0.3599999999999998201 ) ;
#17265 = CARTESIAN_POINT ( 'NONE',  ( 117.0507614775786465, -10.30919188438810075, -12.61870101168855918 ) ) ;
#17266 = CARTESIAN_POINT ( 'NONE',  ( 136.0599924006030790, -4.157849207606297171, -19.25660148625498991 ) ) ;
#17267 = DIRECTION ( 'NONE',  ( 1.000000000000000000, 0.000000000000000000, 0.000000000000000000 ) ) ;
#17268 = CARTESIAN_POINT ( 'NONE',  ( 116.0829010812576882, -0.01829820670803256055, -12.14321520033834290 ) ) ;
#17269 = CARTESIAN_POINT ( 'NONE',  ( 120.0572748109119772, -6.222761293078241884, -8.102969835052219238 ) ) ;
#17270 = VERTEX_POINT ( 'NONE', #213 ) ;
#17271 = CARTESIAN_POINT ( 'NONE',  ( 135.7778351054754182, -9.571724809176972215, -9.731156920816491862 ) ) ;
#17272 = CARTESIAN_POINT ( 'NONE',  ( 120.1140014775786398, -1.561330072975668504, -17.79121239304076951 ) ) ;
#17273 = CARTESIAN_POINT ( 'NONE',  ( 123.1158699480702552, -6.365377317481717867, -18.95617363400926081 ) ) ;
#17274 = CARTESIAN_POINT ( 'NONE',  ( 114.6115148109119986, -6.222761293078241884, -8.102969835052219238 ) ) ;
#17275 = CARTESIAN_POINT ( 'NONE',  ( 113.4769814775786330, 0.4262465694468514643, -12.03445270309931736 ) ) ;
#17276 = CARTESIAN_POINT ( 'NONE',  ( 109.9269421295247753, 0.8980012041604618078, -13.39321520033831447 ) ) ;
#17277 = ADVANCED_FACE ( 'NONE', ( #35069 ), #3419, .F. ) ;
#17278 = DIRECTION ( 'NONE',  ( 1.000000000000000000, 0.000000000000000000, -0.000000000000000000 ) ) ;
#17279 = CARTESIAN_POINT ( 'NONE',  ( 114.2330358795247776, -0.7896495226426338832, -17.46756447353520159 ) ) ;
#17280 = CARTESIAN_POINT ( 'NONE',  ( 120.4543614775786295, -5.574606645277164318, -18.38911715685844683 ) ) ;
#17281 = CARTESIAN_POINT ( 'NONE',  ( 120.2841814775786276, -10.15424416112533912, -14.75197769757731336 ) ) ;
#17282 = CARTESIAN_POINT ( 'NONE',  ( 67.69189222814998175, -59.27884951796255564, -42.87418841894956500 ) ) ;
#17283 = CARTESIAN_POINT ( 'NONE',  ( 120.1601735609119856, 0.6414057260225851653, -11.69287257290600657 ) ) ;
#17284 = CIRCLE ( 'NONE', #27467, 3.000000000000003997 ) ;
#17285 = CARTESIAN_POINT ( 'NONE',  ( 110.4825671295247815, 0.1403307496149613920, -13.39321520033831447 ) ) ;
#17286 = CARTESIAN_POINT ( 'NONE',  ( 109.2294421295247844, -1.388378309844742642, -16.99368411936019641 ) ) ;
#17287 = CARTESIAN_POINT ( 'NONE',  ( 115.1787814775786387, -9.988377603198976828, -10.36322818467138340 ) ) ;
#17288 = CARTESIAN_POINT ( 'NONE',  ( 115.6325948109119821, 0.2603800115204892296, -16.42320221600525088 ) ) ;
#17289 = DIRECTION ( 'NONE',  ( -1.000000000000000000, 0.000000000000000000, 0.000000000000000000 ) ) ;
#17290 = EDGE_LOOP ( 'NONE', ( #5229, #25537, #4577, #43153 ) ) ;
#17291 = CARTESIAN_POINT ( 'NONE',  ( 113.3507721536727928, 0.3967854368540359999, -10.50530088663809636 ) ) ;
#17292 = VECTOR ( 'NONE', #36928, 1000.000000000000000 ) ;
#17293 = ORIENTED_EDGE ( 'NONE', *, *, #37471, .T. ) ;
#17294 = CARTESIAN_POINT ( 'NONE',  ( 122.8936081442453059, 0.2603800115204892296, -16.42320221600525088 ) ) ;
#17295 = CARTESIAN_POINT ( 'NONE',  ( 113.1933481442453058, -4.089484607189486809, -7.948022111789456723 ) ) ;
#17296 = CARTESIAN_POINT ( 'NONE',  ( 118.2420214775786320, -6.222761293078241884, -8.102969835052219238 ) ) ;
#17297 = SURFACE_STYLE_USAGE ( .BOTH. , #42135 ) ;
#17298 = CARTESIAN_POINT ( 'NONE',  ( 120.2518633482210504, -8.245769691054972483, -17.07760699810916094 ) ) ;
#17299 = CARTESIAN_POINT ( 'NONE',  ( 121.7590748109119687, -7.893985811506177619, -18.51759400769804742 ) ) ;
#17300 = CARTESIAN_POINT ( 'NONE',  ( 116.9940348109119839, -9.988377603198976828, -10.36322818467138340 ) ) ;
#17301 = EDGE_CURVE ( 'NONE', #42470, #10099, #37216, .T. ) ;
#17302 = CARTESIAN_POINT ( 'NONE',  ( 108.7462390045248242, -9.868328341294098749, -11.32035403202665869 ) ) ;
#17303 = CARTESIAN_POINT ( 'NONE',  ( 112.5126281442453120, 0.1319031606808879209, -14.10382304977623669 ) ) ;
#17304 = DIRECTION ( 'NONE',  ( 0.000000000000000000, 0.6004852223388321697, -0.7996358532186279566 ) ) ;
#17305 = ORIENTED_EDGE ( 'NONE', *, *, #8321, .T. ) ;
#17306 = EDGE_CURVE ( 'NONE', #26554, #14451, #24395, .T. ) ;
#17307 = CARTESIAN_POINT ( 'NONE',  ( 117.5613014775786525, 0.9020085738987339008, -11.91225656197089222 ) ) ;
#17308 = DIRECTION ( 'NONE',  ( -0.3445294493088599252, -0.9387755102040817867, 0.000000000000000000 ) ) ;
#17309 = CARTESIAN_POINT ( 'NONE',  ( 115.1220548109119761, -8.166667518702817929, -8.995218007635861213 ) ) ;
#17310 = ORIENTED_EDGE ( 'NONE', *, *, #18985, .T. ) ;
#17311 = CARTESIAN_POINT ( 'NONE',  ( 115.4831921295247952, 0.8980012041604618078, -13.39321520033831447 ) ) ;
#17312 = CARTESIAN_POINT ( 'NONE',  ( 126.1837548109119211, -10.63000616557722466, -14.87417383870573495 ) ) ;
#17314 = CARTESIAN_POINT ( 'NONE',  ( 121.9470836909669913, -27.84333996136784961, -14.15691383771150136 ) ) ;
#17313 = VECTOR ( 'NONE', #1264, 999.9999999999998863 ) ;
#17315 = FACE_OUTER_BOUND ( 'NONE', #43577, .T. ) ;
#17316 = CYLINDRICAL_SURFACE ( 'NONE', #19304, 6.000000000000000888 ) ;
#17317 = CARTESIAN_POINT ( 'NONE',  ( 115.9729548109119861, -3.505236298600246325, -18.68346056562440793 ) ) ;
#17318 = CARTESIAN_POINT ( 'NONE',  ( 111.5519368157052611, -9.055753378951116872, -16.12396441109182632 ) ) ;
#17319 = CARTESIAN_POINT ( 'NONE',  ( 119.0929214775786278, -4.153390946401325223, -8.397313243818185668 ) ) ;
#17320 = DIRECTION ( 'NONE',  ( 0.000000000000000000, -1.000000000000000000, 0.000000000000000000 ) ) ;
#17321 = CARTESIAN_POINT ( 'NONE',  ( 120.6245414775786458, -0.1624402480850797581, -16.17319339645315424 ) ) ;
#17322 = CARTESIAN_POINT ( 'NONE',  ( 122.4521266859119635, -0.06289925094097943703, -9.412459353600674206 ) ) ;
#17323 = CARTESIAN_POINT ( 'NONE',  ( 117.2776681442452968, -5.638512984488999180, -18.83840828888717311 ) ) ;
#17324 = CARTESIAN_POINT ( 'NONE',  ( 115.5191414775786569, -6.222761293078241884, -8.102969835052219238 ) ) ;
#17325 = ORIENTED_EDGE ( 'NONE', *, *, #8562, .F. ) ;
#17326 = CARTESIAN_POINT ( 'NONE',  ( 118.3554748109119998, 0.2603800115204892296, -16.42320221600525088 ) ) ;
#17327 = CARTESIAN_POINT ( 'NONE',  ( 107.2182702545248105, -10.62599879583958717, -15.77991374673208469 ) ) ;
#17328 = DIRECTION ( 'NONE',  ( 1.000000000000000000, 0.000000000000000000, -0.000000000000000000 ) ) ;
#17329 = CARTESIAN_POINT ( 'NONE',  ( 106.2459265045248173, -2.791137627527939813, -8.388885654883777576 ) ) ;
#17330 = FACE_OUTER_BOUND ( 'NONE', #22085, .T. ) ;
#17331 = CARTESIAN_POINT ( 'NONE',  ( 122.5532481442453019, -10.63000616557722466, -14.87417383870573495 ) ) ;
#17332 = ORIENTED_EDGE ( 'NONE', *, *, #33350, .F. ) ;
#17333 = CARTESIAN_POINT ( 'NONE',  ( 118.5867969858783511, -2.378957183258571639, -17.95140958770219086 ) ) ;
#17334 = CARTESIAN_POINT ( 'NONE',  ( 118.8092881442453290, -0.1624402480850797581, -16.17319339645315424 ) ) ;
#17335 = DIRECTION ( 'NONE',  ( -0.2768435750659239414, -0.3568721902840664151, 0.8921882507333142032 ) ) ;
#17336 = CARTESIAN_POINT ( 'NONE',  ( 124.6521348109119884, -7.894159318335843167, -9.358103419637860299 ) ) ;
#17337 = EDGE_CURVE ( 'NONE', #37423, #8341, #41730, .T. ) ;
#17338 = CARTESIAN_POINT ( 'NONE',  ( 122.5532481442453019, -10.63000616557722466, -14.87417383870573495 ) ) ;
#17339 = CARTESIAN_POINT ( 'NONE',  ( 110.0658483795247804, -8.402594152722688392, -16.93181055722141792 ) ) ;
#17340 = DIRECTION ( 'NONE',  ( -0.000000000000000000, -0.9284778069183718952, -0.3713878862591649677 ) ) ;
#17341 = EDGE_LOOP ( 'NONE', ( #10597, #33281, #10027, #28982 ) ) ;
#17342 = CARTESIAN_POINT ( 'NONE',  ( 112.6828081442453282, -7.893985811506177619, -18.51759400769804742 ) ) ;
#17343 = CARTESIAN_POINT ( 'NONE',  ( 112.3424481442453384, -6.344957434206662583, -7.627207830600332805 ) ) ;
#17344 = CARTESIAN_POINT ( 'NONE',  ( 122.1561614775786353, -0.4660016031367893996, -10.09054647747474043 ) ) ;
#17345 = AXIS2_PLACEMENT_3D ( 'NONE', #18604, #32495, #11764 ) ;
#17346 = CARTESIAN_POINT ( 'NONE',  ( 115.7460481442453357, -10.15424416112533912, -14.75197769757731336 ) ) ;
#17347 = CARTESIAN_POINT ( 'NONE',  ( 82.31000308962319423, -13.76004065658516673, -8.143215200338314474 ) ) ;
#17348 = CARTESIAN_POINT ( 'NONE',  ( 119.2063748109119814, -1.561330072975668504, -17.79121239304076951 ) ) ;
#17349 = CARTESIAN_POINT ( 'NONE',  ( 127.7184548109119788, -3.484218720211406772, -13.98160872758045947 ) ) ;
#17350 = CARTESIAN_POINT ( 'NONE',  ( 122.3263414775786373, -3.505236298600246325, -18.68346056562440793 ) ) ;
#17351 = ORIENTED_EDGE ( 'NONE', *, *, #2823, .F. ) ;
#17352 = CARTESIAN_POINT ( 'NONE',  ( -7.923679509334008664, -5.078949698970065540, -17.89321520033831447 ) ) ;
#17353 = ADVANCED_FACE ( 'NONE', ( #28043 ), #3850, .T. ) ;
#17354 = CARTESIAN_POINT ( 'NONE',  ( 117.0507614775786465, -10.30919188438810075, -12.61870101168855918 ) ) ;
#17355 = ADVANCED_FACE ( 'NONE', ( #435 ), #34633, .T. ) ;
#17356 = CARTESIAN_POINT ( 'NONE',  ( 123.6877814775786533, -6.222761293078241884, -8.102969835052219238 ) ) ;
#17357 = ORIENTED_EDGE ( 'NONE', *, *, #29592, .F. ) ;
#17358 = CARTESIAN_POINT ( 'NONE',  ( 121.8270485609119760, -10.36940331770106916, -15.09355782777062061 ) ) ;
#17359 = CARTESIAN_POINT ( 'NONE',  ( 62.94933249576302359, -12.59472958831572775, -10.20703604984677959 ) ) ;
#17360 = CARTESIAN_POINT ( 'NONE',  ( 123.8579614775786126, 0.5811942927096110934, -14.16772938898807510 ) ) ;
#17361 = CARTESIAN_POINT ( 'NONE',  ( 106.5237390045248418, 0.8980012041604421569, -15.77991374673208469 ) ) ;
#17362 = CARTESIAN_POINT ( 'NONE',  ( 118.3554748109119998, -9.565557343593413364, -10.61323700422348004 ) ) ;
#17363 = EDGE_LOOP ( 'NONE', ( #17877, #6872, #18060, #28132 ) ) ;
#17364 = VERTEX_POINT ( 'NONE', #28265 ) ;
#17365 = CARTESIAN_POINT ( 'NONE',  ( 113.4202548109119846, -10.30919188438810075, -12.61870101168855918 ) ) ;
#17366 = CARTESIAN_POINT ( 'NONE',  ( 123.4608748109119745, 0.4262465694468514643, -12.03445270309931736 ) ) ;
#17367 = DIRECTION ( 'NONE',  ( 0.000000000000000000, 0.000000000000000000, 1.000000000000000000 ) ) ;
#17368 = DIRECTION ( 'NONE',  ( 1.000000000000000000, 0.000000000000000000, -0.000000000000000000 ) ) ;
#17369 = CARTESIAN_POINT ( 'NONE',  ( 123.6310548109119765, -5.638512984488999180, -18.83840828888717311 ) ) ;
#17370 = CARTESIAN_POINT ( 'NONE',  ( 31.33087284928346605, -19.31933043625826230, -7.393215200338315363 ) ) ;
#17371 = AXIS2_PLACEMENT_3D ( 'NONE', #206, #14120, #35062 ) ;
#17372 = DIRECTION ( 'NONE',  ( -0.9908103287288505534, 0.1352586133457950590, 0.000000000000000000 ) ) ;
#17373 = CARTESIAN_POINT ( 'NONE',  ( 122.3263414775786373, -6.344957434206665248, -7.627207830600338134 ) ) ;
#17375 = CARTESIAN_POINT ( 'NONE',  ( 121.4754414775786131, -1.833838273342659697, -17.42832698103878286 ) ) ;
#17374 = CARTESIAN_POINT ( 'NONE',  ( 118.6391081442452986, -4.089484607189486809, -7.948022111789456723 ) ) ;
#17376 = CARTESIAN_POINT ( 'NONE',  ( 125.5492214775786550, -6.210324830719740064, -8.151390318758597431 ) ) ;
#17377 = CARTESIAN_POINT ( 'NONE',  ( 115.0653281442453277, -6.344957434206662583, -7.627207830600332805 ) ) ;
#17378 = ORIENTED_EDGE ( 'NONE', *, *, #39291, .F. ) ;
#17379 = CARTESIAN_POINT ( 'NONE',  ( 116.0845533854058829, -0.02059610140724144056, -12.14321520033831625 ) ) ;
#17380 = CARTESIAN_POINT ( 'NONE',  ( 106.9404577545248145, -7.250697342233347165, -7.631215200338321125 ) ) ;
#17381 = CARTESIAN_POINT ( 'NONE',  ( 109.0240515045248202, -6.936859964151250502, -18.39754474579286025 ) ) ;
#17382 = CARTESIAN_POINT ( 'NONE',  ( 106.0375671295248310, -10.62599879583958540, -13.39321520033831447 ) ) ;
#17383 = CARTESIAN_POINT ( 'NONE',  ( 124.7655881442452852, 0.5811942927096110934, -14.16772938898807510 ) ) ;
#17384 = CARTESIAN_POINT ( 'NONE',  ( 125.2761281442453054, 0.4262465694468514643, -12.03445270309931736 ) ) ;
#17385 = ORIENTED_EDGE ( 'NONE', *, *, #1363, .F. ) ;
#17386 = CARTESIAN_POINT ( 'NONE',  ( 123.9714148109119805, -0.4660016031367893996, -10.09054647747474043 ) ) ;
#17387 = CARTESIAN_POINT ( 'NONE',  ( 111.3160046295247838, -4.863998795839590272, -7.631215200338315796 ) ) ;
#17388 = CARTESIAN_POINT ( 'NONE',  ( 70.19189222814998175, -50.76020450571126474, -33.50691401458669105 ) ) ;
#17389 = CARTESIAN_POINT ( 'NONE',  ( 122.1561614775786353, -0.4660016031367893996, -10.09054647747474043 ) ) ;
#17390 =( BOUNDED_SURFACE ( )  B_SPLINE_SURFACE ( 1, 2, ( 
 ( #15928, #5643, #29377, #8631, #22311, #5425, #19342, #43288, #39644, #11601, #43517, #39416, #32775, #22090, #12511, #19564, #4974, #18884, #5196, #4748, #1549, #26182, #29825, #12286, #35977, #40090, #12058, #26407, #18668, #40318, #33227, #15241, #25959, #22531, #36427, #32561, #1328, #43062, #33441, #16150, #2220, #22751, #42841, #19114, #25737, #32999, #1773, #2002, #40547, #30953, #6790, #23446, #23676, #34578, #30054, #12963, #16607, #2452, #34137, #33905, #30728, #37565, #6334, #20699, #33675, #26859, #27089, #2675, #2906, #13632, #26634, #16835, #20476, #9308, #44420, #27318, #9530, #16374, #37332, #41455, #3361, #6559, #20251, #27543, #44651, #20023, #13414, #40772, #43968, #12732, #6103, #10213, #30500, #9765, #30276, #5869, #23216, #13186, #44201, #41234, #41010, #9994, #23903, #37786, #34357, #37095, #24121, #3137, #17060, #44876, #38015, #19792, #41678, #11101, #3788, #34793, #21355, #21130, #17938, #10879, #24776, #39131, #20918, #156, #14293, #35005, #35239, #824, #13848, #4016, #7667, #27763, #31612, #14517, #41894, #3576, #10655, #28656, #35698, #38897, #38667, #14745, #31837, #7218, #7435, #14071, #17280, #45092, #24561, #42562, #38447, #42119, #17488, #38227, #31171, #17713, #31385, #606, #382, #28429, #28211, #42342, #25003, #10436, #11324, #21582, #35469, #4244, #18161, #32057, #24343, #25234, #7898, #21805, #7009, #27989, #4474, #23571, #22032, #33797, #18394, #4916, #19675, #18831, #42791, #32286, #23329, #16498, #36148, #1495, #15190, #12855, #26756, #32723, #1278, #1051, #22477, #14967, #39589, #28879, #5987, #30398, #11774, #25682, #12001, #11552, #43005, #33563, #37215, #36371, #25460, #2340, #29094, #2569, #39363, #44320, #40665, #35926, #8350, #22254, #15417, #8130, #4693, #18613, #13078, #32504, #19912, #5142, #29322, #43235, #26976, #25904, #40896, #16269, #39810, #9649, #8576, #30173, #44091, #9417, #37452, #20369, #13751, #34256, #28105, #34032, #2801, #10333, #9887, #31064, #13301, #3477, #10115, #44992, #44539, #27660, #3031 ),
 ( #54, #16952, #31281, #13968, #23797, #27879, #24018, #41573, #6460, #17612, #24236, #16727, #42010, #17175, #30624, #41793, #27209, #10552, #38341, #38129, #30846, #275, #27436, #10774, #41127, #6900, #37687, #44769, #13529, #41358, #37906, #24450, #34689, #6684, #7118, #21028, #14185, #20811, #34901, #17393, #20594, #34470, #3249, #3690, #20148, #31504, #6225, #29213, #14634, #38790, #21702, #24670, #42232, #28552, #42456, #32399, #7333, #28996, #35590, #32176, #15085, #35814, #7562, #22149, #25354, #36041, #31727, #21476, #4360, #1170, #18280, #42903, #945, #32624, #21252, #38557, #14864, #7794, #35130, #28773, #21921, #11665, #8014, #42681, #4810, #11449, #39248, #498, #43123, #25574, #713, #39478, #18731, #3912, #14410, #11222, #8242, #1390, #4585, #25128, #15304, #17830, #10996, #18057, #18509, #28320, #24897, #35360, #39023, #4135, #31948, #19399, #22592, #26697, #16215, #43574, #9366, #5705, #22816, #23275, #19622, #36492, #33506, #2286, #43349, #30118, #29661, #33286, #26021, #37157, #5478, #22371, #2514, #36709, #8468, #44033, #36267, #12795, #40608, #2061, #39927, #19856, #1830, #16440, #5035, #15985, #29434, #5261, #8687, #12119, #19176, #5933, #9142, #33057, #33743, #30340, #11892, #43805, #25794, #36934, #18949, #15760, #12344, #26242, #39703, #29889, #32839, #1607, #40154, #8916, #12572, #15528, #26476, #40380, #23048, #6848, #26919, #3421, #41299, #6621, #34635, #10273, #13248, #41732, #44938, #10495, #6168, #41071, #10059, #20756, #23962, #17338, #37846, #7064, #40840, #44264, #20534, #27376, #13021, #34414, #41517, #31228, #27603, #3195, #24397, #17119, #31008, #20088, #3634, #45148, #20310, #13909, #38285, #9595, #33974, #34195, #27819, #20975, #13695, #2969, #34848, #17552, #30562, #37630, #24179, #38071, #23511, #9829, #37397, #2741, #16666, #44481, #27150, #23739, #6403, #16897, #30790, #44713, #13474, #25520, #31446, #38501, #21416, #15030, #21867, #42400, #35300, #7956, #18457, #17773, #24839, #7729, #11164, #21641, #28267, #22097, #28045 ) ),
 .UNSPECIFIED., .F., .F., .T. ) 
 B_SPLINE_SURFACE_WITH_KNOTS ( ( 2, 2 ),
 ( 3, 2, 2, 2, 2, 2, 2, 2, 2, 2, 2, 2, 2, 2, 2, 2, 2, 2, 2, 2, 2, 2, 2, 2, 2, 2, 2, 2, 2, 2, 2, 2, 2, 2, 2, 2, 2, 2, 2, 2, 2, 2, 2, 2, 2, 2, 2, 2, 2, 2, 2, 2, 2, 2, 2, 2, 2, 2, 2, 2, 2, 2, 2, 2, 2, 2, 2, 2, 2, 2, 2, 2, 2, 2, 2, 2, 2, 2, 2, 2, 2, 2, 2, 2, 2, 2, 2, 2, 2, 2, 2, 2, 2, 2, 2, 2, 2, 2, 2, 2, 2, 2, 2, 2, 2, 2, 2, 2, 2, 2, 2, 2, 2, 2, 2, 2, 2, 2, 2, 2, 2, 2, 2, 2, 2, 2, 2, 2, 3 ),
 ( 0.000000000000000000, 1.000000000000000000 ),
 ( 0.000000000000000000, 0.007812500000000000000, 0.01562500000000000000, 0.02343750000000000000, 0.03125000000000000000, 0.03906250000000000000, 0.04687500000000000000, 0.05468750000000000000, 0.06250000000000000000, 0.07031250000000000000, 0.07812500000000000000, 0.08593750000000000000, 0.09375000000000000000, 0.1015625000000000000, 0.1093750000000000000, 0.1171875000000000000, 0.1250000000000000000, 0.1328125000000000000, 0.1406250000000000000, 0.1484375000000000000, 0.1562500000000000000, 0.1640625000000000000, 0.1718750000000000000, 0.1796875000000000000, 0.1875000000000000000, 0.1953125000000000000, 0.2031250000000000000, 0.2109375000000000000, 0.2187500000000000000, 0.2265625000000000000, 0.2343750000000000000, 0.2421875000000000000, 0.2500000000000000000, 0.2578125000000000000, 0.2656250000000000000, 0.2734375000000000000, 0.2812500000000000000, 0.2890625000000000000, 0.2968750000000000000, 0.3046875000000000000, 0.3125000000000000000, 0.3203125000000000000, 0.3281250000000000000, 0.3359375000000000000, 0.3437500000000000000, 0.3515625000000000000, 0.3593750000000000000, 0.3671875000000000000, 0.3750000000000000000, 0.3828125000000000000, 0.3906250000000000000, 0.3984375000000000000, 0.4062500000000000000, 0.4140625000000000000, 0.4218750000000000000, 0.4296875000000000000, 0.4375000000000000000, 0.4453125000000000000, 0.4531250000000000000, 0.4609375000000000000, 0.4687500000000000000, 0.4765625000000000000, 0.4843750000000000000, 0.4921875000000000000, 0.5000000000000000000, 0.5078125000000000000, 0.5156250000000000000, 0.5234375000000000000, 0.5312500000000000000, 0.5390625000000000000, 0.5468750000000000000, 0.5546875000000000000, 0.5625000000000000000, 0.5703125000000000000, 0.5781250000000000000, 0.5859375000000000000, 0.5937500000000000000, 0.6015625000000000000, 0.6093750000000000000, 0.6171875000000000000, 0.6250000000000000000, 0.6328125000000000000, 0.6406250000000000000, 0.6484375000000000000, 0.6562500000000000000, 0.6640625000000000000, 0.6718750000000000000, 0.6796875000000000000, 0.6875000000000000000, 0.6953125000000000000, 0.7031250000000000000, 0.7109375000000000000, 0.7187500000000000000, 0.7265625000000000000, 0.7343750000000000000, 0.7421875000000000000, 0.7500000000000000000, 0.7578125000000000000, 0.7656250000000000000, 0.7734375000000000000, 0.7812500000000000000, 0.7890625000000000000, 0.7968750000000000000, 0.8046875000000000000, 0.8125000000000000000, 0.8203125000000000000, 0.8281250000000000000, 0.8359375000000000000, 0.8437500000000000000, 0.8515625000000000000, 0.8593750000000000000, 0.8671875000000000000, 0.8750000000000000000, 0.8828125000000000000, 0.8906250000000000000, 0.8984375000000000000, 0.9062500000000000000, 0.9140625000000000000, 0.9218750000000000000, 0.9296875000000000000, 0.9375000000000000000, 0.9453125000000000000, 0.9531250000000000000, 0.9609375000000000000, 0.9687500000000000000, 0.9765625000000000000, 0.9843750000000000000, 0.9921875000000000000, 1.000000000000000000 ),
 .UNSPECIFIED. ) 
 GEOMETRIC_REPRESENTATION_ITEM ( )  RATIONAL_B_SPLINE_SURFACE ( (
 ( 1.000000000000000000, 0.9238795325112869605, 1.000000000000000000, 0.9238795325112869605, 1.000000000000000000, 0.9238795325112869605, 1.000000000000000000, 0.9238795325112869605, 1.000000000000000000, 0.9238795325112869605, 1.000000000000000000, 0.9238795325112869605, 1.000000000000000000, 0.9238795325112869605, 1.000000000000000000, 0.9238795325112869605, 1.000000000000000000, 0.9238795325112869605, 1.000000000000000000, 0.9238795325112869605, 1.000000000000000000, 0.9238795325112869605, 1.000000000000000000, 0.9238795325112869605, 1.000000000000000000, 0.9238795325112869605, 1.000000000000000000, 0.9238795325112869605, 1.000000000000000000, 0.9238795325112869605, 1.000000000000000000, 0.9238795325112869605, 1.000000000000000000, 0.9238795325112869605, 1.000000000000000000, 0.9238795325112869605, 1.000000000000000000, 0.9238795325112869605, 1.000000000000000000, 0.9238795325112869605, 1.000000000000000000, 0.9238795325112869605, 1.000000000000000000, 0.9238795325112869605, 1.000000000000000000, 0.9238795325112869605, 1.000000000000000000, 0.9238795325112869605, 1.000000000000000000, 0.9238795325112869605, 1.000000000000000000, 0.9238795325112869605, 1.000000000000000000, 0.9238795325112869605, 1.000000000000000000, 0.9238795325112869605, 1.000000000000000000, 0.9238795325112869605, 1.000000000000000000, 0.9238795325112869605, 1.000000000000000000, 0.9238795325112869605, 1.000000000000000000, 0.9238795325112869605, 1.000000000000000000, 0.9238795325112869605, 1.000000000000000000, 0.9238795325112869605, 1.000000000000000000, 0.9238795325112869605, 1.000000000000000000, 0.9238795325112869605, 1.000000000000000000, 0.9238795325112869605, 1.000000000000000000, 0.9238795325112869605, 1.000000000000000000, 0.9238795325112869605, 1.000000000000000000, 0.9238795325112869605, 1.000000000000000000, 0.9238795325112869605, 1.000000000000000000, 0.9238795325112869605, 1.000000000000000000, 0.9238795325112869605, 1.000000000000000000, 0.9238795325112869605, 1.000000000000000000, 0.9238795325112869605, 1.000000000000000000, 0.9238795325112869605, 1.000000000000000000, 0.9238795325112869605, 1.000000000000000000, 0.9238795325112869605, 1.000000000000000000, 0.9238795325112869605, 1.000000000000000000, 0.9238795325112869605, 1.000000000000000000, 0.9238795325112869605, 1.000000000000000000, 0.9238795325112869605, 1.000000000000000000, 0.9238795325112869605, 1.000000000000000000, 0.9238795325112869605, 1.000000000000000000, 0.9238795325112869605, 1.000000000000000000, 0.9238795325112869605, 1.000000000000000000, 0.9238795325112869605, 1.000000000000000000, 0.9238795325112869605, 1.000000000000000000, 0.9238795325112869605, 1.000000000000000000, 0.9238795325112869605, 1.000000000000000000, 0.9238795325112869605, 1.000000000000000000, 0.9238795325112869605, 1.000000000000000000, 0.9238795325112869605, 1.000000000000000000, 0.9238795325112869605, 1.000000000000000000, 0.9238795325112869605, 1.000000000000000000, 0.9238795325112869605, 1.000000000000000000, 0.9238795325112869605, 1.000000000000000000, 0.9238795325112869605, 1.000000000000000000, 0.9238795325112869605, 1.000000000000000000, 0.9238795325112869605, 1.000000000000000000, 0.9238795325112869605, 1.000000000000000000, 0.9238795325112869605, 1.000000000000000000, 0.9238795325112869605, 1.000000000000000000, 0.9238795325112869605, 1.000000000000000000, 0.9238795325112869605, 1.000000000000000000, 0.9238795325112869605, 1.000000000000000000, 0.9238795325112869605, 1.000000000000000000, 0.9238795325112869605, 1.000000000000000000, 0.9238795325112869605, 1.000000000000000000, 0.9238795325112869605, 1.000000000000000000, 0.9238795325112869605, 1.000000000000000000, 0.9238795325112869605, 1.000000000000000000, 0.9238795325112869605, 1.000000000000000000, 0.9238795325112869605, 1.000000000000000000, 0.9238795325112869605, 1.000000000000000000, 0.9238795325112869605, 1.000000000000000000, 0.9238795325112869605, 1.000000000000000000, 0.9238795325112869605, 1.000000000000000000, 0.9238795325112869605, 1.000000000000000000, 0.9238795325112869605, 1.000000000000000000, 0.9238795325112869605, 1.000000000000000000, 0.9238795325112869605, 1.000000000000000000, 0.9238795325112869605, 1.000000000000000000, 0.9238795325112869605, 1.000000000000000000, 0.9238795325112869605, 1.000000000000000000, 0.9238795325112869605, 1.000000000000000000, 0.9238795325112869605, 1.000000000000000000, 0.9238795325112869605, 1.000000000000000000, 0.9238795325112869605, 1.000000000000000000, 0.9238795325112869605, 1.000000000000000000, 0.9238795325112869605, 1.000000000000000000, 0.9238795325112869605, 1.000000000000000000, 0.9238795325112869605, 1.000000000000000000, 0.9238795325112869605, 1.000000000000000000, 0.9238795325112869605, 1.000000000000000000, 0.9238795325112869605, 1.000000000000000000, 0.9238795325112869605, 1.000000000000000000, 0.9238795325112869605, 1.000000000000000000, 0.9238795325112869605, 1.000000000000000000, 0.9238795325112869605, 1.000000000000000000, 0.9238795325112869605, 1.000000000000000000, 0.9238795325112869605, 1.000000000000000000, 0.9238795325112869605, 1.000000000000000000, 0.9238795325112869605, 1.000000000000000000, 0.9238795325112869605, 1.000000000000000000, 0.9238795325112869605, 1.000000000000000000, 0.9238795325112869605, 1.000000000000000000, 0.9238795325112869605, 1.000000000000000000, 0.9238795325112869605, 1.000000000000000000, 0.9238795325112869605, 1.000000000000000000, 0.9238795325112869605, 1.000000000000000000, 0.9238795325112869605, 1.000000000000000000, 0.9238795325112869605, 1.000000000000000000, 0.9238795325112869605, 1.000000000000000000, 0.9238795325112869605, 1.000000000000000000, 0.9238795325112869605, 1.000000000000000000, 0.9238795325112869605, 1.000000000000000000, 0.9238795325112869605, 1.000000000000000000),
 ( 1.000000000000000000, 0.9238795325112869605, 1.000000000000000000, 0.9238795325112869605, 1.000000000000000000, 0.9238795325112869605, 1.000000000000000000, 0.9238795325112869605, 1.000000000000000000, 0.9238795325112869605, 1.000000000000000000, 0.9238795325112869605, 1.000000000000000000, 0.9238795325112869605, 1.000000000000000000, 0.9238795325112869605, 1.000000000000000000, 0.9238795325112869605, 1.000000000000000000, 0.9238795325112869605, 1.000000000000000000, 0.9238795325112869605, 1.000000000000000000, 0.9238795325112869605, 1.000000000000000000, 0.9238795325112869605, 1.000000000000000000, 0.9238795325112869605, 1.000000000000000000, 0.9238795325112869605, 1.000000000000000000, 0.9238795325112869605, 1.000000000000000000, 0.9238795325112869605, 1.000000000000000000, 0.9238795325112869605, 1.000000000000000000, 0.9238795325112869605, 1.000000000000000000, 0.9238795325112869605, 1.000000000000000000, 0.9238795325112869605, 1.000000000000000000, 0.9238795325112869605, 1.000000000000000000, 0.9238795325112869605, 1.000000000000000000, 0.9238795325112869605, 1.000000000000000000, 0.9238795325112869605, 1.000000000000000000, 0.9238795325112869605, 1.000000000000000000, 0.9238795325112869605, 1.000000000000000000, 0.9238795325112869605, 1.000000000000000000, 0.9238795325112869605, 1.000000000000000000, 0.9238795325112869605, 1.000000000000000000, 0.9238795325112869605, 1.000000000000000000, 0.9238795325112869605, 1.000000000000000000, 0.9238795325112869605, 1.000000000000000000, 0.9238795325112869605, 1.000000000000000000, 0.9238795325112869605, 1.000000000000000000, 0.9238795325112869605, 1.000000000000000000, 0.9238795325112869605, 1.000000000000000000, 0.9238795325112869605, 1.000000000000000000, 0.9238795325112869605, 1.000000000000000000, 0.9238795325112869605, 1.000000000000000000, 0.9238795325112869605, 1.000000000000000000, 0.9238795325112869605, 1.000000000000000000, 0.9238795325112869605, 1.000000000000000000, 0.9238795325112869605, 1.000000000000000000, 0.9238795325112869605, 1.000000000000000000, 0.9238795325112869605, 1.000000000000000000, 0.9238795325112869605, 1.000000000000000000, 0.9238795325112869605, 1.000000000000000000, 0.9238795325112869605, 1.000000000000000000, 0.9238795325112869605, 1.000000000000000000, 0.9238795325112869605, 1.000000000000000000, 0.9238795325112869605, 1.000000000000000000, 0.9238795325112869605, 1.000000000000000000, 0.9238795325112869605, 1.000000000000000000, 0.9238795325112869605, 1.000000000000000000, 0.9238795325112869605, 1.000000000000000000, 0.9238795325112869605, 1.000000000000000000, 0.9238795325112869605, 1.000000000000000000, 0.9238795325112869605, 1.000000000000000000, 0.9238795325112869605, 1.000000000000000000, 0.9238795325112869605, 1.000000000000000000, 0.9238795325112869605, 1.000000000000000000, 0.9238795325112869605, 1.000000000000000000, 0.9238795325112869605, 1.000000000000000000, 0.9238795325112869605, 1.000000000000000000, 0.9238795325112869605, 1.000000000000000000, 0.9238795325112869605, 1.000000000000000000, 0.9238795325112869605, 1.000000000000000000, 0.9238795325112869605, 1.000000000000000000, 0.9238795325112869605, 1.000000000000000000, 0.9238795325112869605, 1.000000000000000000, 0.9238795325112869605, 1.000000000000000000, 0.9238795325112869605, 1.000000000000000000, 0.9238795325112869605, 1.000000000000000000, 0.9238795325112869605, 1.000000000000000000, 0.9238795325112869605, 1.000000000000000000, 0.9238795325112869605, 1.000000000000000000, 0.9238795325112869605, 1.000000000000000000, 0.9238795325112869605, 1.000000000000000000, 0.9238795325112869605, 1.000000000000000000, 0.9238795325112869605, 1.000000000000000000, 0.9238795325112869605, 1.000000000000000000, 0.9238795325112869605, 1.000000000000000000, 0.9238795325112869605, 1.000000000000000000, 0.9238795325112869605, 1.000000000000000000, 0.9238795325112869605, 1.000000000000000000, 0.9238795325112869605, 1.000000000000000000, 0.9238795325112869605, 1.000000000000000000, 0.9238795325112869605, 1.000000000000000000, 0.9238795325112869605, 1.000000000000000000, 0.9238795325112869605, 1.000000000000000000, 0.9238795325112869605, 1.000000000000000000, 0.9238795325112869605, 1.000000000000000000, 0.9238795325112869605, 1.000000000000000000, 0.9238795325112869605, 1.000000000000000000, 0.9238795325112869605, 1.000000000000000000, 0.9238795325112869605, 1.000000000000000000, 0.9238795325112869605, 1.000000000000000000, 0.9238795325112869605, 1.000000000000000000, 0.9238795325112869605, 1.000000000000000000, 0.9238795325112869605, 1.000000000000000000, 0.9238795325112869605, 1.000000000000000000, 0.9238795325112869605, 1.000000000000000000, 0.9238795325112869605, 1.000000000000000000, 0.9238795325112869605, 1.000000000000000000, 0.9238795325112869605, 1.000000000000000000, 0.9238795325112869605, 1.000000000000000000, 0.9238795325112869605, 1.000000000000000000, 0.9238795325112869605, 1.000000000000000000, 0.9238795325112869605, 1.000000000000000000, 0.9238795325112869605, 1.000000000000000000, 0.9238795325112869605, 1.000000000000000000, 0.9238795325112869605, 1.000000000000000000, 0.9238795325112869605, 1.000000000000000000, 0.9238795325112869605, 1.000000000000000000, 0.9238795325112869605, 1.000000000000000000, 0.9238795325112869605, 1.000000000000000000, 0.9238795325112869605, 1.000000000000000000, 0.9238795325112869605, 1.000000000000000000, 0.9238795325112869605, 1.000000000000000000, 0.9238795325112869605, 1.000000000000000000, 0.9238795325112869605, 1.000000000000000000, 0.9238795325112869605, 1.000000000000000000, 0.9238795325112869605, 1.000000000000000000, 0.9238795325112869605, 1.000000000000000000, 0.9238795325112869605, 1.000000000000000000, 0.9238795325112869605, 1.000000000000000000, 0.9238795325112869605, 1.000000000000000000) ) ) 
 REPRESENTATION_ITEM ( '' )  SURFACE ( )  );
#17391 = CARTESIAN_POINT ( 'NONE',  ( 125.6732148109119862, 0.5811942927096110934, -14.16772938898807510 ) ) ;
#17392 = LINE ( 'NONE', #37451, #37299 ) ;
#17393 = CARTESIAN_POINT ( 'NONE',  ( 113.9307948109119906, 0.9020085738987339008, -11.91225656197089222 ) ) ;
#17394 = CARTESIAN_POINT ( 'NONE',  ( 116.5944421295247793, 0.8980012041604618078, -13.39321520033831447 ) ) ;
#17395 = CARTESIAN_POINT ( 'NONE',  ( 106.9404577545248145, -7.250697342233347165, -7.631215200338321125 ) ) ;
#17396 = ORIENTED_EDGE ( 'NONE', *, *, #40117, .F. ) ;
#17397 = CARTESIAN_POINT ( 'NONE',  ( 138.2184548109119930, -4.105398160058917334, -19.34506575923121474 ) ) ;
#17398 = CARTESIAN_POINT ( 'NONE',  ( 115.8595014775786609, -7.643976991954077427, -18.09477374809248928 ) ) ;
#17399 = CARTESIAN_POINT ( 'NONE',  ( 113.9875214775786532, -0.4660016031367893996, -10.09054647747474043 ) ) ;
#17400 = CARTESIAN_POINT ( 'NONE',  ( 115.2053796295247849, -4.863998795839590272, -19.15521520033831493 ) ) ;
#17401 = CARTESIAN_POINT ( 'NONE',  ( 108.8851452545248151, -9.868328341294098749, -15.46607636864997204 ) ) ;
#17402 = CARTESIAN_POINT ( 'NONE',  ( 120.7379948109119709, 0.4262465694468514643, -12.03445270309931736 ) ) ;
#17403 = CARTESIAN_POINT ( 'NONE',  ( 117.0507614775786465, 0.1319031606808879209, -14.10382304977623669 ) ) ;
#17404 = CARTESIAN_POINT ( 'NONE',  ( 111.3780948109119890, -5.574606645277164318, -18.38911715685844683 ) ) ;
#17405 = ORIENTED_EDGE ( 'NONE', *, *, #37021, .F. ) ;
#17406 = CARTESIAN_POINT ( 'NONE',  ( 124.2550481442452792, -0.1624402480850797581, -16.17319339645315424 ) ) ;
#17407 = EDGE_CURVE ( 'NONE', #25810, #4027, #21326, .T. ) ;
#17408 = CARTESIAN_POINT ( 'NONE',  ( 73.01241679510815175, -70.92052552613920113, -40.69577108532303811 ) ) ;
#17409 = CARTESIAN_POINT ( 'NONE',  ( 115.8595014775786609, -7.643976991954077427, -18.09477374809248928 ) ) ;
#17410 = ORIENTED_EDGE ( 'NONE', *, *, #20874, .T. ) ;
#17411 = CARTESIAN_POINT ( 'NONE',  ( 126.2184548109119788, 0.08617673920515746266, -14.09731900820182915 ) ) ;
#17412 = ORIENTED_EDGE ( 'NONE', *, *, #14261, .F. ) ;
#17413 = CARTESIAN_POINT ( 'NONE',  ( 120.2274548109119934, -9.859900752359374465, -12.68260735090039404 ) ) ;
#17414 = CARTESIAN_POINT ( 'NONE',  ( 115.0653281442453277, -3.505236298600246325, -18.68346056562440793 ) ) ;
#17415 = CARTESIAN_POINT ( 'NONE',  ( 117.5676200025837090, -2.311015703046737535, -18.04188382666267998 ) ) ;
#17416 = CARTESIAN_POINT ( 'NONE',  ( 123.3550173109119612, -9.289237151508434209, -11.05642687123711276 ) ) ;
#17417 = ORIENTED_EDGE ( 'NONE', *, *, #1622, .T. ) ;
#17418 = DIRECTION ( 'NONE',  ( 0.000000000000000000, 0.000000000000000000, -1.000000000000000000 ) ) ;
#17419 = CARTESIAN_POINT ( 'NONE',  ( 119.7434548109119703, -2.613043214085062793, -8.928554074455437473 ) ) ;
#17420 = CARTESIAN_POINT ( 'NONE',  ( 114.4413952545248350, 0.8980012041604421569, -11.00651665394454071 ) ) ;
#17421 = CARTESIAN_POINT ( 'NONE',  ( 115.2053796295247849, -4.863998795839638234, -8.388885654883775800 ) ) ;
#17422 = CARTESIAN_POINT ( 'NONE',  ( 124.5386814775786206, -4.153390946401325223, -8.397313243818185668 ) ) ;
#17423 = CARTESIAN_POINT ( 'NONE',  ( 118.8660148109119774, 0.1319031606808879209, -14.10382304977623669 ) ) ;
#17424 = CARTESIAN_POINT ( 'NONE',  ( 113.8740681442453138, -9.859900752359374465, -12.68260735090037983 ) ) ;
#17425 = ORIENTED_EDGE ( 'NONE', *, *, #11666, .F. ) ;
#17426 = CARTESIAN_POINT ( 'NONE',  ( 116.0388171295248014, 0.1403307496149613920, -13.39321520033831447 ) ) ;
#17427 = CARTESIAN_POINT ( 'NONE',  ( 116.7671281442453335, -7.643976991954077427, -18.09477374809248928 ) ) ;
#17428 = CARTESIAN_POINT ( 'NONE',  ( 119.7434548109119703, -2.832009000835249868, -18.56602343984135572 ) ) ;
#17429 = CARTESIAN_POINT ( 'NONE',  ( 86.04230958663548279, -25.82262605124143917, -7.893215200338315363 ) ) ;
#17430 = CARTESIAN_POINT ( 'NONE',  ( 116.7619158011494136, -1.149058757900091265, -17.09122335155388939 ) ) ;
#17431 = CARTESIAN_POINT ( 'NONE',  ( 114.4413348109119823, -9.261995988541697145, -16.69588392320189030 ) ) ;
#17432 = ORIENTED_EDGE ( 'NONE', *, *, #6097, .F. ) ;
#17433 = CARTESIAN_POINT ( 'NONE',  ( 115.4056881442453459, -7.893985811506177619, -18.51759400769804742 ) ) ;
#17434 = AXIS2_PLACEMENT_3D ( 'NONE', #24502, #18102, #38386 ) ;
#17435 = DIRECTION ( 'NONE',  ( 0.9970811988817434024, -0.07634843047859724008, 0.000000000000000000 ) ) ;
#17436 = CARTESIAN_POINT ( 'NONE',  ( 111.2465515045248168, -2.477300249445798297, -7.631215200338321125 ) ) ;
#17437 = CARTESIAN_POINT ( 'NONE',  ( 111.8319081442453182, -5.638512984488999180, -18.83840828888717311 ) ) ;
#17438 = CARTESIAN_POINT ( 'NONE',  ( 112.9097148109120070, 0.2603800115204892296, -16.42320221600525088 ) ) ;
#17439 = CARTESIAN_POINT ( 'NONE',  ( 124.6521348109119884, -7.894159318335828068, -9.358103419637847864 ) ) ;
#17440 = FACE_OUTER_BOUND ( 'NONE', #17108, .T. ) ;
#17441 = CARTESIAN_POINT ( 'NONE',  ( 108.6767858795247861, -8.402594152722688392, -9.854619843455216355 ) ) ;
#17442 = DIRECTION ( 'NONE',  ( -0.000000000000000000, -0.9284778069183721172, -0.3713878862591650232 ) ) ;
#17443 = CARTESIAN_POINT ( 'NONE',  ( 109.2294419155992671, -4.095350944532103021, -18.49013907498823528 ) ) ;
#17444 = CARTESIAN_POINT ( 'NONE',  ( 117.6747548109119919, -7.643976991954077427, -18.09477374809248928 ) ) ;
#17445 = CARTESIAN_POINT ( 'NONE',  ( 107.2182702545248105, -10.62599879583958717, -15.77991374673208469 ) ) ;
#17446 = CARTESIAN_POINT ( 'NONE',  ( 108.4684265045247997, -7.250697342233347165, -19.15521520033831138 ) ) ;
#17447 = CARTESIAN_POINT ( 'NONE',  ( 125.2761281442453054, -10.63000616557722466, -14.87417383870573495 ) ) ;
#17448 = CARTESIAN_POINT ( 'NONE',  ( 123.9714148109119805, -0.4660016031367893996, -10.09054647747474043 ) ) ;
#17449 = CARTESIAN_POINT ( 'NONE',  ( 120.4543614775786295, -5.574606645277196293, -18.38911715685844683 ) ) ;
#17450 = CARTESIAN_POINT ( 'NONE',  ( 120.9081748109119872, -5.638512984488999180, -18.83840828888717311 ) ) ;
#17451 = CARTESIAN_POINT ( 'NONE',  ( 115.4056881442453459, -7.893985811506177619, -18.51759400769804742 ) ) ;
#17452 = VERTEX_POINT ( 'NONE', #12856 ) ;
#17453 = CARTESIAN_POINT ( 'NONE',  ( 115.9729548109119861, -3.505236298600246325, -18.68346056562440793 ) ) ;
#17454 = CARTESIAN_POINT ( 'NONE',  ( 124.4252281442452812, -9.261995988541697145, -16.69588392320189030 ) ) ;
#17455 = CARTESIAN_POINT ( 'NONE',  ( 119.6034614775786196, -6.344957434206665248, -7.627207830600338134 ) ) ;
#17456 = CARTESIAN_POINT ( 'NONE',  ( 114.8384214775786489, -10.15424416112533912, -14.75197769757731336 ) ) ;
#17457 = VERTEX_POINT ( 'NONE', #44092 ) ;
#17458 = CARTESIAN_POINT ( 'NONE',  ( 121.1918081442452859, -10.15424416112533912, -14.75197769757731336 ) ) ;
#17459 = CARTESIAN_POINT ( 'NONE',  ( 115.5758681442453053, -1.561330072975668060, -17.79121239304076951 ) ) ;
#17460 = CARTESIAN_POINT ( 'NONE',  ( 136.6626210033597886, 0.7813541710858115108, -12.84505551963111891 ) ) ;
#17461 = CARTESIAN_POINT ( 'NONE',  ( 113.7468640045248236, -10.62599879583958717, -11.00651665394454604 ) ) ;
#17462 = ORIENTED_EDGE ( 'NONE', *, *, #21558, .T. ) ;
#17463 = CARTESIAN_POINT ( 'NONE',  ( 59.90552009294157898, -2.897503654462289191, -8.893215200338314474 ) ) ;
#17464 = DIRECTION ( 'NONE',  ( -0.000000000000000000, -0.9284778069183721172, -0.3713878862591650232 ) ) ;
#17465 = LINE ( 'NONE', #10192, #5806 ) ;
#17466 = VECTOR ( 'NONE', #29613, 1000.000000000000000 ) ;
#17467 = CARTESIAN_POINT ( 'NONE',  ( 113.8740681442453138, 0.5811942927096154232, -14.16772938898807155 ) ) ;
#17468 = CIRCLE ( 'NONE', #14572, 1.999999999999999112 ) ;
#17469 = DIRECTION ( 'NONE',  ( 0.9387755102040806765, -0.3445294493088623122, 0.000000000000000000 ) ) ;
#17470 = CARTESIAN_POINT ( 'NONE',  ( 124.6110072661092119, -9.586796501237937917, -15.06922472696892967 ) ) ;
#17471 = CARTESIAN_POINT ( 'NONE',  ( 63.41276417961783096, -12.69524715595927589, -16.33464570172938224 ) ) ;
#17472 = FACE_OUTER_BOUND ( 'NONE', #6533, .T. ) ;
#17473 = CARTESIAN_POINT ( 'NONE',  ( 115.6220983795247861, -8.402594152722688392, -16.93181055722141792 ) ) ;
#17474 = CARTESIAN_POINT ( 'NONE',  ( 116.4267681442453153, -3.383040157471821630, -19.15922257007629170 ) ) ;
#17475 =( NAMED_UNIT ( * ) PLANE_ANGLE_UNIT ( ) SI_UNIT ( $, .RADIAN. ) );
#17476 = CARTESIAN_POINT ( 'NONE',  ( 87.14323352029596492, -26.75858941326842810, -11.54476601486570964 ) ) ;
#17477 = CARTESIAN_POINT ( 'NONE',  ( 67.69189222814998175, -49.76310523276723785, -40.89321520033831092 ) ) ;
#17478 = CARTESIAN_POINT ( 'NONE',  ( 138.2184548109119930, 0.7334521766912248664, -9.189818643966587430 ) ) ;
#17479 = EDGE_LOOP ( 'NONE', ( #38889, #31959, #24492, #36431, #32736 ) ) ;
#17480 = CARTESIAN_POINT ( 'NONE',  ( 122.0703311593281768, -8.517053830703083861, -17.59134500557228620 ) ) ;
#17481 = CARTESIAN_POINT ( 'NONE',  ( 121.4754414775786131, -8.166667518702819706, -8.995218007635861213 ) ) ;
#17482 = CARTESIAN_POINT ( 'NONE',  ( 89.78938736644981589, -25.99489077589524300, -13.39321520033831625 ) ) ;
#17483 = CARTESIAN_POINT ( 'NONE',  ( 116.5969481442453031, -9.859900752359374465, -12.68260735090039404 ) ) ;
#17484 = EDGE_CURVE ( 'NONE', #41948, #1558, #33741, .T. ) ;
#17485 = CARTESIAN_POINT ( 'NONE',  ( 113.8173414775786512, -9.565557343593413364, -10.61323700422348004 ) ) ;
#17486 = LINE ( 'NONE', #7007, #39493 ) ;
#17487 = CARTESIAN_POINT ( 'NONE',  ( 112.8439733795247832, -8.938348069036489818, -17.46756447353520159 ) ) ;
#17488 = CARTESIAN_POINT ( 'NONE',  ( 120.7947214775786193, -0.8288870151387760510, -10.36305467784173118 ) ) ;
#17489 = CARTESIAN_POINT ( 'NONE',  ( 120.6812681442452941, 0.1319031606808879209, -14.10382304977623669 ) ) ;
#17490 = CARTESIAN_POINT ( 'NONE',  ( 109.2294741910440052, -4.090390389109569647, -7.902357633321886787 ) ) ;
#17491 = CARTESIAN_POINT ( 'NONE',  ( 121.4797829359119987, -4.283928203966213211, -7.183505701512925334 ) ) ;
#17492 = CARTESIAN_POINT ( 'NONE',  ( 109.0935046295247872, -4.863998795839590272, -18.39754474579285315 ) ) ;
#17493 = CARTESIAN_POINT ( 'NONE',  ( 70.19189222814998175, -61.90193818873174791, -37.96356864969668266 ) ) ;
#17494 = CARTESIAN_POINT ( 'NONE',  ( 113.4769814775786330, -10.63000616557722466, -14.87417383870573495 ) ) ;
#17495 = CARTESIAN_POINT ( 'NONE',  ( 116.0864081442453113, -9.988377603198976828, -10.36322818467138340 ) ) ;
#17496 = CARTESIAN_POINT ( 'NONE',  ( 109.0240515045248202, -2.477300249445798297, -7.631215200338321125 ) ) ;
#17497 = LINE ( 'NONE', #27327, #28657 ) ;
#17498 = B_SPLINE_CURVE_WITH_KNOTS ( 'NONE', 3,
 ( #24539, #11302, #13829, #35447, #10417, #24324, #21335, #35220, #42317, #42095, #17693, #34773, #10635, #4222, #41874, #18140, #10859, #38428, #7196, #28634, #42541, #34983, #25211, #28189, #31591, #1920, #15848, #11979, #39340, #1029, #32481, #32921, #26331, #39783, #29073, #32261, #8106, #19267, #8773, #12432, #25881, #15617, #22677, #29743, #29299, #43656, #43439, #1473, #35903, #36347, #42769, #15395, #1255, #36575, #32702, #12203 ),
 .UNSPECIFIED., .F., .F.,
 ( 4, 2, 2, 2, 2, 2, 2, 1, 2, 2, 2, 2, 2, 2, 2, 2, 2, 2, 2, 2, 2, 1, 2, 2, 2, 2, 2, 2, 4 ),
 ( 0.000000000000000000, 0.06249999999995559108, 0.09374999999993996469, 0.1093749999999387573, 0.1249999999999375500, 0.1874999999999329425, 0.2187499999999246436, 0.2343749999999204803, 0.2421874999999237832, 0.2499999999999271139, 0.3124999999999338307, 0.3437499999999332756, 0.3593749999999370504, 0.3749999999999408251, 0.4999999999999611422, 0.5624999999999709122, 0.5937499999999757971, 0.6093749999999760192, 0.6249999999999762412, 0.6874999999999791278, 0.7187499999999805711, 0.7343749999999812372, 0.7421874999999814593, 0.7499999999999816813, 0.8124999999999922284, 0.8437499999999976685, 0.8593750000000004441, 0.8750000000000032196, 1.000000000000000000 ),
 .UNSPECIFIED. ) ;
#17499 = ORIENTED_EDGE ( 'NONE', *, *, #41809, .T. ) ;
#17500 = CARTESIAN_POINT ( 'NONE',  ( 70.19189222814998175, -50.70706315265230302, -33.48565765860439569 ) ) ;
#17501 = CARTESIAN_POINT ( 'NONE',  ( 122.4965214775786251, -10.30919188438810075, -12.61870101168855918 ) ) ;
#17502 = AXIS2_PLACEMENT_3D ( 'NONE', #19371, #12994, #8886 ) ;
#17503 = CARTESIAN_POINT ( 'NONE',  ( 114.4980614775786592, -7.893985811506177619, -18.51759400769804742 ) ) ;
#17504 = CARTESIAN_POINT ( 'NONE',  ( 117.9583881442453048, 0.1319031606808879209, -14.10382304977623669 ) ) ;
#17505 = SHAPE_REPRESENTATION_RELATIONSHIP ( 'NONE' , 'NONE' ,  #38750, #6345 ) ;
#17506 = CARTESIAN_POINT ( 'NONE',  ( 125.3328548109119964, -9.261995988541697145, -16.69588392320189030 ) ) ;
#17507 = CARTESIAN_POINT ( 'NONE',  ( 118.0151148109119816, -10.63000616557722466, -14.87417383870573495 ) ) ;
#17508 = EDGE_CURVE ( 'NONE', #43489, #17518, #27886, .T. ) ;
#17509 = CARTESIAN_POINT ( 'NONE',  ( 108.5378796295247810, -4.863998795839590272, -8.388885654883775800 ) ) ;
#17510 = CARTESIAN_POINT ( 'NONE',  ( 113.1933481442453058, -5.574606645277164318, -18.38911715685844683 ) ) ;
#17511 = DIRECTION ( 'NONE',  ( 1.000000000000000000, 0.000000000000000000, -0.000000000000000000 ) ) ;
#17512 = ORIENTED_EDGE ( 'NONE', *, *, #42420, .F. ) ;
#17513 = CARTESIAN_POINT ( 'NONE',  ( 122.9503348109119827, 0.5811942927096110934, -14.16772938898807510 ) ) ;
#17514 = EDGE_CURVE ( 'NONE', #7179, #10924, #24303, .T. ) ;
#17515 = CARTESIAN_POINT ( 'NONE',  ( 120.9936110609119737, -3.163656168406935087, -18.89861972220014508 ) ) ;
#17516 = EDGE_CURVE ( 'NONE', #12241, #24220, #18437, .T. ) ;
#17517 = CARTESIAN_POINT ( 'NONE',  ( 115.7460481442453357, 0.9020085738987339008, -11.91225656197089222 ) ) ;
#17518 = VERTEX_POINT ( 'NONE', #26977 ) ;
#17519 = CARTESIAN_POINT ( 'NONE',  ( 114.0941296295247867, -4.863998795839590272, -19.15521520033831493 ) ) ;
#17520 = CARTESIAN_POINT ( 'NONE',  ( 123.7445081442452874, -1.561330072975668948, -17.79121239304076951 ) ) ;
#17521 = AXIS2_PLACEMENT_3D ( 'NONE', #10334, #27210, #24237 ) ;
#17522 = CARTESIAN_POINT ( 'NONE',  ( 122.5532481442453019, -10.63000616557722999, -14.87417383870572962 ) ) ;
#17523 = CARTESIAN_POINT ( 'NONE',  ( 112.3424481442453384, -3.505236298600246325, -18.68346056562440793 ) ) ;
#17524 = FACE_OUTER_BOUND ( 'NONE', #13122, .T. ) ;
#17525 = CARTESIAN_POINT ( 'NONE',  ( 120.5678148109119832, -1.833838273342659253, -17.42832698103878286 ) ) ;
#17526 = DIRECTION ( 'NONE',  ( 0.3090169943749414005, 0.8789898214420971412, 0.3631602827797495991 ) ) ;
#17527 = EDGE_CURVE ( 'NONE', #9245, #24192, #13922, .T. ) ;
#17528 = CARTESIAN_POINT ( 'NONE',  ( 121.7590748109119687, -2.084020599724406786, -8.691656652584148546 ) ) ;
#17529 = AXIS2_PLACEMENT_3D ( 'NONE', #6962, #41633, #37968 ) ;
#17530 = CARTESIAN_POINT ( 'NONE',  ( 125.3563494635812958, -11.21126645141554512, -10.32843986934705605 ) ) ;
#17531 = CARTESIAN_POINT ( 'NONE',  ( 120.1707281442453166, -9.565557343593413364, -10.61323700422348004 ) ) ;
#17532 = AXIS2_PLACEMENT_3D ( 'NONE', #25774, #1584, #5456 ) ;
#17533 = EDGE_CURVE ( 'NONE', #3126, #219, #27915, .T. ) ;
#17534 = CARTESIAN_POINT ( 'NONE',  ( 121.6186891859119896, -8.844754642576884152, -8.592115655440050404 ) ) ;
#17535 = CARTESIAN_POINT ( 'NONE',  ( 117.4478481442453131, 0.2603800115204892296, -16.42320221600525088 ) ) ;
#17536 = CARTESIAN_POINT ( 'NONE',  ( 122.0950914740559199, -1.081026697600536046, -17.18181821144402832 ) ) ;
#17537 = EDGE_CURVE ( 'NONE', #37929, #11150, #10173, .T. ) ;
#17538 = EDGE_CURVE ( 'NONE', #16862, #2299, #15028, .T. ) ;
#17539 = CARTESIAN_POINT ( 'NONE',  ( 117.1074881442453233, 0.4262465694468514643, -12.03445270309931736 ) ) ;
#17540 = ORIENTED_EDGE ( 'NONE', *, *, #3588, .F. ) ;
#17541 = CARTESIAN_POINT ( 'NONE',  ( 115.2355081442453155, -10.30919188438810075, -12.61870101168855918 ) ) ;
#17542 = CARTESIAN_POINT ( 'NONE',  ( 107.7738952545248310, 0.8980012041604421569, -11.00651665394454071 ) ) ;
#17543 = DIRECTION ( 'NONE',  ( 0.000000000000000000, -0.3818493186865927203, 0.9242245927363029745 ) ) ;
#17544 = CARTESIAN_POINT ( 'NONE',  ( 114.6497546295247929, -4.863998795839541422, -18.39754474579285315 ) ) ;
#17545 = CARTESIAN_POINT ( 'NONE',  ( 127.9707505455493219, -4.185443562423379227, -15.54568186907484950 ) ) ;
#17546 = CARTESIAN_POINT ( 'NONE',  ( 121.9292548109119849, -1.561330072975668948, -17.79121239304076951 ) ) ;
#17547 = ORIENTED_EDGE ( 'NONE', *, *, #41198, .T. ) ;
#17548 = CARTESIAN_POINT ( 'NONE',  ( 126.9115046738297536, -8.805351640776619249, -9.780119036498003737 ) ) ;
#17549 = CARTESIAN_POINT ( 'NONE',  ( 117.3343948109119737, -6.222761293078241884, -8.102969835052219238 ) ) ;
#17550 = CARTESIAN_POINT ( 'NONE',  ( 116.4642898793805443, -2.191907684172563986, -18.20049396185734025 ) ) ;
#17551 = CARTESIAN_POINT ( 'NONE',  ( 60.06931813437628875, -14.72076136720885309, -18.18301750815651374 ) ) ;
#17552 = CARTESIAN_POINT ( 'NONE',  ( 124.2550481442452792, -9.988377603198980381, -10.36322818467138518 ) ) ;
#17553 = CARTESIAN_POINT ( 'NONE',  ( 113.2606921295247702, -9.868328341294093420, -13.39321520033831447 ) ) ;
#17554 = CARTESIAN_POINT ( 'NONE',  ( 89.19450566478245435, -10.26038732334573744, -13.97729785597371333 ) ) ;
#17555 = ORIENTED_EDGE ( 'NONE', *, *, #25940, .F. ) ;
#17556 = CARTESIAN_POINT ( 'NONE',  ( 113.8740681442453138, 0.5811942927096154232, -14.16772938898807155 ) ) ;
#17557 = CARTESIAN_POINT ( 'NONE',  ( 126.5808414775786446, -9.859900752359378018, -12.68260735090039759 ) ) ;
#17558 = CARTESIAN_POINT ( 'NONE',  ( 123.1205148109119563, -1.834011780172310813, -8.268836392978581529 ) ) ;
#17559 = CIRCLE ( 'NONE', #13917, 2.999999999999999556 ) ;
#17560 = CARTESIAN_POINT ( 'NONE',  ( 118.8660148109119774, 0.1319031606808879209, -14.10382304977623669 ) ) ;
#17561 = CARTESIAN_POINT ( 'NONE',  ( 82.45341866970989031, -31.73112455768813689, -22.62568415223593377 ) ) ;
#17562 = SURFACE_STYLE_FILL_AREA ( #35081 ) ;
#17563 = CARTESIAN_POINT ( 'NONE',  ( 117.5045748109119756, 0.5811942927096110934, -14.16772938898807510 ) ) ;
#17564 = DIRECTION ( 'NONE',  ( 1.000000000000000000, 0.000000000000000000, 0.000000000000000000 ) ) ;
#17565 = FACE_OUTER_BOUND ( 'NONE', #32590, .T. ) ;
#17566 = CARTESIAN_POINT ( 'NONE',  ( 124.5386814775786206, -4.153390946401325223, -8.397313243818185668 ) ) ;
#17567 = VERTEX_POINT ( 'NONE', #35528 ) ;
#17568 = DIRECTION ( 'NONE',  ( 1.000000000000000000, 0.000000000000000000, -0.000000000000000000 ) ) ;
#17569 = AXIS2_PLACEMENT_3D ( 'NONE', #19462, #25417, #39318 ) ;
#17570 = CARTESIAN_POINT ( 'NONE',  ( 118.5823814775786360, -1.834011780172310813, -8.268836392978581529 ) ) ;
#17571 = CARTESIAN_POINT ( 'NONE',  ( 136.2267163768046032, -8.499329989147907938, -17.98615556580662656 ) ) ;
#17572 = EDGE_LOOP ( 'NONE', ( #41000, #5465, #9855 ) ) ;
#17573 = VECTOR ( 'NONE', #17890, 1000.000000000000000 ) ;
#17574 = B_SPLINE_SURFACE_WITH_KNOTS ( 'NONE', 3, 3, ( 
 ( #3070, #41397, #6726, #37952, #20637, #9927 ),
 ( #23841, #6498, #20413, #34297, #34514, #16999 ),
 ( #3292, #30888, #17214, #13567, #44810, #31105 ),
 ( #25941, #1088, #8612, #36187, #4509, #39848 ),
 ( #21617, #25718, #18196, #7703, #25040, #32091 ),
 ( #39399, #38933, #18650, #15678, #12038, #862 ),
 ( #42598, #11811, #22511, #28915, #15002, #21841 ),
 ( #1531, #18432, #42825, #29131, #15224, #29582 ) ),
 .UNSPECIFIED., .F., .F., .F.,
 ( 4, 2, 2, 4 ),
 ( 4, 2, 4 ),
 ( 0.000000000000000000, 0.5000000000000000000, 0.7500000000000000000, 1.000000000000000000 ),
 ( 0.000000000000000000, 0.5000000000000000000, 1.000000000000000000 ),
 .UNSPECIFIED. ) ;
#17575 = CARTESIAN_POINT ( 'NONE',  ( 137.5082292857839548, -1.031900795168988250, -10.16812068200164454 ) ) ;
#17576 = CARTESIAN_POINT ( 'NONE',  ( 123.6877814775786533, -3.383040157471821630, -19.15922257007629170 ) ) ;
#17577 = CARTESIAN_POINT ( 'NONE',  ( 109.0935046295247872, -4.863998795839590272, -7.631215200338315796 ) ) ;
#17578 = CARTESIAN_POINT ( 'NONE',  ( 121.3052614775786111, -7.643976991954077427, -18.09477374809248928 ) ) ;
#17579 = ORIENTED_EDGE ( 'NONE', *, *, #12303, .F. ) ;
#17580 = ORIENTED_EDGE ( 'NONE', *, *, #8493, .F. ) ;
#17581 = CARTESIAN_POINT ( 'NONE',  ( 112.6828081442453282, -7.893985811506177619, -18.51759400769804742 ) ) ;
#17582 = CARTESIAN_POINT ( 'NONE',  ( 90.99708770779186295, -25.99489077589524300, -13.39321520033831447 ) ) ;
#17583 = CARTESIAN_POINT ( 'NONE',  ( 120.6812681442452941, -10.30919188438810075, -12.61870101168855918 ) ) ;
#17584 = EDGE_CURVE ( 'NONE', #40407, #3603, #37365, .T. ) ;
#17585 = DIRECTION ( 'NONE',  ( 1.000000000000000000, 0.000000000000000000, 0.000000000000000000 ) ) ;
#17586 = CARTESIAN_POINT ( 'NONE',  ( 123.1772414775786189, -4.089484607189486809, -7.948022111789456723 ) ) ;
#17587 = DIRECTION ( 'NONE',  ( 0.000000000000000000, 0.9284778069183718952, 0.3713878862591649677 ) ) ;
#17588 = CIRCLE ( 'NONE', #19044, 0.8509999999999994236 ) ;
#17589 = CARTESIAN_POINT ( 'NONE',  ( 71.02242295334774269, -99.02728775972636299, -55.91838671430374319 ) ) ;
#17590 = CARTESIAN_POINT ( 'NONE',  ( 124.3685014775786328, -10.63000616557722466, -14.87417383870573495 ) ) ;
#17592 = CARTESIAN_POINT ( 'NONE',  ( 124.8790414775786246, -8.899110576539710493, -16.42337572283490132 ) ) ;
#17591 = CARTESIAN_POINT ( 'NONE',  ( 120.3976348109119812, -1.834011780172310813, -8.268836392978581529 ) ) ;
#17593 = CARTESIAN_POINT ( 'NONE',  ( 119.8303681442453126, 0.4262465694468514643, -12.03445270309931736 ) ) ;
#17594 = CARTESIAN_POINT ( 'NONE',  ( 125.7194014775786286, -9.814174330883794539, -12.68911139247586739 ) ) ;
#17595 = CARTESIAN_POINT ( 'NONE',  ( 114.7249681442453237, 0.2603800115204892296, -16.42320221600525088 ) ) ;
#17596 = VERTEX_POINT ( 'NONE', #25743 ) ;
#17597 = CARTESIAN_POINT ( 'NONE',  ( 116.0855952810452862, -0.02204510709163942650, -12.14321520033831625 ) ) ;
#17598 = CARTESIAN_POINT ( 'NONE',  ( 113.7468640045248236, 0.1403307496149616695, -15.46607636864997204 ) ) ;
#17599 = AXIS2_PLACEMENT_3D ( 'NONE', #16437, #30335, #6165 ) ;
#17600 = CARTESIAN_POINT ( 'NONE',  ( 108.9545983795247821, -8.402594152722688392, -16.93181055722141792 ) ) ;
#17601 = CARTESIAN_POINT ( 'NONE',  ( 111.9410827545248708, -6.936859964151250502, -8.388885654883777576 ) ) ;
#17602 = CARTESIAN_POINT ( 'NONE',  ( 126.1270281442452870, -10.30919188438810075, -12.61870101168855918 ) ) ;
#17603 = CARTESIAN_POINT ( 'NONE',  ( 126.2404814775786264, -0.8288870151387760510, -10.36305467784173118 ) ) ;
#17604 = ORIENTED_EDGE ( 'NONE', *, *, #19256, .T. ) ;
#17605 = CARTESIAN_POINT ( 'NONE',  ( 114.3278814775786429, 0.1319031606808879209, -14.10382304977623669 ) ) ;
#17606 = CARTESIAN_POINT ( 'NONE',  ( 110.6909265045248247, -7.250697342233347165, -19.15521520033831138 ) ) ;
#17607 = CARTESIAN_POINT ( 'NONE',  ( 72.54180985774836188, -57.87148204839928667, -35.62222722694667709 ) ) ;
#17608 = ADVANCED_FACE ( 'NONE', ( #42397 ), #1110, .T. ) ;
#17609 = CARTESIAN_POINT ( 'NONE',  ( 124.1415948109119540, -6.344957434206665248, -7.627207830600338134 ) ) ;
#17610 = CARTESIAN_POINT ( 'NONE',  ( 123.1205148109119563, -1.834011780172310813, -8.268836392978581529 ) ) ;
#17611 = CARTESIAN_POINT ( 'NONE',  ( 119.3930141859119942, -1.409680983675372534, -17.55938974467904856 ) ) ;
#17612 = CARTESIAN_POINT ( 'NONE',  ( 112.2289948109119848, -1.834011780172310813, -8.268836392978581529 ) ) ;
#17613 = CARTESIAN_POINT ( 'NONE',  ( 113.1217858795247935, -0.7896495226426338832, -17.46756447353520159 ) ) ;
#17614 = CARTESIAN_POINT ( 'NONE',  ( 114.9970202545248412, 0.1403307496149616695, -11.32035403202665336 ) ) ;
#17615 = ORIENTED_EDGE ( 'NONE', *, *, #11679, .F. ) ;
#17616 = CARTESIAN_POINT ( 'NONE',  ( 121.4964260444391755, -1.267766418764731728, -16.93314635290706605 ) ) ;
#17617 = CARTESIAN_POINT ( 'NONE',  ( 115.8027748109119841, -8.899110576539710493, -16.42337572283490132 ) ) ;
#17618 = CARTESIAN_POINT ( 'NONE',  ( 114.1577014775786552, -6.344957434206662583, -7.627207830600332805 ) ) ;
#17619 = CARTESIAN_POINT ( 'NONE',  ( 113.5385046295247804, -4.863998795839590272, -7.631215200338315796 ) ) ;
#17620 = CARTESIAN_POINT ( 'NONE',  ( 105.0652233795248378, -1.325403438956436419, -9.854619843455211026 ) ) ;
#17621 = CARTESIAN_POINT ( 'NONE',  ( 122.3263414775786373, -3.505236298600246325, -18.68346056562440793 ) ) ;
#17622 = CARTESIAN_POINT ( 'NONE',  ( 120.2274548109119934, -9.859900752359378018, -12.68260735090039759 ) ) ;
#17623 = CARTESIAN_POINT ( 'NONE',  ( 125.6164881442453094, 0.2603800115204892296, -16.42320221600525088 ) ) ;
#17624 = ORIENTED_EDGE ( 'NONE', *, *, #35047, .F. ) ;
#17625 = CARTESIAN_POINT ( 'NONE',  ( 120.9241579359119925, -4.360204210389833968, -8.000047426360245240 ) ) ;
#17626 = DIRECTION ( 'NONE',  ( 0.000000000000000000, -0.3818493186865897226, 0.9242245927363041957 ) ) ;
#17627 = CARTESIAN_POINT ( 'NONE',  ( 112.9097148109120070, -9.565557343593413364, -10.61323700422348004 ) ) ;
#17628 = VERTEX_POINT ( 'NONE', #4070 ) ;
#17629 = CARTESIAN_POINT ( 'NONE',  ( 125.4584548109119737, -13.11073630560948722, -15.94021774473354114 ) ) ;
#17630 = CARTESIAN_POINT ( 'NONE',  ( 109.7185827545247889, -6.936859964151250502, -8.388885654883777576 ) ) ;
#17631 = AXIS2_PLACEMENT_3D ( 'NONE', #21863, #35758, #33548 ) ;
#17632 = ORIENTED_EDGE ( 'NONE', *, *, #30026, .T. ) ;
#17633 = CARTESIAN_POINT ( 'NONE',  ( 117.0507614775786465, 0.1319031606808879209, -14.10382304977623669 ) ) ;
#17634 = CARTESIAN_POINT ( 'NONE',  ( 114.1577014775786552, -3.505236298600246325, -18.68346056562440793 ) ) ;
#17635 = CARTESIAN_POINT ( 'NONE',  ( 121.9470836909669913, -27.84333996136784961, -14.15691383771150136 ) ) ;
#17636 = CARTESIAN_POINT ( 'NONE',  ( 123.2855641859119942, -0.8832429491016019485, -18.19431474523657855 ) ) ;
#17637 = ORIENTED_EDGE ( 'NONE', *, *, #30147, .T. ) ;
#17638 = CYLINDRICAL_SURFACE ( 'NONE', #21549, 1.499999999999998002 ) ;
#17639 = CARTESIAN_POINT ( 'NONE',  ( 124.7472578386042272, -0.1571248981867441608, -7.198489643910104263 ) ) ;
#17640 = CARTESIAN_POINT ( 'NONE',  ( 115.0664733795247798, -8.938348069036489818, -17.46756447353520159 ) ) ;
#17641 = CARTESIAN_POINT ( 'NONE',  ( 113.7038881442453402, -3.383040157471821630, -19.15922257007629170 ) ) ;
#17642 = CARTESIAN_POINT ( 'NONE',  ( 122.3830681442452857, -1.833838273342659697, -17.42832698103878286 ) ) ;
#17643 =( BOUNDED_SURFACE ( )  B_SPLINE_SURFACE ( 1, 2, ( 
 ( #28843, #28390, #7181, #11064, #29060, #24966, #38862, #42755, #21994, #7865, #17678, #11518, #35433, #4654, #4207, #32467, #1243, #784, #28619, #42529, #11289, #21771, #21091, #31576, #11736, #25648, #344, #14257, #25197, #22888, #26543, #8538, #5773, #5552, #4882, #40454, #16287, #32905, #33131, #44107, #39552, #22439, #26087, #11964, #43641, #43422, #40224, #1901, #15830, #30189, #43198, #36332, #36559, #12187, #12415, #23125, #36111, #26315, #29960, #18799, #8757, #36781, #19017, #25863, #1680, #19693, #12874, #16054, #29727, #37002, #8988, #29506, #19470, #5102, #8314, #22214, #15602, #33580, #39991, #19250, #39767, #15379, #32688, #22662, #5333, #33352, #2125, #43876, #12647, #9216, #2356, #1458, #29284, #41143, #10129, #27225, #13543, #9667, #37230, #44785, #16744, #27675, #19927, #33814, #26773, #40682, #44334, #3264, #9434, #13321, #30862, #9902, #2584, #6005, #20612, #45006, #44555, #6474, #31080, #34272, #2815, #20386, #23585, #23347, #30414, #23815, #16515, #37703, #27451, #30638, #6241, #13094, #3045, #16970, #34486, #41374, #24033, #37924, #17189, #6701, #40913, #26993, #13766, #37469, #41590, #20164, #34047, #1594, #16200, #22800, #26906, #29421, #43335, #22358, #40826, #39912, #5919, #36252, #36695, #36919, #5464, #15514, #5019, #40594, #33729, #8902, #19384, #33273, #23031, #33043, #2500, #19162, #18936, #40364, #32823, #12104, #30103, #44019, #29646, #26008, #8674, #30323, #36478, #15744, #5689, #9352, #9127, #22577, #19608, #1817, #19841, #5245, #16427, #12780, #43560, #12329, #40138, #15971, #33492, #26229, #2047, #44250, #29874, #37145, #13007, #43790, #2270, #23262, #12555, #26461, #26682, #12434, #36799, #32923, #22906, #29745, #5120, #29301, #15850, #26333, #25662, #32704, #15619, #19036, #29525, #36126, #29976, #35905, #4670, #12205, #11753, #1699, #15168, #5353, #11981, #43441, #1257, #26103, #4895, #9009, #43658, #25883, #5567, #33148, #40010, #1475, #42986, #8775, #39785, #22679, #36577, #19269, #18812, #22009, #19489, #1922, #40240 ),
 ( #39567, #33371, #2141, #16072, #43893, #12662, #39342, #29075, #8331, #8554, #22230, #18592, #8108, #32483, #15397, #43214, #22455, #36349, #16304, #44126, #16534, #30431, #34290, #30205, #3063, #27015, #37720, #33598, #13341, #44350, #16990, #27245, #37945, #2374, #23368, #37487, #30881, #23602, #44801, #20181, #34506, #23143, #26560, #6261, #12891, #3284, #23834, #6491, #13560, #9920, #16761, #20629, #27470, #41390, #13110, #31099, #10143, #2602, #24052, #20405, #6718, #17206, #34066, #45024, #40473, #2832, #40932, #9234, #37023, #26789, #19945, #30658, #44576, #41159, #37249, #5793, #19712, #40698, #9454, #6022, #33833, #9685, #24931, #31541, #21283, #20844, #35169, #24488, #28586, #18092, #310, #11256, #7596, #24703, #25164, #21511, #38376, #35398, #4174, #90, #31985, #14224, #3946, #27918, #39062, #7370, #24274, #4402, #10808, #748, #17868, #21738, #10366, #13782, #38593, #34723, #35627, #11032, #38828, #14672, #42267, #31765, #7832, #42496, #18319, #28139, #32210, #27694, #34937, #41611, #38162, #6938, #3506, #537, #17423, #31315, #14448, #3724, #14002, #41828, #10588, #7148, #28354, #21059, #17644, #42048, #36747, #42719, #11486, #18986, #18543, #39735, #21960, #12154, #18768, #8504, #8055, #22408, #11702, #15795, #5300, #32657, #43609, #39961, #11930, #12384, #8723, #25613, #22629, #36528, #32435, #19216, #1425, #36301, #15123, #26282, #5069, #25391, #5515, #25828, #39287, #33096, #35848, #1866, #29697, #32874, #29030, #8957, #36078, #19435, #4622, #1644, #1209, #39516, #42940, #8280, #22182, #40190, #43386, #4850, #22856, #984, #14899, #15567, #28810, #26057, #15344, #29253, #43162, #29471, #16020, #23551, #37888, #6664, #26955, #23310, #10097, #23086, #5738, #37195, #5968, #41109, #36967, #9867, #33779, #44518, #40420, #20126, #19892, #23776, #34013, #44751, #9179, #30154, #44301, #37668, #27189, #2549, #33320, #19657, #33544, #2094, #29928, #2323, #16932, #43842, #16478, #2782, #30379, #26512, #12609, #6444, #13510, #13056, #40877, #9630, #16707 ) ),
 .UNSPECIFIED., .F., .F., .F. ) 
 B_SPLINE_SURFACE_WITH_KNOTS ( ( 2, 2 ),
 ( 3, 2, 2, 2, 2, 2, 2, 2, 2, 2, 2, 2, 2, 2, 2, 2, 2, 2, 2, 2, 2, 2, 2, 2, 2, 2, 2, 2, 2, 2, 2, 2, 2, 2, 2, 2, 2, 2, 2, 2, 2, 2, 2, 2, 2, 2, 2, 2, 2, 2, 2, 2, 2, 2, 2, 2, 2, 2, 2, 2, 2, 2, 2, 2, 2, 2, 2, 2, 2, 2, 2, 2, 2, 2, 2, 2, 2, 2, 2, 2, 2, 2, 2, 2, 2, 2, 2, 2, 2, 2, 2, 2, 2, 2, 2, 2, 2, 2, 2, 2, 2, 2, 2, 2, 2, 2, 2, 2, 2, 2, 2, 2, 2, 2, 2, 2, 2, 2, 2, 2, 2, 2, 2, 2, 2, 2, 2, 2, 3 ),
 ( 0.000000000000000000, 1.000000000000000000 ),
 ( 0.000000000000000000, 0.007812500000000000000, 0.01562500000000000000, 0.02343750000000000000, 0.03125000000000000000, 0.03906250000000000000, 0.04687500000000000000, 0.05468750000000000000, 0.06250000000000000000, 0.07031250000000000000, 0.07812500000000000000, 0.08593750000000000000, 0.09375000000000000000, 0.1015625000000000000, 0.1093750000000000000, 0.1171875000000000000, 0.1250000000000000000, 0.1328125000000000000, 0.1406250000000000000, 0.1484375000000000000, 0.1562500000000000000, 0.1640625000000000000, 0.1718750000000000000, 0.1796875000000000000, 0.1875000000000000000, 0.1953125000000000000, 0.2031250000000000000, 0.2109375000000000000, 0.2187500000000000000, 0.2265625000000000000, 0.2343750000000000000, 0.2421875000000000000, 0.2500000000000000000, 0.2578125000000000000, 0.2656250000000000000, 0.2734375000000000000, 0.2812500000000000000, 0.2890625000000000000, 0.2968750000000000000, 0.3046875000000000000, 0.3125000000000000000, 0.3203125000000000000, 0.3281250000000000000, 0.3359375000000000000, 0.3437500000000000000, 0.3515625000000000000, 0.3593750000000000000, 0.3671875000000000000, 0.3750000000000000000, 0.3828125000000000000, 0.3906250000000000000, 0.3984375000000000000, 0.4062500000000000000, 0.4140625000000000000, 0.4218750000000000000, 0.4296875000000000000, 0.4375000000000000000, 0.4453125000000000000, 0.4531250000000000000, 0.4609375000000000000, 0.4687500000000000000, 0.4765625000000000000, 0.4843750000000000000, 0.4921875000000000000, 0.5000000000000000000, 0.5078125000000000000, 0.5156250000000000000, 0.5234375000000000000, 0.5312500000000000000, 0.5390625000000000000, 0.5468750000000000000, 0.5546875000000000000, 0.5625000000000000000, 0.5703125000000000000, 0.5781250000000000000, 0.5859375000000000000, 0.5937500000000000000, 0.6015625000000000000, 0.6093750000000000000, 0.6171875000000000000, 0.6250000000000000000, 0.6328125000000000000, 0.6406250000000000000, 0.6484375000000000000, 0.6562500000000000000, 0.6640625000000000000, 0.6718750000000000000, 0.6796875000000000000, 0.6875000000000000000, 0.6953125000000000000, 0.7031250000000000000, 0.7109375000000000000, 0.7187500000000000000, 0.7265625000000000000, 0.7343750000000000000, 0.7421875000000000000, 0.7500000000000000000, 0.7578125000000000000, 0.7656250000000000000, 0.7734375000000000000, 0.7812500000000000000, 0.7890625000000000000, 0.7968750000000000000, 0.8046875000000000000, 0.8125000000000000000, 0.8203125000000000000, 0.8281250000000000000, 0.8359375000000000000, 0.8437500000000000000, 0.8515625000000000000, 0.8593750000000000000, 0.8671875000000000000, 0.8750000000000000000, 0.8828125000000000000, 0.8906250000000000000, 0.8984375000000000000, 0.9062500000000000000, 0.9140625000000000000, 0.9218750000000000000, 0.9296875000000000000, 0.9375000000000000000, 0.9453125000000000000, 0.9531250000000000000, 0.9609375000000000000, 0.9687500000000000000, 0.9765625000000000000, 0.9843750000000000000, 0.9921875000000000000, 1.000000000000000000 ),
 .UNSPECIFIED. ) 
 GEOMETRIC_REPRESENTATION_ITEM ( )  RATIONAL_B_SPLINE_SURFACE ( (
 ( 1.000000000000000000, 0.9238795325112869605, 1.000000000000000000, 0.9238795325112869605, 1.000000000000000000, 0.9238795325112869605, 1.000000000000000000, 0.9238795325112869605, 1.000000000000000000, 0.9238795325112869605, 1.000000000000000000, 0.9238795325112869605, 1.000000000000000000, 0.9238795325112869605, 1.000000000000000000, 0.9238795325112869605, 1.000000000000000000, 0.9238795325112869605, 1.000000000000000000, 0.9238795325112869605, 1.000000000000000000, 0.9238795325112869605, 1.000000000000000000, 0.9238795325112869605, 1.000000000000000000, 0.9238795325112869605, 1.000000000000000000, 0.9238795325112869605, 1.000000000000000000, 0.9238795325112869605, 1.000000000000000000, 0.9238795325112869605, 1.000000000000000000, 0.9238795325112869605, 1.000000000000000000, 0.9238795325112869605, 1.000000000000000000, 0.9238795325112869605, 1.000000000000000000, 0.9238795325112869605, 1.000000000000000000, 0.9238795325112869605, 1.000000000000000000, 0.9238795325112869605, 1.000000000000000000, 0.9238795325112869605, 1.000000000000000000, 0.9238795325112869605, 1.000000000000000000, 0.9238795325112869605, 1.000000000000000000, 0.9238795325112869605, 1.000000000000000000, 0.9238795325112869605, 1.000000000000000000, 0.9238795325112869605, 1.000000000000000000, 0.9238795325112869605, 1.000000000000000000, 0.9238795325112869605, 1.000000000000000000, 0.9238795325112869605, 1.000000000000000000, 0.9238795325112869605, 1.000000000000000000, 0.9238795325112869605, 1.000000000000000000, 0.9238795325112869605, 1.000000000000000000, 0.9238795325112869605, 1.000000000000000000, 0.9238795325112869605, 1.000000000000000000, 0.9238795325112869605, 1.000000000000000000, 0.9238795325112869605, 1.000000000000000000, 0.9238795325112869605, 1.000000000000000000, 0.9238795325112869605, 1.000000000000000000, 0.9238795325112869605, 1.000000000000000000, 0.9238795325112869605, 1.000000000000000000, 0.9238795325112869605, 1.000000000000000000, 0.9238795325112869605, 1.000000000000000000, 0.9238795325112869605, 1.000000000000000000, 0.9238795325112869605, 1.000000000000000000, 0.9238795325112869605, 1.000000000000000000, 0.9238795325112869605, 1.000000000000000000, 0.9238795325112869605, 1.000000000000000000, 0.9238795325112869605, 1.000000000000000000, 0.9238795325112869605, 1.000000000000000000, 0.9238795325112869605, 1.000000000000000000, 0.9238795325112869605, 1.000000000000000000, 0.9238795325112869605, 1.000000000000000000, 0.9238795325112869605, 1.000000000000000000, 0.9238795325112869605, 1.000000000000000000, 0.9238795325112869605, 1.000000000000000000, 0.9238795325112869605, 1.000000000000000000, 0.9238795325112869605, 1.000000000000000000, 0.9238795325112869605, 1.000000000000000000, 0.9238795325112869605, 1.000000000000000000, 0.9238795325112869605, 1.000000000000000000, 0.9238795325112869605, 1.000000000000000000, 0.9238795325112869605, 1.000000000000000000, 0.9238795325112869605, 1.000000000000000000, 0.9238795325112869605, 1.000000000000000000, 0.9238795325112869605, 1.000000000000000000, 0.9238795325112869605, 1.000000000000000000, 0.9238795325112869605, 1.000000000000000000, 0.9238795325112869605, 1.000000000000000000, 0.9238795325112869605, 1.000000000000000000, 0.9238795325112869605, 1.000000000000000000, 0.9238795325112869605, 1.000000000000000000, 0.9238795325112869605, 1.000000000000000000, 0.9238795325112869605, 1.000000000000000000, 0.9238795325112869605, 1.000000000000000000, 0.9238795325112869605, 1.000000000000000000, 0.9238795325112869605, 1.000000000000000000, 0.9238795325112869605, 1.000000000000000000, 0.9238795325112869605, 1.000000000000000000, 0.9238795325112869605, 1.000000000000000000, 0.9238795325112869605, 1.000000000000000000, 0.9238795325112869605, 1.000000000000000000, 0.9238795325112869605, 1.000000000000000000, 0.9238795325112869605, 1.000000000000000000, 0.9238795325112869605, 1.000000000000000000, 0.9238795325112869605, 1.000000000000000000, 0.9238795325112869605, 1.000000000000000000, 0.9238795325112869605, 1.000000000000000000, 0.9238795325112869605, 1.000000000000000000, 0.9238795325112869605, 1.000000000000000000, 0.9238795325112869605, 1.000000000000000000, 0.9238795325112869605, 1.000000000000000000, 0.9238795325112869605, 1.000000000000000000, 0.9238795325112869605, 1.000000000000000000, 0.9238795325112869605, 1.000000000000000000, 0.9238795325112869605, 1.000000000000000000, 0.9238795325112869605, 1.000000000000000000, 0.9238795325112869605, 1.000000000000000000, 0.9238795325112869605, 1.000000000000000000, 0.9238795325112869605, 1.000000000000000000, 0.9238795325112869605, 1.000000000000000000, 0.9238795325112869605, 1.000000000000000000, 0.9238795325112869605, 1.000000000000000000, 0.9238795325112869605, 1.000000000000000000, 0.9238795325112869605, 1.000000000000000000, 0.9238795325112869605, 1.000000000000000000, 0.9238795325112869605, 1.000000000000000000, 0.9238795325112869605, 1.000000000000000000, 0.9238795325112869605, 1.000000000000000000, 0.9238795325112869605, 1.000000000000000000, 0.9238795325112869605, 1.000000000000000000, 0.9238795325112869605, 1.000000000000000000, 0.9238795325112869605, 1.000000000000000000, 0.9238795325112869605, 1.000000000000000000, 0.9238795325112869605, 1.000000000000000000, 0.9238795325112869605, 1.000000000000000000, 0.9238795325112869605, 1.000000000000000000, 0.9238795325112869605, 1.000000000000000000, 0.9238795325112869605, 1.000000000000000000, 0.9238795325112869605, 1.000000000000000000, 0.9238795325112869605, 1.000000000000000000, 0.9238795325112869605, 1.000000000000000000, 0.9238795325112869605, 1.000000000000000000, 0.9238795325112869605, 1.000000000000000000, 0.9238795325112869605, 1.000000000000000000, 0.9238795325112869605, 1.000000000000000000, 0.9238795325112869605, 1.000000000000000000),
 ( 1.000000000000000000, 0.9238795325112869605, 1.000000000000000000, 0.9238795325112869605, 1.000000000000000000, 0.9238795325112869605, 1.000000000000000000, 0.9238795325112869605, 1.000000000000000000, 0.9238795325112869605, 1.000000000000000000, 0.9238795325112869605, 1.000000000000000000, 0.9238795325112869605, 1.000000000000000000, 0.9238795325112869605, 1.000000000000000000, 0.9238795325112869605, 1.000000000000000000, 0.9238795325112869605, 1.000000000000000000, 0.9238795325112869605, 1.000000000000000000, 0.9238795325112869605, 1.000000000000000000, 0.9238795325112869605, 1.000000000000000000, 0.9238795325112869605, 1.000000000000000000, 0.9238795325112869605, 1.000000000000000000, 0.9238795325112869605, 1.000000000000000000, 0.9238795325112869605, 1.000000000000000000, 0.9238795325112869605, 1.000000000000000000, 0.9238795325112869605, 1.000000000000000000, 0.9238795325112869605, 1.000000000000000000, 0.9238795325112869605, 1.000000000000000000, 0.9238795325112869605, 1.000000000000000000, 0.9238795325112869605, 1.000000000000000000, 0.9238795325112869605, 1.000000000000000000, 0.9238795325112869605, 1.000000000000000000, 0.9238795325112869605, 1.000000000000000000, 0.9238795325112869605, 1.000000000000000000, 0.9238795325112869605, 1.000000000000000000, 0.9238795325112869605, 1.000000000000000000, 0.9238795325112869605, 1.000000000000000000, 0.9238795325112869605, 1.000000000000000000, 0.9238795325112869605, 1.000000000000000000, 0.9238795325112869605, 1.000000000000000000, 0.9238795325112869605, 1.000000000000000000, 0.9238795325112869605, 1.000000000000000000, 0.9238795325112869605, 1.000000000000000000, 0.9238795325112869605, 1.000000000000000000, 0.9238795325112869605, 1.000000000000000000, 0.9238795325112869605, 1.000000000000000000, 0.9238795325112869605, 1.000000000000000000, 0.9238795325112869605, 1.000000000000000000, 0.9238795325112869605, 1.000000000000000000, 0.9238795325112869605, 1.000000000000000000, 0.9238795325112869605, 1.000000000000000000, 0.9238795325112869605, 1.000000000000000000, 0.9238795325112869605, 1.000000000000000000, 0.9238795325112869605, 1.000000000000000000, 0.9238795325112869605, 1.000000000000000000, 0.9238795325112869605, 1.000000000000000000, 0.9238795325112869605, 1.000000000000000000, 0.9238795325112869605, 1.000000000000000000, 0.9238795325112869605, 1.000000000000000000, 0.9238795325112869605, 1.000000000000000000, 0.9238795325112869605, 1.000000000000000000, 0.9238795325112869605, 1.000000000000000000, 0.9238795325112869605, 1.000000000000000000, 0.9238795325112869605, 1.000000000000000000, 0.9238795325112869605, 1.000000000000000000, 0.9238795325112869605, 1.000000000000000000, 0.9238795325112869605, 1.000000000000000000, 0.9238795325112869605, 1.000000000000000000, 0.9238795325112869605, 1.000000000000000000, 0.9238795325112869605, 1.000000000000000000, 0.9238795325112869605, 1.000000000000000000, 0.9238795325112869605, 1.000000000000000000, 0.9238795325112869605, 1.000000000000000000, 0.9238795325112869605, 1.000000000000000000, 0.9238795325112869605, 1.000000000000000000, 0.9238795325112869605, 1.000000000000000000, 0.9238795325112869605, 1.000000000000000000, 0.9238795325112869605, 1.000000000000000000, 0.9238795325112869605, 1.000000000000000000, 0.9238795325112869605, 1.000000000000000000, 0.9238795325112869605, 1.000000000000000000, 0.9238795325112869605, 1.000000000000000000, 0.9238795325112869605, 1.000000000000000000, 0.9238795325112869605, 1.000000000000000000, 0.9238795325112869605, 1.000000000000000000, 0.9238795325112869605, 1.000000000000000000, 0.9238795325112869605, 1.000000000000000000, 0.9238795325112869605, 1.000000000000000000, 0.9238795325112869605, 1.000000000000000000, 0.9238795325112869605, 1.000000000000000000, 0.9238795325112869605, 1.000000000000000000, 0.9238795325112869605, 1.000000000000000000, 0.9238795325112869605, 1.000000000000000000, 0.9238795325112869605, 1.000000000000000000, 0.9238795325112869605, 1.000000000000000000, 0.9238795325112869605, 1.000000000000000000, 0.9238795325112869605, 1.000000000000000000, 0.9238795325112869605, 1.000000000000000000, 0.9238795325112869605, 1.000000000000000000, 0.9238795325112869605, 1.000000000000000000, 0.9238795325112869605, 1.000000000000000000, 0.9238795325112869605, 1.000000000000000000, 0.9238795325112869605, 1.000000000000000000, 0.9238795325112869605, 1.000000000000000000, 0.9238795325112869605, 1.000000000000000000, 0.9238795325112869605, 1.000000000000000000, 0.9238795325112869605, 1.000000000000000000, 0.9238795325112869605, 1.000000000000000000, 0.9238795325112869605, 1.000000000000000000, 0.9238795325112869605, 1.000000000000000000, 0.9238795325112869605, 1.000000000000000000, 0.9238795325112869605, 1.000000000000000000, 0.9238795325112869605, 1.000000000000000000, 0.9238795325112869605, 1.000000000000000000, 0.9238795325112869605, 1.000000000000000000, 0.9238795325112869605, 1.000000000000000000, 0.9238795325112869605, 1.000000000000000000, 0.9238795325112869605, 1.000000000000000000, 0.9238795325112869605, 1.000000000000000000, 0.9238795325112869605, 1.000000000000000000, 0.9238795325112869605, 1.000000000000000000, 0.9238795325112869605, 1.000000000000000000, 0.9238795325112869605, 1.000000000000000000, 0.9238795325112869605, 1.000000000000000000, 0.9238795325112869605, 1.000000000000000000, 0.9238795325112869605, 1.000000000000000000, 0.9238795325112869605, 1.000000000000000000, 0.9238795325112869605, 1.000000000000000000, 0.9238795325112869605, 1.000000000000000000, 0.9238795325112869605, 1.000000000000000000, 0.9238795325112869605, 1.000000000000000000, 0.9238795325112869605, 1.000000000000000000, 0.9238795325112869605, 1.000000000000000000, 0.9238795325112869605, 1.000000000000000000, 0.9238795325112869605, 1.000000000000000000) ) ) 
 REPRESENTATION_ITEM ( '' )  SURFACE ( )  );
#17644 = CARTESIAN_POINT ( 'NONE',  ( 119.4332814775786318, -8.899110576539710493, -16.42337572283490132 ) ) ;
#17645 = CARTESIAN_POINT ( 'NONE',  ( 125.4584548109119737, -6.811592368434140177, -19.80118297172327857 ) ) ;
#17646 = VERTEX_POINT ( 'NONE', #32343 ) ;
#17647 = CARTESIAN_POINT ( 'NONE',  ( 116.4834948109119779, -7.894159318335828068, -9.358103419637847864 ) ) ;
#17648 = AXIS2_PLACEMENT_3D ( 'NONE', #8023, #14419, #42241 ) ;
#17649 = CARTESIAN_POINT ( 'NONE',  ( 125.1059481442452750, -1.833838273342660141, -17.42832698103878286 ) ) ;
#17650 = AXIS2_PLACEMENT_3D ( 'NONE', #40425, #19662, #41560 ) ;
#17651 = DIRECTION ( 'NONE',  ( 1.000000000000000000, 0.000000000000000000, -0.000000000000000000 ) ) ;
#17652 = SPHERICAL_SURFACE ( 'NONE', #23990, 6.500000000000000000 ) ;
#17653 = ADVANCED_FACE ( 'NONE', ( #21865 ), #1387, .F. ) ;
#17654 = CARTESIAN_POINT ( 'NONE',  ( 114.3278814775786429, -10.30919188438810075, -12.61870101168855918 ) ) ;
#17655 = ORIENTED_EDGE ( 'NONE', *, *, #23779, .T. ) ;
#17656 = CARTESIAN_POINT ( 'NONE',  ( 116.1431348109119881, -10.30919188438810075, -12.61870101168855918 ) ) ;
#17657 = CARTESIAN_POINT ( 'NONE',  ( 109.5102388068194870, 0.1168444861213632779, -12.14321520033833757 ) ) ;
#17658 = CARTESIAN_POINT ( 'NONE',  ( 112.9134265045247645, -7.250697342233347165, -19.15521520033831138 ) ) ;
#17659 = CARTESIAN_POINT ( 'NONE',  ( 112.3991748109119868, -8.166667518702817929, -8.995218007635859436 ) ) ;
#17660 = CARTESIAN_POINT ( 'NONE',  ( 112.7962614775786676, -3.383040157471821630, -19.15922257007629170 ) ) ;
#17661 = CARTESIAN_POINT ( 'NONE',  ( 122.7801548109119665, -6.222761293078241884, -8.102969835052219238 ) ) ;
#17662 = CARTESIAN_POINT ( 'NONE',  ( 112.0105358795248804, -8.402594152722736354, -9.854619843455244776 ) ) ;
#17663 = CARTESIAN_POINT ( 'NONE',  ( 111.0381921295247878, -9.868328341294093420, -13.39321520033831447 ) ) ;
#17664 = CONICAL_SURFACE ( 'NONE', #32930, 2.999999999999999556, 0.9599310885968830309 ) ;
#17665 = DIRECTION ( 'NONE',  ( -0.5040994586965557023, -0.8636456077245108220, 0.000000000000000000 ) ) ;
#17666 = CARTESIAN_POINT ( 'NONE',  ( 109.2294714807263887, -6.964600658336093097, -18.24697958790709151 ) ) ;
#17667 = CARTESIAN_POINT ( 'NONE',  ( 117.0507614775786465, 0.1319031606808879209, -14.10382304977623669 ) ) ;
#17668 = CARTESIAN_POINT ( 'NONE',  ( 108.1906140045248463, -10.62599879583958717, -11.00651665394454604 ) ) ;
#17669 = CARTESIAN_POINT ( 'NONE',  ( 117.2294421295247844, -10.72535413672978599, -21.89321520033831447 ) ) ;
#17670 = CARTESIAN_POINT ( 'NONE',  ( 110.5520202545248054, -10.62599879583958717, -15.77991374673208469 ) ) ;
#17671 = CARTESIAN_POINT ( 'NONE',  ( 121.9484597424434043, -0.9924539043446216624, -17.29976612834909133 ) ) ;
#17672 = CARTESIAN_POINT ( 'NONE',  ( 111.3780948109119890, -5.574606645277164318, -18.38911715685844683 ) ) ;
#17673 = DIRECTION ( 'NONE',  ( 1.000000000000000000, 0.000000000000000000, -0.000000000000000000 ) ) ;
#17674 = CARTESIAN_POINT ( 'NONE',  ( 124.8790414775786246, -0.4660016031367893996, -10.09054647747474043 ) ) ;
#17675 = CARTESIAN_POINT ( 'NONE',  ( 115.1787814775786387, -9.988377603198976828, -10.36322818467138340 ) ) ;
#17676 = ORIENTED_EDGE ( 'NONE', *, *, #43166, .T. ) ;
#17677 = CARTESIAN_POINT ( 'NONE',  ( 116.5402214775786405, -9.565557343593413364, -10.61323700422348004 ) ) ;
#17678 = CARTESIAN_POINT ( 'NONE',  ( 112.2857214775786474, -4.089484607189486809, -7.948022111789456723 ) ) ;
#17680 = EDGE_CURVE ( 'NONE', #39064, #11127, #17497, .T. ) ;
#17679 = CARTESIAN_POINT ( 'NONE',  ( 116.7104014775786425, -0.4660016031367893996, -10.09054647747474043 ) ) ;
#17681 = CARTESIAN_POINT ( 'NONE',  ( 115.0653281442453277, -3.505236298600246325, -18.68346056562440793 ) ) ;
#17682 = ORIENTED_EDGE ( 'NONE', *, *, #43722, .T. ) ;
#17683 = CARTESIAN_POINT ( 'NONE',  ( 121.4187148109119789, -3.505236298600246325, -18.68346056562440793 ) ) ;
#17684 = CIRCLE ( 'NONE', #43887, 2.000000000000000444 ) ;
#17685 = CARTESIAN_POINT ( 'NONE',  ( 115.4056881442453459, -7.893985811506177619, -18.51759400769804742 ) ) ;
#17686 = DIRECTION ( 'NONE',  ( -1.000000000000000000, 0.000000000000000000, 0.000000000000000000 ) ) ;
#17687 = CARTESIAN_POINT ( 'NONE',  ( 109.5796765045248122, -7.250697342233347165, -19.15521520033831138 ) ) ;
#17688 = CARTESIAN_POINT ( 'NONE',  ( 143.3676850761856940, -69.76310523276724496, -16.89321520033831447 ) ) ;
#17689 = DIRECTION ( 'NONE',  ( 1.000000000000000000, 0.000000000000000000, -0.000000000000000000 ) ) ;
#17690 = CYLINDRICAL_SURFACE ( 'NONE', #36397, 3.000000000000001776 ) ;
#17691 = CIRCLE ( 'NONE', #43186, 0.5000000000000004441 ) ;
#17692 = CARTESIAN_POINT ( 'NONE',  ( 113.6471614775786492, -5.638512984488999180, -18.83840828888717311 ) ) ;
#17693 = CARTESIAN_POINT ( 'NONE',  ( 136.3514896076009109, -10.64081954711834044, -14.04243400364072869 ) ) ;
#17694 = CARTESIAN_POINT ( 'NONE',  ( 113.8740681442453138, -9.859900752359374465, -12.68260735090039404 ) ) ;
#17695 = DIRECTION ( 'NONE',  ( 0.9609149988134843001, -0.1028163501681632064, 0.2570431154366505933 ) ) ;
#17696 = DIRECTION ( 'NONE',  ( -0.8636456077245086016, 0.5040994586965593660, 0.000000000000000000 ) ) ;
#17697 = CARTESIAN_POINT ( 'NONE',  ( 116.3166296295247832, -4.863998795839590272, -8.388885654883775800 ) ) ;
#17698 = CARTESIAN_POINT ( 'NONE',  ( 113.7038881442453402, -6.222761293078241884, -8.102969835052219238 ) ) ;
#17699 = DIRECTION ( 'NONE',  ( 0.000000000000000000, 0.000000000000000000, -1.000000000000000000 ) ) ;
#17701 = CARTESIAN_POINT ( 'NONE',  ( 116.0296814775786345, -8.166667518702817929, -8.995218007635861213 ) ) ;
#17700 = DIRECTION ( 'NONE',  ( 1.000000000000000000, 0.000000000000000000, -0.000000000000000000 ) ) ;
#17702 = CARTESIAN_POINT ( 'NONE',  ( 125.2194014775786286, 0.1319031606808879209, -14.10382304977623669 ) ) ;
#17703 = CARTESIAN_POINT ( 'NONE',  ( 119.8303681442453126, 0.4262465694468514643, -12.03445270309931736 ) ) ;
#17704 = ORIENTED_EDGE ( 'NONE', *, *, #37137, .F. ) ;
#17705 = CARTESIAN_POINT ( 'NONE',  ( 136.5847729262498262, -9.288433219509910188, -9.783805946180876845 ) ) ;
#17706 = CARTESIAN_POINT ( 'NONE',  ( 122.2128881442453263, -1.834011780172310813, -8.268836392978581529 ) ) ;
#17707 = CARTESIAN_POINT ( 'NONE',  ( 115.9693640045247776, 0.1403307496149616695, -15.46607636864997204 ) ) ;
#17708 = CARTESIAN_POINT ( 'NONE',  ( 115.3489614775786407, -0.8288870151387760510, -10.36305467784173118 ) ) ;
#17710 = CARTESIAN_POINT ( 'NONE',  ( 126.2404814775786264, -9.261995988541697145, -16.69588392320189030 ) ) ;
#17709 = AXIS2_PLACEMENT_3D ( 'NONE', #39882, #1789, #33244 ) ;
#17711 = CARTESIAN_POINT ( 'NONE',  ( -7.917624645353497748, -12.21642755857638818, -18.19321520033831519 ) ) ;
#17712 = CARTESIAN_POINT ( 'NONE',  ( 110.6214733795247867, -8.938348069036489818, -17.46756447353520159 ) ) ;
#17713 = CARTESIAN_POINT ( 'NONE',  ( 120.9649014775786355, -6.222761293078241884, -8.102969835052219238 ) ) ;
#17714 = CIRCLE ( 'NONE', #29363, 2.999999999999999556 ) ;
#17715 = CARTESIAN_POINT ( 'NONE',  ( 121.4187148109119789, -3.505236298600246325, -18.68346056562440793 ) ) ;
#17716 = CARTESIAN_POINT ( 'NONE',  ( 115.4451630180080883, 0.7607806665037644134, -14.64321520033834467 ) ) ;
#17717 = DIRECTION ( 'NONE',  ( 0.7202110682883375858, 0.2576522076061144029, -0.6441361323747234469 ) ) ;
#17718 = DIRECTION ( 'NONE',  ( 0.000000000000000000, 0.3818493186865927203, -0.9242245927363029745 ) ) ;
#17719 = CARTESIAN_POINT ( 'NONE',  ( 111.1076452545248259, -9.868328341294098749, -15.46607636864997204 ) ) ;
#17720 = CARTESIAN_POINT ( 'NONE',  ( 116.5060880209376535, 2.200519030075564597, -20.49989231505612963 ) ) ;
#17721 = CARTESIAN_POINT ( 'NONE',  ( 118.6958348109119754, -6.344957434206665248, -7.627207830600338134 ) ) ;
#17722 = CARTESIAN_POINT ( 'NONE',  ( 115.3489614775786407, -9.261995988541697145, -16.69588392320189030 ) ) ;
#17723 = CARTESIAN_POINT ( 'NONE',  ( 112.1494421295248003, 0.8980012041604618078, -13.39321520033831447 ) ) ;
#17724 = CARTESIAN_POINT ( 'NONE',  ( 121.4797829359119987, -5.367793381288652910, -18.78638297431638904 ) ) ;
#17725 = ORIENTED_EDGE ( 'NONE', *, *, #9761, .T. ) ;
#17726 = UNCERTAINTY_MEASURE_WITH_UNIT (LENGTH_MEASURE( 1.000000000000000082E-05 ), #21341, 'distance_accuracy_value', 'NONE');
#17727 = CARTESIAN_POINT ( 'NONE',  ( 83.72016463086879412, -24.14644159042263993, -12.62951656296512937 ) ) ;
#17728 = VECTOR ( 'NONE', #15214, 1000.000000000000000 ) ;
#17729 = CARTESIAN_POINT ( 'NONE',  ( 123.8012348109119642, 0.2603800115204892296, -16.42320221600525088 ) ) ;
#17730 = CARTESIAN_POINT ( 'NONE',  ( 112.9097148109120070, 0.2603800115204892296, -16.42320221600525088 ) ) ;
#17731 = CARTESIAN_POINT ( 'NONE',  ( 122.7801548109119665, -6.222761293078241884, -8.102969835052219238 ) ) ;
#17732 = CARTESIAN_POINT ( 'NONE',  ( 125.7866681442452688, -0.4660016031367893996, -10.09054647747474043 ) ) ;
#17733 = CARTESIAN_POINT ( 'NONE',  ( 121.0216281442452981, -1.561330072975668948, -17.79121239304076951 ) ) ;
#17734 = CARTESIAN_POINT ( 'NONE',  ( 107.0099108795247815, -1.325403438956436419, -16.93181055722141792 ) ) ;
#17735 = CARTESIAN_POINT ( 'NONE',  ( 116.4834948109119779, -7.894159318335828068, -9.358103419637847864 ) ) ;
#17736 = CARTESIAN_POINT ( 'NONE',  ( 126.2184548109119788, -2.495269033102075262, -17.79652296963211455 ) ) ;
#17737 = ORIENTED_EDGE ( 'NONE', *, *, #35637, .F. ) ;
#17738 = B_SPLINE_CURVE_WITH_KNOTS ( 'NONE', 3,
 ( #1829, #37573, #36491, #22370, #16844, #20030, #27326, #43348, #10002, #43573 ),
 .UNSPECIFIED., .F., .F.,
 ( 4, 3, 3, 4 ),
 ( 0.000000000000000000, 0.0001671877560958140072, 0.0003343755126086610133, 0.0006438490228507209303 ),
 .UNSPECIFIED. ) ;
#17739 = CARTESIAN_POINT ( 'NONE',  ( 120.1140014775786398, -1.561330072975668504, -17.79121239304076951 ) ) ;
#17740 = EDGE_CURVE ( 'NONE', #9071, #43660, #35018, .T. ) ;
#17741 = FACE_OUTER_BOUND ( 'NONE', #17090, .T. ) ;
#17742 = CARTESIAN_POINT ( 'NONE',  ( 115.1787814775786387, -9.988377603198976828, -10.36322818467138340 ) ) ;
#17743 = ORIENTED_EDGE ( 'NONE', *, *, #902, .T. ) ;
#17744 = CARTESIAN_POINT ( 'NONE',  ( 114.9970202545248412, -10.62599879583958717, -15.77991374673208469 ) ) ;
#17745 = CARTESIAN_POINT ( 'NONE',  ( 125.3895814775786448, -7.893985811506177619, -18.51759400769804742 ) ) ;
#17746 = CARTESIAN_POINT ( 'NONE',  ( 84.77016061404391678, -25.99489077589524300, -13.39321520033831625 ) ) ;
#17747 = CARTESIAN_POINT ( 'NONE',  ( 116.4267681442453153, -6.222761293078241884, -8.102969835052219238 ) ) ;
#17748 = DIRECTION ( 'NONE',  ( 0.9609149988134837450, -0.1028163501681639419, 0.2570431154366518145 ) ) ;
#17749 = CARTESIAN_POINT ( 'NONE',  ( 121.3052614775786111, -7.643976991954077427, -18.09477374809248928 ) ) ;
#17750 = CARTESIAN_POINT ( 'NONE',  ( 125.4584548109119737, -4.863998795839242995, -13.39321520033831447 ) ) ;
#17751 = CARTESIAN_POINT ( 'NONE',  ( 121.2485348109119769, -8.899110576539710493, -16.42337572283490132 ) ) ;
#17752 = VECTOR ( 'NONE', #39568, 1000.000000000000000 ) ;
#17753 = CARTESIAN_POINT ( 'NONE',  ( 124.6565730087442887, -12.30134031792964855, -10.93904118205077935 ) ) ;
#17754 = CARTESIAN_POINT ( 'NONE',  ( 118.4122014775786340, -9.859900752359374465, -12.68260735090039404 ) ) ;
#17755 = CARTESIAN_POINT ( 'NONE',  ( 121.6881423109119709, -9.959231468620755479, -10.70263013195267199 ) ) ;
#17756 = CARTESIAN_POINT ( 'NONE',  ( 115.5758681442453053, -1.561330072975668060, -17.79121239304076951 ) ) ;
#17757 = DIRECTION ( 'NONE',  ( 0.000000000000000000, -0.3818493186865927203, 0.9242245927363029745 ) ) ;
#17758 = CARTESIAN_POINT ( 'NONE',  ( 121.4187148109119789, -3.505236298600246325, -18.68346056562440793 ) ) ;
#17759 = ORIENTED_EDGE ( 'NONE', *, *, #30102, .F. ) ;
#17760 = CARTESIAN_POINT ( 'NONE',  ( 117.6747548109119919, -1.834011780172310813, -8.268836392978581529 ) ) ;
#17761 = CARTESIAN_POINT ( 'NONE',  ( 115.7610046295247912, -4.863998795839590272, -18.39754474579285315 ) ) ;
#17762 = EDGE_CURVE ( 'NONE', #23958, #34887, #14081, .T. ) ;
#17763 = CARTESIAN_POINT ( 'NONE',  ( 119.7434548109119703, -9.675291321254654520, -19.78473021908636298 ) ) ;
#17764 = DIRECTION ( 'NONE',  ( 0.9609149988134837450, -0.1028163501681639419, 0.2570431154366518145 ) ) ;
#17765 = CARTESIAN_POINT ( 'NONE',  ( 121.6881423109119709, -0.4387604401700521684, -15.73000352943951974 ) ) ;
#17766 = CARTESIAN_POINT ( 'NONE',  ( 123.0637881442452937, -0.4660016031367893996, -10.09054647747474043 ) ) ;
#17767 = VERTEX_POINT ( 'NONE', #24350 ) ;
#17768 = CARTESIAN_POINT ( 'NONE',  ( 126.5010429760479695, -8.432961773280235107, -9.692480226144548183 ) ) ;
#17769 = CARTESIAN_POINT ( 'NONE',  ( 123.0637881442452937, -8.899110576539710493, -16.42337572283490132 ) ) ;
#17770 = EDGE_CURVE ( 'NONE', #22820, #23145, #27999, .T. ) ;
#17771 = CARTESIAN_POINT ( 'NONE',  ( 67.30914723170953096, -55.09414448979863010, -36.13498279219247422 ) ) ;
#17772 = CARTESIAN_POINT ( 'NONE',  ( 60.37455426411234782, -13.41643124914782703, -19.35299115515521606 ) ) ;
#17773 = CARTESIAN_POINT ( 'NONE',  ( 125.8433948109119456, -1.834011780172310813, -8.268836392978581529 ) ) ;
#17774 = CLOSED_SHELL ( 'NONE', ( #19760, #20748, #1365, #11142, #19718, #39380, #35126, #5782, #18026, #36132, #8617, #16853, #31538, #23199, #24289, #13707, #25285, #39956, #3855, #19600, #16713, #1065, #36751, #43152, #38639, #11359, #35324, #32251, #43415, #38918, #1899, #20051, #23856, #38663, #35323, #24491, #4105, #38729, #15016, #27834, #24194, #31145, #17355, #35897, #30354, #39223, #32308, #11556, #7746, #25874, #8940, #19996, #6232, #39519, #41555, #24649, #4717, #38774, #14429, #18905, #29455, #5625, #43816, #21418, #19539, #18676, #16585, #37587, #32249, #39263, #6080, #21769, #23631, #30560, #43180, #16415, #33155, #29527, #24101, #9185, #29848, #9828, #12818, #37294, #3810, #43726, #31054, #28943, #12358, #19985, #30363, #36718, #11420, #22896, #22505, #33630, #10616, #41246, #4087, #10657, #10458, #8383, #38120, #40137, #38126 ) ) ;
#17775 = EDGE_CURVE ( 'NONE', #2572, #4353, #35891, .T. ) ;
#17776 = CARTESIAN_POINT ( 'NONE',  ( 111.8021765045248372, -2.791137627527939813, -8.388885654883777576 ) ) ;
#17777 = FACE_OUTER_BOUND ( 'NONE', #39443, .T. ) ;
#17778 = ORIENTED_EDGE ( 'NONE', *, *, #28630, .F. ) ;
#17779 = CARTESIAN_POINT ( 'NONE',  ( 116.0864081442453113, -9.988377603198976828, -10.36322818467138340 ) ) ;
#17780 = CARTESIAN_POINT ( 'NONE',  ( 125.9001214775786224, -5.574606645277164318, -18.38911715685844683 ) ) ;
#17781 = CARTESIAN_POINT ( 'NONE',  ( 124.9357681442453014, -1.834011780172310813, -8.268836392978581529 ) ) ;
#17782 = CARTESIAN_POINT ( 'NONE',  ( 115.8027748109119841, -8.899110576539710493, -16.42337572283490132 ) ) ;
#17783 = CARTESIAN_POINT ( 'NONE',  ( 126.8396850857575515, -3.206737104985623699, -8.347647502750785264 ) ) ;
#17784 = CARTESIAN_POINT ( 'NONE',  ( 117.9016614775786280, -9.988377603198976828, -10.36322818467138340 ) ) ;
#17785 = CARTESIAN_POINT ( 'NONE',  ( 111.6722681442453222, -0.8658195297461032114, -10.39078908864415496 ) ) ;
#17786 = DIRECTION ( 'NONE',  ( -0.9908103287288504424, 0.1352586133457950590, 0.000000000000000000 ) ) ;
#17787 = CARTESIAN_POINT ( 'NONE',  ( 110.2065776191212763, 0.4261359969231631739, -12.14321520033831625 ) ) ;
#17788 = CARTESIAN_POINT ( 'NONE',  ( 122.8368814775786291, -7.894159318335828068, -9.358103419637847864 ) ) ;
#17789 = ORIENTED_EDGE ( 'NONE', *, *, #17796, .F. ) ;
#17790 = DIRECTION ( 'NONE',  ( -0.000000000000000000, -0.3818493186865893341, 0.9242245927363043068 ) ) ;
#17791 = CARTESIAN_POINT ( 'NONE',  ( 121.4754414775786131, -8.166667518702819706, -8.995218007635861213 ) ) ;
#17792 = CARTESIAN_POINT ( 'NONE',  ( 124.1415948109119540, -3.505236298600246325, -18.68346056562440793 ) ) ;
#17793 = VERTEX_POINT ( 'NONE', #3148 ) ;
#17794 = EDGE_CURVE ( 'NONE', #30249, #35231, #42492, .T. ) ;
#17795 = CARTESIAN_POINT ( 'NONE',  ( 121.1198558961590521, -2.263366209404226392, -18.10533625161308180 ) ) ;
#17796 = EDGE_CURVE ( 'NONE', #24941, #34537, #20928, .T. ) ;
#17797 = EDGE_CURVE ( 'NONE', #41268, #16139, #44683, .T. ) ;
#17798 = CARTESIAN_POINT ( 'NONE',  ( 121.8725281442453223, -3.383040157471821630, -19.15922257007629170 ) ) ;
#17799 = CARTESIAN_POINT ( 'NONE',  ( 105.7597546295248350, -4.863998795839590272, -7.631215200338315796 ) ) ;
#17800 = CARTESIAN_POINT ( 'NONE',  ( 119.0361948109119652, -2.084020599724406786, -8.691656652584148546 ) ) ;
#17801 = CIRCLE ( 'NONE', #35252, 5.999999999999997335 ) ;
#17802 = ORIENTED_EDGE ( 'NONE', *, *, #38102, .F. ) ;
#17803 = CARTESIAN_POINT ( 'NONE',  ( 112.9097148109120070, 0.2603800115204892296, -16.42320221600525088 ) ) ;
#17804 = LINE ( 'NONE', #38759, #41609 ) ;
#17805 = CARTESIAN_POINT ( 'NONE',  ( 112.4201593777725208, -1.267766418764741276, -16.93314635290707315 ) ) ;
#17806 = LINE ( 'NONE', #10968, #38917 ) ;
#17807 = CARTESIAN_POINT ( 'NONE',  ( 125.5597614775786326, -1.561330072975669392, -17.79121239304076951 ) ) ;
#17808 = CARTESIAN_POINT ( 'NONE',  ( 122.7419882662982786, -6.118135741080345191, -18.48796566952144005 ) ) ;
#17809 = CARTESIAN_POINT ( 'NONE',  ( 73.60369002873177635, -5.846784287000932778, -8.143215200338314474 ) ) ;
#17810 = CARTESIAN_POINT ( 'NONE',  ( 124.3117748109119844, -10.30919188438810075, -12.61870101168855918 ) ) ;
#17812 = CARTESIAN_POINT ( 'NONE',  ( 123.2906948109119867, -1.833838273342659697, -17.42832698103878286 ) ) ;
#17811 = CARTESIAN_POINT ( 'NONE',  ( 121.3619881442452879, -4.089484607189486809, -7.948022111789456723 ) ) ;
#17813 = CARTESIAN_POINT ( 'NONE',  ( 120.9649014775786355, -6.222761293078241884, -8.102969835052219238 ) ) ;
#17814 = FACE_OUTER_BOUND ( 'NONE', #2784, .T. ) ;
#17815 = CARTESIAN_POINT ( 'NONE',  ( 115.1787814775786387, -9.988377603198976828, -10.36322818467138340 ) ) ;
#17816 = ORIENTED_EDGE ( 'NONE', *, *, #10663, .F. ) ;
#17817 = CARTESIAN_POINT ( 'NONE',  ( 74.43213512091445239, -36.61236768192972590, -14.39321520033831625 ) ) ;
#17818 = CARTESIAN_POINT ( 'NONE',  ( 114.7886608795247696, -1.325403438956436419, -16.93181055722141792 ) ) ;
#17819 = CARTESIAN_POINT ( 'NONE',  ( 108.4684265045247997, -2.791137627527939813, -8.388885654883777576 ) ) ;
#17820 = CARTESIAN_POINT ( 'NONE',  ( 111.8021765045248372, -2.791137627527939813, -8.388885654883777576 ) ) ;
#17821 = DIRECTION ( 'NONE',  ( 0.9609149988134843001, -0.1028163501681632064, 0.2570431154366505933 ) ) ;
#17822 = CARTESIAN_POINT ( 'NONE',  ( 112.5126281442453120, -10.30919188438810075, -12.61870101168855918 ) ) ;
#17823 = ORIENTED_EDGE ( 'NONE', *, *, #9728, .T. ) ;
#17824 = CARTESIAN_POINT ( 'NONE',  ( 114.8384214775786489, -10.15424416112533912, -14.75197769757731336 ) ) ;
#17825 = CARTESIAN_POINT ( 'NONE',  ( 110.8298327545248299, -2.477300249445798297, -19.15521520033831138 ) ) ;
#17826 = CARTESIAN_POINT ( 'NONE',  ( 121.9859814775786333, -9.565557343593409811, -10.61323700422347649 ) ) ;
#17827 = CARTESIAN_POINT ( 'NONE',  ( 125.0492214775786266, -6.344957434206665248, -7.627207830600338134 ) ) ;
#17828 = CARTESIAN_POINT ( 'NONE',  ( 124.3685014775786328, -10.63000616557722466, -14.87417383870573495 ) ) ;
#17829 = DIRECTION ( 'NONE',  ( -0.2768435750659239414, -0.3568721902840664151, 0.8921882507333142032 ) ) ;
#17830 = CARTESIAN_POINT ( 'NONE',  ( 117.4478481442453131, 0.2603800115204892296, -16.42320221600525088 ) ) ;
#17831 = EDGE_CURVE ( 'NONE', #40625, #29947, #45100, .T. ) ;
#17832 = CARTESIAN_POINT ( 'NONE',  ( 116.3166296295247832, -4.863998795839590272, -19.15521520033831493 ) ) ;
#17833 = CARTESIAN_POINT ( 'NONE',  ( 105.8986608795248401, -8.938348069036489818, -9.318865927141430916 ) ) ;
#17834 = AXIS2_PLACEMENT_3D ( 'NONE', #13885, #26891, #23712 ) ;
#17835 = ORIENTED_EDGE ( 'NONE', *, *, #25861, .F. ) ;
#17836 = DIRECTION ( 'NONE',  ( -1.000000000000000000, 0.000000000000000000, 0.000000000000000000 ) ) ;
#17837 = CARTESIAN_POINT ( 'NONE',  ( 114.8951481442453115, -8.899110576539710493, -16.42337572283490132 ) ) ;
#17838 = CARTESIAN_POINT ( 'NONE',  ( 126.4106614775786284, -6.222761293078241884, -8.102969835052219238 ) ) ;
#17839 = CARTESIAN_POINT ( 'NONE',  ( 116.0388171295248014, -10.62599879583958540, -13.39321520033831447 ) ) ;
#17840 = CARTESIAN_POINT ( 'NONE',  ( 109.0240515045248202, -6.936859964151250502, -18.39754474579286025 ) ) ;
#17841 = CARTESIAN_POINT ( 'NONE',  ( 124.0848681442452772, -5.574606645277164318, -18.38911715685844683 ) ) ;
#17842 = PRODUCT_DEFINITION_CONTEXT ( 'detailed design', #25639, 'design' ) ;
#17843 = CARTESIAN_POINT ( 'NONE',  ( 121.0783548109119749, -9.565557343593413364, -10.61323700422348004 ) ) ;
#17844 = CARTESIAN_POINT ( 'NONE',  ( 112.0588148109119828, -9.859900752359374465, -12.68260735090039404 ) ) ;
#17845 = ORIENTED_EDGE ( 'NONE', *, *, #16681, .T. ) ;
#17846 = CARTESIAN_POINT ( 'NONE',  ( 125.1059481442452750, -1.833838273342660141, -17.42832698103878286 ) ) ;
#17847 = CARTESIAN_POINT ( 'NONE',  ( 75.63675420052337017, -42.57465691284114939, -10.89321520033831447 ) ) ;
#17848 = CARTESIAN_POINT ( 'NONE',  ( 112.5126281442453120, 0.1319031606808879209, -14.10382304977623669 ) ) ;
#17849 = ORIENTED_EDGE ( 'NONE', *, *, #36785, .F. ) ;
#17850 = CARTESIAN_POINT ( 'NONE',  ( 126.4599182912924675, -9.283010264413503521, -15.98057921980140783 ) ) ;
#17851 = EDGE_CURVE ( 'NONE', #2333, #35973, #10889, .T. ) ;
#17852 = CARTESIAN_POINT ( 'NONE',  ( 112.7962614775786676, -3.383040157471821630, -19.15922257007629170 ) ) ;
#17853 = CARTESIAN_POINT ( 'NONE',  ( 112.1494421295248003, -9.868328341294093420, -13.39321520033831447 ) ) ;
#17854 = ORIENTED_EDGE ( 'NONE', *, *, #26771, .T. ) ;
#17855 = EDGE_CURVE ( 'NONE', #15244, #32861, #17714, .T. ) ;
#17856 = CARTESIAN_POINT ( 'NONE',  ( 117.4478481442453131, -9.565557343593413364, -10.61323700422348004 ) ) ;
#17857 = CARTESIAN_POINT ( 'NONE',  ( 115.0086014775786509, -5.574606645277164318, -18.38911715685844683 ) ) ;
#17858 = ADVANCED_FACE ( 'NONE', ( #11786 ), #40153, .T. ) ;
#17859 = CARTESIAN_POINT ( 'NONE',  ( 124.5857744023975471, -9.784663199447079407, -14.29957148619841334 ) ) ;
#17860 = CARTESIAN_POINT ( 'NONE',  ( 116.0506660444391969, -1.267766418764730840, -16.93314635290706605 ) ) ;
#17861 = ORIENTED_EDGE ( 'NONE', *, *, #42030, .F. ) ;
#17862 = CARTESIAN_POINT ( 'NONE',  ( 121.3786053070358832, -1.196538596002817867, -17.02799684832028504 ) ) ;
#17863 = CYLINDRICAL_SURFACE ( 'NONE', #42688, 2.000000000000000444 ) ;
#17864 = AXIS2_PLACEMENT_3D ( 'NONE', #29581, #22069, #11585 ) ;
#17865 = CARTESIAN_POINT ( 'NONE',  ( 110.2047546295247855, -4.863998795839590272, -7.631215200338315796 ) ) ;
#17866 = CARTESIAN_POINT ( 'NONE',  ( 117.1162029564635674, -11.29425726270896035, -21.74748621749282051 ) ) ;
#17867 = CARTESIAN_POINT ( 'NONE',  ( 111.7184548109119788, -9.261995988541697145, -16.69588392320189030 ) ) ;
#17868 = CARTESIAN_POINT ( 'NONE',  ( 117.5045748109119756, -9.859900752359374465, -12.68260735090039404 ) ) ;
#17869 = CARTESIAN_POINT ( 'NONE',  ( 125.4584548109119737, -6.717659058379802595, -19.62329895828877468 ) ) ;
#17870 = ORIENTED_EDGE ( 'NONE', *, *, #23468, .T. ) ;
#17871 = AXIS2_PLACEMENT_3D ( 'NONE', #29449, #31963, #18294 ) ;
#17872 = CARTESIAN_POINT ( 'NONE',  ( 117.1074881442453233, 0.4262465694468514643, -12.03445270309931736 ) ) ;
#17873 = DIRECTION ( 'NONE',  ( 0.000000000000000000, 0.6004852223388327248, -0.7996358532186277346 ) ) ;
#17874 = CARTESIAN_POINT ( 'NONE',  ( 114.1934435773848833, -2.467220198592768199, -17.83387418641523325 ) ) ;
#17875 = CARTESIAN_POINT ( 'NONE',  ( 115.2053796295247849, -4.863998795839590272, -19.15521520033831493 ) ) ;
#17876 = CARTESIAN_POINT ( 'NONE',  ( 115.8595014775786609, -1.834011780172310813, -8.268836392978581529 ) ) ;
#17877 = ORIENTED_EDGE ( 'NONE', *, *, #40253, .F. ) ;
#17878 = CARTESIAN_POINT ( 'NONE',  ( 118.5823814775786360, -1.834011780172310813, -8.268836392978581529 ) ) ;
#17879 = LINE ( 'NONE', #34734, #45109 ) ;
#17880 = CARTESIAN_POINT ( 'NONE',  ( 110.6909265045248247, -7.250697342233347165, -19.15521520033831138 ) ) ;
#17881 = CARTESIAN_POINT ( 'NONE',  ( 126.0703014775786102, -0.1624402480850797581, -16.17319339645315424 ) ) ;
#17882 = CARTESIAN_POINT ( 'NONE',  ( 114.2144281442453178, -8.166667518702817929, -8.995218007635859436 ) ) ;
#17883 = CARTESIAN_POINT ( 'NONE',  ( 126.8137406967851319, -10.15933636723070599, -13.56223398357370158 ) ) ;
#17884 = CARTESIAN_POINT ( 'NONE',  ( 90.45092582798827152, -26.75858941326842810, -11.54476601486570964 ) ) ;
#17885 = CARTESIAN_POINT ( 'NONE',  ( 111.1770983795247787, -8.402594152722688392, -16.93181055722141792 ) ) ;
#17886 = VERTEX_POINT ( 'NONE', #13031 ) ;
#17887 = DIRECTION ( 'NONE',  ( 1.000000000000000000, 0.000000000000000000, -0.000000000000000000 ) ) ;
#17888 = CARTESIAN_POINT ( 'NONE',  ( 109.2294337548798779, -7.896060072502915084, -17.78522704774125174 ) ) ;
#17889 = CARTESIAN_POINT ( 'NONE',  ( 115.0086014775786509, -5.574606645277164318, -18.38911715685844683 ) ) ;
#17890 = DIRECTION ( 'NONE',  ( 1.000000000000000000, 0.000000000000000000, 0.000000000000000000 ) ) ;
#17891 = CIRCLE ( 'NONE', #44136, 12.50000000000000178 ) ;
#17892 = CARTESIAN_POINT ( 'NONE',  ( 115.1359265045248605, -2.791137627527939813, -8.388885654883777576 ) ) ;
#17893 = CARTESIAN_POINT ( 'NONE',  ( 107.8433483795247838, -0.7896495226426338832, -9.318865927141430916 ) ) ;
#17894 = CARTESIAN_POINT ( 'NONE',  ( 127.7617783745857452, -5.489033741201595262, -7.655088239364113534 ) ) ;
#17895 = CARTESIAN_POINT ( 'NONE',  ( 125.9001214775786224, -4.089484607189486809, -7.948022111789456723 ) ) ;
#17896 = CARTESIAN_POINT ( 'NONE',  ( 120.3409081442453044, -8.899110576539722928, -16.42337572283488356 ) ) ;
#17897 = CARTESIAN_POINT ( 'NONE',  ( 125.4463081442452932, -5.638512984488999180, -18.83840828888717311 ) ) ;
#17898 = CARTESIAN_POINT ( 'NONE',  ( 115.9729548109119861, -6.344957434206662583, -7.627207830600332805 ) ) ;
#17900 = VERTEX_POINT ( 'NONE', #27161 ) ;
#17899 = ADVANCED_FACE ( 'NONE', ( #26929 ), #2980, .T. ) ;
#17901 = CARTESIAN_POINT ( 'NONE',  ( 115.9162281442453093, -5.574606645277164318, -18.38911715685844683 ) ) ;
#17902 = CARTESIAN_POINT ( 'NONE',  ( 84.86020291624612355, -30.49489077589588604, -18.39321520033831803 ) ) ;
#17903 = CARTESIAN_POINT ( 'NONE',  ( 116.1998614775786507, -10.63000616557722466, -14.87417383870573495 ) ) ;
#17904 = CARTESIAN_POINT ( 'NONE',  ( 116.2565881442453133, -0.8288870151387760510, -10.36305467784173118 ) ) ;
#17905 = ORIENTED_EDGE ( 'NONE', *, *, #39993, .F. ) ;
#17906 = CARTESIAN_POINT ( 'NONE',  ( 119.6034614775786196, -3.505236298600246325, -18.68346056562440793 ) ) ;
#17907 = CARTESIAN_POINT ( 'NONE',  ( 118.1852948109119836, -5.638512984488999180, -18.83840828888717311 ) ) ;
#17908 = EDGE_CURVE ( 'NONE', #34165, #30525, #981, .T. ) ;
#17909 = CARTESIAN_POINT ( 'NONE',  ( 135.5366836739015071, 0.6402420525674652474, -15.78128361289120640 ) ) ;
#17910 = CARTESIAN_POINT ( 'NONE',  ( 109.9269421295247753, 0.8980012041604618078, -13.39321520033831447 ) ) ;
#17911 = CARTESIAN_POINT ( 'NONE',  ( 67.30914723170953096, -53.23718887596189120, -35.39220701967414584 ) ) ;
#17912 = CARTESIAN_POINT ( 'NONE',  ( 89.78938736644981589, -25.99489077589524300, -13.39321520033831625 ) ) ;
#17913 = CARTESIAN_POINT ( 'NONE',  ( 70.19189222814998175, -100.0979043305785581, -53.24182196210380624 ) ) ;
#17914 = CARTESIAN_POINT ( 'NONE',  ( 114.8951481442453115, -0.4660016031367893996, -10.09054647747474043 ) ) ;
#17915 = CIRCLE ( 'NONE', #28146, 2.999999999999999556 ) ;
#17916 = CARTESIAN_POINT ( 'NONE',  ( 119.7434548109119703, -7.429215134363809092, -20.97079166887802160 ) ) ;
#17917 = CARTESIAN_POINT ( 'NONE',  ( 115.1220548109119761, -1.833838273342658809, -17.42832698103878286 ) ) ;
#17918 = CARTESIAN_POINT ( 'NONE',  ( 62.66980483302768334, -12.54647196691845323, -16.71198379459248429 ) ) ;
#17919 = FACE_OUTER_BOUND ( 'NONE', #29483, .T. ) ;
#17920 = CARTESIAN_POINT ( 'NONE',  ( 115.3442858795247759, -8.402594152722688392, -9.854619843455216355 ) ) ;
#17921 = CARTESIAN_POINT ( 'NONE',  ( 112.2857214775786474, -5.574606645277164318, -18.38911715685844683 ) ) ;
#17922 = CARTESIAN_POINT ( 'NONE',  ( 81.52050388106540879, 0.5255923868638483487, -15.89321520033831447 ) ) ;
#17923 = DIRECTION ( 'NONE',  ( 0.000000000000000000, 0.6004852223388321697, -0.7996358532186279566 ) ) ;
#17925 = CARTESIAN_POINT ( 'NONE',  ( 119.2063748109119814, -1.561330072975668504, -17.79121239304076951 ) ) ;
#17924 = DIRECTION ( 'NONE',  ( 0.000000000000000000, -0.3818493186865927203, 0.9242245927363029745 ) ) ;
#17926 = CARTESIAN_POINT ( 'NONE',  ( 124.1415948109119540, -3.505236298600246325, -18.68346056562440793 ) ) ;
#17927 = CARTESIAN_POINT ( 'NONE',  ( 120.1707281442453166, -9.565557343593413364, -10.61323700422348004 ) ) ;
#17928 = CARTESIAN_POINT ( 'NONE',  ( 111.8886348109120092, -6.222761293078241884, -8.102969835052219238 ) ) ;
#17929 = ORIENTED_EDGE ( 'NONE', *, *, #39135, .T. ) ;
#17930 = CARTESIAN_POINT ( 'NONE',  ( 136.1332990479124589, -7.072588780063932212, -7.940136130744186893 ) ) ;
#17931 = CARTESIAN_POINT ( 'NONE',  ( 124.6521348109119884, -1.561330072975668948, -17.79121239304076951 ) ) ;
#17932 = CARTESIAN_POINT ( 'NONE',  ( 113.3995983795247895, -8.402594152722688392, -16.93181055722141792 ) ) ;
#17933 = CARTESIAN_POINT ( 'NONE',  ( 119.8303681442453126, 0.4262465694468514643, -12.03445270309931736 ) ) ;
#17934 = AXIS2_PLACEMENT_3D ( 'NONE', #24630, #10731, #42635 ) ;
#17935 = CARTESIAN_POINT ( 'NONE',  ( 126.1270281442452870, -10.30919188438810075, -12.61870101168855918 ) ) ;
#17936 = CARTESIAN_POINT ( 'NONE',  ( 84.89885432604606308, -29.90127023760751612, -11.39376025726712349 ) ) ;
#17937 = CARTESIAN_POINT ( 'NONE',  ( 112.7050671295247923, -10.62599879583958540, -13.39321520033831447 ) ) ;
#17938 = CARTESIAN_POINT ( 'NONE',  ( 118.8660148109119774, 0.1319031606808879209, -14.10382304977623669 ) ) ;
#17939 = CARTESIAN_POINT ( 'NONE',  ( 119.1496481442453046, -6.222761293078241884, -8.102969835052219238 ) ) ;
#17940 = CARTESIAN_POINT ( 'NONE',  ( 116.5987716749792895, -9.866677412677834269, -13.52174868289714027 ) ) ;
#17941 = CARTESIAN_POINT ( 'NONE',  ( 109.2295693424392908, -6.082835033032921501, -7.893315249734571104 ) ) ;
#17942 = CARTESIAN_POINT ( 'NONE',  ( 120.3685329359119862, -4.283928203966213211, -7.183505701512925334 ) ) ;
#17943 = CARTESIAN_POINT ( 'NONE',  ( 110.9687390045248350, -9.868328341294098749, -11.32035403202665869 ) ) ;
#17944 = CARTESIAN_POINT ( 'NONE',  ( 116.5324863327809339, 2.186940848879305399, -20.53455829175617353 ) ) ;
#17945 = CARTESIAN_POINT ( 'NONE',  ( 118.8092881442453290, -9.988377603198976828, -10.36322818467138340 ) ) ;
#17946 = CARTESIAN_POINT ( 'NONE',  ( 113.0798948109119948, -0.4660016031367893996, -10.09054647747474043 ) ) ;
#17947 = CARTESIAN_POINT ( 'NONE',  ( 109.9269421295247753, 0.8980012041604618078, -13.39321520033831447 ) ) ;
#17948 = CARTESIAN_POINT ( 'NONE',  ( 112.6260814775786514, -9.261995988541697145, -16.69588392320189030 ) ) ;
#17949 = VERTEX_POINT ( 'NONE', #44492 ) ;
#17950 = DIRECTION ( 'NONE',  ( 1.000000000000000000, 0.000000000000000000, -0.000000000000000000 ) ) ;
#17951 = CARTESIAN_POINT ( 'NONE',  ( 124.1415948109119540, -6.344957434206665248, -7.627207830600338134 ) ) ;
#17952 = CARTESIAN_POINT ( 'NONE',  ( 115.2355081442453155, -10.30919188438810075, -12.61870101168855918 ) ) ;
#17953 = CARTESIAN_POINT ( 'NONE',  ( 120.9081748109119872, -4.153390946401325223, -8.397313243818185668 ) ) ;
#17954 = AXIS2_PLACEMENT_3D ( 'NONE', #29665, #1394, #40158 ) ;
#17955 = CARTESIAN_POINT ( 'NONE',  ( 124.9924948109119924, -4.089484607189486809, -7.948022111789456723 ) ) ;
#17956 = CARTESIAN_POINT ( 'NONE',  ( 123.1772414775786189, -4.089484607189486809, -7.948022111789456723 ) ) ;
#17957 = CARTESIAN_POINT ( 'NONE',  ( 113.4690515045247992, -2.477300249445798297, -7.631215200338321125 ) ) ;
#17958 = EDGE_CURVE ( 'NONE', #13784, #34606, #26473, .T. ) ;
#17959 = CARTESIAN_POINT ( 'NONE',  ( 116.3133148109120043, -2.084020599724406786, -8.691656652584148546 ) ) ;
#17960 = DIRECTION ( 'NONE',  ( 0.000000000000000000, -0.9242245927363029745, -0.3818493186865927203 ) ) ;
#17961 = ORIENTED_EDGE ( 'NONE', *, *, #41910, .T. ) ;
#17962 = CARTESIAN_POINT ( 'NONE',  ( 122.1561614775786353, -0.4660016031367893996, -10.09054647747474043 ) ) ;
#17963 = AXIS2_PLACEMENT_3D ( 'NONE', #43320, #12089, #8659 ) ;
#17964 = CARTESIAN_POINT ( 'NONE',  ( 119.8129079359119942, -4.360204210389833968, -8.000047426360245240 ) ) ;
#17965 = CARTESIAN_POINT ( 'NONE',  ( 120.5110881442453206, -6.344957434206665248, -7.627207830600338134 ) ) ;
#17966 = ORIENTED_EDGE ( 'NONE', *, *, #23045, .T. ) ;
#17967 = CARTESIAN_POINT ( 'NONE',  ( 106.1764733795248219, -1.325403438956436419, -9.854619843455211026 ) ) ;
#17968 = CARTESIAN_POINT ( 'NONE',  ( 124.4252281442452812, -9.261995988541697145, -16.69588392320189030 ) ) ;
#17969 = CARTESIAN_POINT ( 'NONE',  ( 65.41257106814472877, -15.47412461924279725, -16.39321520033831447 ) ) ;
#17970 = CARTESIAN_POINT ( 'NONE',  ( 116.3700414775786527, -4.153390946401321671, -8.397313243818183892 ) ) ;
#17971 = CARTESIAN_POINT ( 'NONE',  ( 77.38585178070579218, -56.64430055435828848, -1.796958453011376022 ) ) ;
#17972 = CARTESIAN_POINT ( 'NONE',  ( 121.0216281442452981, -7.894159318335828068, -9.358103419637847864 ) ) ;
#17973 = DIRECTION ( 'NONE',  ( 0.7871354856660198740, 0.4483307682966886643, 0.4235767337848242442 ) ) ;
#17974 = CARTESIAN_POINT ( 'NONE',  ( 121.6456214775786293, 0.4262465694468514643, -12.03445270309931736 ) ) ;
#17975 = CARTESIAN_POINT ( 'NONE',  ( 85.82015659721905365, -25.99489077589524300, -13.39321520033831625 ) ) ;
#17976 = VECTOR ( 'NONE', #410, 1000.000000000000000 ) ;
#17977 = CARTESIAN_POINT ( 'NONE',  ( 119.5467348109119712, -5.574606645277164318, -18.38911715685844683 ) ) ;
#17978 = CARTESIAN_POINT ( 'NONE',  ( 112.6828081442453282, -7.893985811506177619, -18.51759400769804742 ) ) ;
#17979 = CARTESIAN_POINT ( 'NONE',  ( 118.2987481442453088, -1.561330072975668504, -17.79121239304076951 ) ) ;
#17980 = CARTESIAN_POINT ( 'NONE',  ( 112.1155414775786454, 0.9020085738987339008, -11.91225656197089222 ) ) ;
#17981 = CARTESIAN_POINT ( 'NONE',  ( 84.86020291624612355, -29.99489077589588959, -12.39321520033834645 ) ) ;
#17982 = CARTESIAN_POINT ( 'NONE',  ( 121.1918081442452859, -10.15424416112533912, -14.75197769757731336 ) ) ;
#17983 = ORIENTED_EDGE ( 'NONE', *, *, #26672, .T. ) ;
#17984 = CARTESIAN_POINT ( 'NONE',  ( 115.0653281442453277, -6.344957434206662583, -7.627207830600332805 ) ) ;
#17985 = CARTESIAN_POINT ( 'NONE',  ( 112.0799890045248475, -9.868328341294098749, -11.32035403202665869 ) ) ;
#17986 = CONICAL_SURFACE ( 'NONE', #21602, 0.8509999999999994236, 0.06981317007976593769 ) ;
#17987 = CARTESIAN_POINT ( 'NONE',  ( 115.3489614775786407, -0.8288870151387673912, -10.36305467784174184 ) ) ;
#17988 = CYLINDRICAL_SURFACE ( 'NONE', #29830, 1.999999999999998890 ) ;
#17989 = CARTESIAN_POINT ( 'NONE',  ( 121.9659548109119811, -2.527210466738039951, -8.967976844669125924 ) ) ;
#17990 = CARTESIAN_POINT ( 'NONE',  ( 120.9081748109119872, -5.638512984488999180, -18.83840828888717311 ) ) ;
#17991 = ORIENTED_EDGE ( 'NONE', *, *, #35379, .T. ) ;
#17992 = CARTESIAN_POINT ( 'NONE',  ( 126.4162218615764743, -8.334346880300483207, -9.657250028486881632 ) ) ;
#17993 = CARTESIAN_POINT ( 'NONE',  ( 122.3830681442452857, -1.833838273342659697, -17.42832698103878286 ) ) ;
#17994 = CARTESIAN_POINT ( 'NONE',  ( 120.0212673109119805, 0.2312338769422704887, -16.08380026872395874 ) ) ;
#17995 = DIRECTION ( 'NONE',  ( 0.000000000000000000, -0.4669533266896287449, -0.8842819633428518067 ) ) ;
#17996 = MECHANICAL_DESIGN_GEOMETRIC_PRESENTATION_REPRESENTATION (  '', ( #19467 ), #4159 ) ;
#17997 = DIRECTION ( 'NONE',  ( 0.000000000000000000, 0.9284778069183718952, 0.3713878862591649677 ) ) ;
#17998 = CARTESIAN_POINT ( 'NONE',  ( 113.9552233795247815, -1.325403438956436419, -9.854619843455211026 ) ) ;
#17999 = VERTEX_POINT ( 'NONE', #37169 ) ;
#18000 = CARTESIAN_POINT ( 'NONE',  ( 114.1577014775786552, -6.344957434206662583, -7.627207830600332805 ) ) ;
#18001 = CARTESIAN_POINT ( 'NONE',  ( 126.2404814775786264, -0.8288870151387760510, -10.36305467784173118 ) ) ;
#18002 = CARTESIAN_POINT ( 'NONE',  ( 122.4397948109119767, -9.988377603198976828, -10.36322818467138340 ) ) ;
#18003 = CARTESIAN_POINT ( 'NONE',  ( 121.9859814775786333, -9.565557343593413364, -10.61323700422348004 ) ) ;
#18004 = CARTESIAN_POINT ( 'NONE',  ( 126.2184548109105435, -4.159894987975746972, -8.443039665293909479 ) ) ;
#18005 = CARTESIAN_POINT ( 'NONE',  ( 123.9714148109119805, -0.4660016031367893996, -10.09054647747474043 ) ) ;
#18006 = CARTESIAN_POINT ( 'NONE',  ( 2.181596283295915484, -11.50482699009217669, -8.893215200338314474 ) ) ;
#18007 = CARTESIAN_POINT ( 'NONE',  ( 85.38561350750011059, -9.917550408422661334, -8.143215200338314474 ) ) ;
#18008 = DIRECTION ( 'NONE',  ( 0.000000000000000000, 0.000000000000000000, -1.000000000000000000 ) ) ;
#18009 = CARTESIAN_POINT ( 'NONE',  ( 112.2857214775786474, -4.089484607189486809, -7.948022111789456723 ) ) ;
#18010 = ORIENTED_EDGE ( 'NONE', *, *, #10152, .F. ) ;
#18011 = CARTESIAN_POINT ( 'NONE',  ( 115.4137390045248566, -9.868328341294098749, -11.32035403202665869 ) ) ;
#18012 = AXIS2_PLACEMENT_3D ( 'NONE', #33156, #40250, #9017 ) ;
#18013 = CARTESIAN_POINT ( 'NONE',  ( 119.3765548109119834, 0.9020085738987339008, -11.91225656197089222 ) ) ;
#18014 = CARTESIAN_POINT ( 'NONE',  ( 135.5886503745704488, -10.44469069420684804, -15.59668197382750598 ) ) ;
#18015 = ORIENTED_EDGE ( 'NONE', *, *, #15886, .T. ) ;
#18016 = CARTESIAN_POINT ( 'NONE',  ( 121.0024232127138504, -2.191907684172563986, -18.20049396185734025 ) ) ;
#18017 = CARTESIAN_POINT ( 'NONE',  ( 123.1772414775786189, -4.089484607189486809, -7.948022111789456723 ) ) ;
#18018 = DIRECTION ( 'NONE',  ( 1.000000000000000000, 0.000000000000000000, -0.000000000000000000 ) ) ;
#18019 = CARTESIAN_POINT ( 'NONE',  ( 121.7023481442452919, -0.8288870151387760510, -10.36305467784173118 ) ) ;
#18020 = ORIENTED_EDGE ( 'NONE', *, *, #23916, .F. ) ;
#18021 = CARTESIAN_POINT ( 'NONE',  ( 114.2711548109119803, -9.988377603198976828, -10.36322818467138340 ) ) ;
#18022 = LINE ( 'NONE', #1362, #16114 ) ;
#18023 = DIRECTION ( 'NONE',  ( 0.000000000000000000, -0.3818493186865936084, 0.9242245927363024194 ) ) ;
#18024 = CIRCLE ( 'NONE', #4899, 0.1999999999999988731 ) ;
#18025 = DIRECTION ( 'NONE',  ( -1.000000000000000000, 0.000000000000000000, 0.000000000000000000 ) ) ;
#18026 = ADVANCED_FACE ( 'NONE', ( #5944 ), #4119, .T. ) ;
#18027 = CARTESIAN_POINT ( 'NONE',  ( 111.6050014775786536, 0.1319031606808879209, -14.10382304977623669 ) ) ;
#18028 = DIRECTION ( 'NONE',  ( 1.000000000000000000, 0.000000000000000000, 0.000000000000000000 ) ) ;
#18029 = FACE_OUTER_BOUND ( 'NONE', #16363, .T. ) ;
#18030 = CARTESIAN_POINT ( 'NONE',  ( 122.9503348109119827, 0.5811942927096110934, -14.16772938898807510 ) ) ;
#18032 = CARTESIAN_POINT ( 'NONE',  ( 124.1983214775786166, -1.833838273342659697, -17.42832698103878286 ) ) ;
#18031 = CARTESIAN_POINT ( 'NONE',  ( 122.3263414775786373, -6.344957434206665248, -7.627207830600338134 ) ) ;
#18033 = CARTESIAN_POINT ( 'NONE',  ( 119.3765548109119834, -10.15424416112533912, -14.75197769757731336 ) ) ;
#18034 =( BOUNDED_SURFACE ( )  B_SPLINE_SURFACE ( 1, 2, ( 
 ( #29736, #18582, #39775, #15837, #36566, #18805, #1910, #36338, #42976, #19026, #43647, #1464, #32475, #2132, #43883, #32911, #39332, #22000, #30420, #37932, #26780, #40462, #6250, #45013, #33589, #24040, #6480, #41149, #2364, #23132, #9224, #16295, #37010, #9674, #5780, #34054, #31087, #27458, #30195, #44114, #12880, #27234, #41380, #44341, #13100, #37239, #19701, #16977, #19935, #16523, #44564, #30645, #26550, #20394, #34494, #2821, #40689, #30868, #10135, #9910, #13327, #9442, #3051, #44790, #23354, #6011, #33821, #6708, #34278, #23823, #2592, #27002, #40920, #23592, #37476, #20171, #16750, #37709, #13548, #20617, #3270, #17195, #77, #14435, #28575, #31529, #17633, #24474, #38151, #4163, #7138, #3713, #31754, #17856, #32199, #38816, #21727, #35156, #6925, #18079, #42483, #28343, #524, #27904, #35386, #31974, #13772, #3936, #41819, #10576, #25153, #737, #14660, #299, #11245, #39049, #42256, #34711, #21499, #35615, #7820, #28127, #11020, #27683, #13990, #42036, #10795, #24921, #24692, #4389, #38364, #18304, #7585, #41597, #38581, #14212, #7359, #10354, #24261, #3496, #21274, #20830, #17413, #31304, #21049, #34926, #29686, #43373, #22617, #39726, #18975, #8492, #22845, #5503, #42929, #8266, #8041, #25817, #36291, #29460, #33084, #22171, #36065, #36517, #32645, #11475, #1413, #4835, #36737, #25379, #5290, #42706, #15331, #19205, #32863, #18532, #22396, #29241, #21947, #18756, #12143, #15110, #39277, #1634, #5059, #43149, #1197, #15554, #11918, #12370, #29019, #14888, #26045, #32424, #39950, #8712, #35838, #1855, #15784, #11691, #4611, #43597, #26270, #40178, #25600, #8944, #19424, #971, #39505, #28799, #13045, #6652, #40409, #30817, #13272, #2771, #9169, #29917, #2085, #23074, #16009, #16465, #43832, #40867, #37877, #34224, #36957, #5728, #19647, #34001, #2997, #5957, #37184, #44059, #12599, #23765, #26724, #23300, #6195, #37425, #33310, #27178, #41327, #9621, #26501, #37656, #16922, #16695, #20114, #2312, #9857, #6430, #33533, #23541, #16242, #30144, #44740 ),
 ( #12825, #40633, #9389, #13499, #27405, #19883, #2539, #44291, #26944, #33770, #10085, #23988, #30369, #30589, #44508, #41098, #20340, #17581, #13721, #28072, #42428, #17803, #41980, #27628, #24207, #31919, #6873, #3447, #38989, #14155, #17365, #31474, #21222, #10745, #247, #4099, #20782, #11192, #38758, #31696, #20562, #7089, #31253, #24422, #684, #18021, #13938, #31033, #14603, #35099, #10305, #35330, #10521, #28522, #464, #14379, #41543, #34441, #34872, #7304, #38312, #38099, #25095, #21445, #25, #34661, #42201, #3661, #10963, #27851, #3220, #41760, #17147, #44965, #20998, #24644, #38526, #3881, #28292, #24867, #7529, #12315, #1137, #18700, #42648, #29407, #4781, #913, #15272, #29630, #5003, #29181, #14834, #11416, #19144, #39218, #35786, #26212, #1360, #4555, #32591, #8437, #43093, #11862, #36460, #7982, #43545, #25992, #18916, #7760, #39450, #18482, #11631, #33028, #5230, #15056, #18250, #1802, #22342, #25325, #22559, #42874, #15729, #32808, #1578, #25768, #15499, #32145, #43319, #25544, #28744, #21668, #12087, #28967, #36237, #21891, #39897, #32371, #8212, #22119, #8658, #39673, #36011, #35556, #4328, #30307, #12539, #19369, #5675, #6137, #44684, #12992, #2255, #5449, #26443, #37600, #27118, #30759, #44232, #9564, #33940, #41042, #20281, #2483, #16869, #16637, #19824, #9111, #23479, #15955, #33712, #19593, #9798, #5902, #30531, #2030, #36903, #20058, #23013, #44452, #34166, #13444, #37366, #2710, #6370, #13219, #29858, #23709, #30088, #2938, #40121, #8884, #26888, #22785, #33258, #36679, #44001, #43774, #40349, #33474, #16183, #40807, #12765, #26664, #40577, #9337, #23246, #37127, #16408, #45124, #7469, #21387, #17520, #44909, #6591, #38045, #38474, #31867, #184, #34608, #37816, #13666, #24809, #14326, #17968, #31418, #41924, #21163, #28240, #35269, #34822, #4046, #3821, #7038, #41487, #10689, #3170, #20948, #6822, #42149, #38257, #17745, #34387, #24154, #7250, #10245, #31641, #634, #27350, #24591, #35041, #20509, #41269, #41704, #14102, #17312, #17092 ) ),
 .UNSPECIFIED., .F., .F., .T. ) 
 B_SPLINE_SURFACE_WITH_KNOTS ( ( 2, 2 ),
 ( 3, 2, 2, 2, 2, 2, 2, 2, 2, 2, 2, 2, 2, 2, 2, 2, 2, 2, 2, 2, 2, 2, 2, 2, 2, 2, 2, 2, 2, 2, 2, 2, 2, 2, 2, 2, 2, 2, 2, 2, 2, 2, 2, 2, 2, 2, 2, 2, 2, 2, 2, 2, 2, 2, 2, 2, 2, 2, 2, 2, 2, 2, 2, 2, 2, 2, 2, 2, 2, 2, 2, 2, 2, 2, 2, 2, 2, 2, 2, 2, 2, 2, 2, 2, 2, 2, 2, 2, 2, 2, 2, 2, 2, 2, 2, 2, 2, 2, 2, 2, 2, 2, 2, 2, 2, 2, 2, 2, 2, 2, 2, 2, 2, 2, 2, 2, 2, 2, 2, 2, 2, 2, 2, 2, 2, 2, 2, 2, 3 ),
 ( 0.000000000000000000, 1.000000000000000000 ),
 ( 0.000000000000000000, 0.007812500000000000000, 0.01562500000000000000, 0.02343750000000000000, 0.03125000000000000000, 0.03906250000000000000, 0.04687500000000000000, 0.05468750000000000000, 0.06250000000000000000, 0.07031250000000000000, 0.07812500000000000000, 0.08593750000000000000, 0.09375000000000000000, 0.1015625000000000000, 0.1093750000000000000, 0.1171875000000000000, 0.1250000000000000000, 0.1328125000000000000, 0.1406250000000000000, 0.1484375000000000000, 0.1562500000000000000, 0.1640625000000000000, 0.1718750000000000000, 0.1796875000000000000, 0.1875000000000000000, 0.1953125000000000000, 0.2031250000000000000, 0.2109375000000000000, 0.2187500000000000000, 0.2265625000000000000, 0.2343750000000000000, 0.2421875000000000000, 0.2500000000000000000, 0.2578125000000000000, 0.2656250000000000000, 0.2734375000000000000, 0.2812500000000000000, 0.2890625000000000000, 0.2968750000000000000, 0.3046875000000000000, 0.3125000000000000000, 0.3203125000000000000, 0.3281250000000000000, 0.3359375000000000000, 0.3437500000000000000, 0.3515625000000000000, 0.3593750000000000000, 0.3671875000000000000, 0.3750000000000000000, 0.3828125000000000000, 0.3906250000000000000, 0.3984375000000000000, 0.4062500000000000000, 0.4140625000000000000, 0.4218750000000000000, 0.4296875000000000000, 0.4375000000000000000, 0.4453125000000000000, 0.4531250000000000000, 0.4609375000000000000, 0.4687500000000000000, 0.4765625000000000000, 0.4843750000000000000, 0.4921875000000000000, 0.5000000000000000000, 0.5078125000000000000, 0.5156250000000000000, 0.5234375000000000000, 0.5312500000000000000, 0.5390625000000000000, 0.5468750000000000000, 0.5546875000000000000, 0.5625000000000000000, 0.5703125000000000000, 0.5781250000000000000, 0.5859375000000000000, 0.5937500000000000000, 0.6015625000000000000, 0.6093750000000000000, 0.6171875000000000000, 0.6250000000000000000, 0.6328125000000000000, 0.6406250000000000000, 0.6484375000000000000, 0.6562500000000000000, 0.6640625000000000000, 0.6718750000000000000, 0.6796875000000000000, 0.6875000000000000000, 0.6953125000000000000, 0.7031250000000000000, 0.7109375000000000000, 0.7187500000000000000, 0.7265625000000000000, 0.7343750000000000000, 0.7421875000000000000, 0.7500000000000000000, 0.7578125000000000000, 0.7656250000000000000, 0.7734375000000000000, 0.7812500000000000000, 0.7890625000000000000, 0.7968750000000000000, 0.8046875000000000000, 0.8125000000000000000, 0.8203125000000000000, 0.8281250000000000000, 0.8359375000000000000, 0.8437500000000000000, 0.8515625000000000000, 0.8593750000000000000, 0.8671875000000000000, 0.8750000000000000000, 0.8828125000000000000, 0.8906250000000000000, 0.8984375000000000000, 0.9062500000000000000, 0.9140625000000000000, 0.9218750000000000000, 0.9296875000000000000, 0.9375000000000000000, 0.9453125000000000000, 0.9531250000000000000, 0.9609375000000000000, 0.9687500000000000000, 0.9765625000000000000, 0.9843750000000000000, 0.9921875000000000000, 1.000000000000000000 ),
 .UNSPECIFIED. ) 
 GEOMETRIC_REPRESENTATION_ITEM ( )  RATIONAL_B_SPLINE_SURFACE ( (
 ( 1.000000000000000000, 0.9238795325112869605, 1.000000000000000000, 0.9238795325112869605, 1.000000000000000000, 0.9238795325112869605, 1.000000000000000000, 0.9238795325112869605, 1.000000000000000000, 0.9238795325112869605, 1.000000000000000000, 0.9238795325112869605, 1.000000000000000000, 0.9238795325112869605, 1.000000000000000000, 0.9238795325112869605, 1.000000000000000000, 0.9238795325112869605, 1.000000000000000000, 0.9238795325112869605, 1.000000000000000000, 0.9238795325112869605, 1.000000000000000000, 0.9238795325112869605, 1.000000000000000000, 0.9238795325112869605, 1.000000000000000000, 0.9238795325112869605, 1.000000000000000000, 0.9238795325112869605, 1.000000000000000000, 0.9238795325112869605, 1.000000000000000000, 0.9238795325112869605, 1.000000000000000000, 0.9238795325112869605, 1.000000000000000000, 0.9238795325112869605, 1.000000000000000000, 0.9238795325112869605, 1.000000000000000000, 0.9238795325112869605, 1.000000000000000000, 0.9238795325112869605, 1.000000000000000000, 0.9238795325112869605, 1.000000000000000000, 0.9238795325112869605, 1.000000000000000000, 0.9238795325112869605, 1.000000000000000000, 0.9238795325112869605, 1.000000000000000000, 0.9238795325112869605, 1.000000000000000000, 0.9238795325112869605, 1.000000000000000000, 0.9238795325112869605, 1.000000000000000000, 0.9238795325112869605, 1.000000000000000000, 0.9238795325112869605, 1.000000000000000000, 0.9238795325112869605, 1.000000000000000000, 0.9238795325112869605, 1.000000000000000000, 0.9238795325112869605, 1.000000000000000000, 0.9238795325112869605, 1.000000000000000000, 0.9238795325112869605, 1.000000000000000000, 0.9238795325112869605, 1.000000000000000000, 0.9238795325112869605, 1.000000000000000000, 0.9238795325112869605, 1.000000000000000000, 0.9238795325112869605, 1.000000000000000000, 0.9238795325112869605, 1.000000000000000000, 0.9238795325112869605, 1.000000000000000000, 0.9238795325112869605, 1.000000000000000000, 0.9238795325112869605, 1.000000000000000000, 0.9238795325112869605, 1.000000000000000000, 0.9238795325112869605, 1.000000000000000000, 0.9238795325112869605, 1.000000000000000000, 0.9238795325112869605, 1.000000000000000000, 0.9238795325112869605, 1.000000000000000000, 0.9238795325112869605, 1.000000000000000000, 0.9238795325112869605, 1.000000000000000000, 0.9238795325112869605, 1.000000000000000000, 0.9238795325112869605, 1.000000000000000000, 0.9238795325112869605, 1.000000000000000000, 0.9238795325112869605, 1.000000000000000000, 0.9238795325112869605, 1.000000000000000000, 0.9238795325112869605, 1.000000000000000000, 0.9238795325112869605, 1.000000000000000000, 0.9238795325112869605, 1.000000000000000000, 0.9238795325112869605, 1.000000000000000000, 0.9238795325112869605, 1.000000000000000000, 0.9238795325112869605, 1.000000000000000000, 0.9238795325112869605, 1.000000000000000000, 0.9238795325112869605, 1.000000000000000000, 0.9238795325112869605, 1.000000000000000000, 0.9238795325112869605, 1.000000000000000000, 0.9238795325112869605, 1.000000000000000000, 0.9238795325112869605, 1.000000000000000000, 0.9238795325112869605, 1.000000000000000000, 0.9238795325112869605, 1.000000000000000000, 0.9238795325112869605, 1.000000000000000000, 0.9238795325112869605, 1.000000000000000000, 0.9238795325112869605, 1.000000000000000000, 0.9238795325112869605, 1.000000000000000000, 0.9238795325112869605, 1.000000000000000000, 0.9238795325112869605, 1.000000000000000000, 0.9238795325112869605, 1.000000000000000000, 0.9238795325112869605, 1.000000000000000000, 0.9238795325112869605, 1.000000000000000000, 0.9238795325112869605, 1.000000000000000000, 0.9238795325112869605, 1.000000000000000000, 0.9238795325112869605, 1.000000000000000000, 0.9238795325112869605, 1.000000000000000000, 0.9238795325112869605, 1.000000000000000000, 0.9238795325112869605, 1.000000000000000000, 0.9238795325112869605, 1.000000000000000000, 0.9238795325112869605, 1.000000000000000000, 0.9238795325112869605, 1.000000000000000000, 0.9238795325112869605, 1.000000000000000000, 0.9238795325112869605, 1.000000000000000000, 0.9238795325112869605, 1.000000000000000000, 0.9238795325112869605, 1.000000000000000000, 0.9238795325112869605, 1.000000000000000000, 0.9238795325112869605, 1.000000000000000000, 0.9238795325112869605, 1.000000000000000000, 0.9238795325112869605, 1.000000000000000000, 0.9238795325112869605, 1.000000000000000000, 0.9238795325112869605, 1.000000000000000000, 0.9238795325112869605, 1.000000000000000000, 0.9238795325112869605, 1.000000000000000000, 0.9238795325112869605, 1.000000000000000000, 0.9238795325112869605, 1.000000000000000000, 0.9238795325112869605, 1.000000000000000000, 0.9238795325112869605, 1.000000000000000000, 0.9238795325112869605, 1.000000000000000000, 0.9238795325112869605, 1.000000000000000000, 0.9238795325112869605, 1.000000000000000000, 0.9238795325112869605, 1.000000000000000000, 0.9238795325112869605, 1.000000000000000000, 0.9238795325112869605, 1.000000000000000000, 0.9238795325112869605, 1.000000000000000000, 0.9238795325112869605, 1.000000000000000000, 0.9238795325112869605, 1.000000000000000000, 0.9238795325112869605, 1.000000000000000000, 0.9238795325112869605, 1.000000000000000000, 0.9238795325112869605, 1.000000000000000000, 0.9238795325112869605, 1.000000000000000000, 0.9238795325112869605, 1.000000000000000000, 0.9238795325112869605, 1.000000000000000000, 0.9238795325112869605, 1.000000000000000000, 0.9238795325112869605, 1.000000000000000000, 0.9238795325112869605, 1.000000000000000000, 0.9238795325112869605, 1.000000000000000000, 0.9238795325112869605, 1.000000000000000000, 0.9238795325112869605, 1.000000000000000000, 0.9238795325112869605, 1.000000000000000000, 0.9238795325112869605, 1.000000000000000000, 0.9238795325112869605, 1.000000000000000000),
 ( 1.000000000000000000, 0.9238795325112869605, 1.000000000000000000, 0.9238795325112869605, 1.000000000000000000, 0.9238795325112869605, 1.000000000000000000, 0.9238795325112869605, 1.000000000000000000, 0.9238795325112869605, 1.000000000000000000, 0.9238795325112869605, 1.000000000000000000, 0.9238795325112869605, 1.000000000000000000, 0.9238795325112869605, 1.000000000000000000, 0.9238795325112869605, 1.000000000000000000, 0.9238795325112869605, 1.000000000000000000, 0.9238795325112869605, 1.000000000000000000, 0.9238795325112869605, 1.000000000000000000, 0.9238795325112869605, 1.000000000000000000, 0.9238795325112869605, 1.000000000000000000, 0.9238795325112869605, 1.000000000000000000, 0.9238795325112869605, 1.000000000000000000, 0.9238795325112869605, 1.000000000000000000, 0.9238795325112869605, 1.000000000000000000, 0.9238795325112869605, 1.000000000000000000, 0.9238795325112869605, 1.000000000000000000, 0.9238795325112869605, 1.000000000000000000, 0.9238795325112869605, 1.000000000000000000, 0.9238795325112869605, 1.000000000000000000, 0.9238795325112869605, 1.000000000000000000, 0.9238795325112869605, 1.000000000000000000, 0.9238795325112869605, 1.000000000000000000, 0.9238795325112869605, 1.000000000000000000, 0.9238795325112869605, 1.000000000000000000, 0.9238795325112869605, 1.000000000000000000, 0.9238795325112869605, 1.000000000000000000, 0.9238795325112869605, 1.000000000000000000, 0.9238795325112869605, 1.000000000000000000, 0.9238795325112869605, 1.000000000000000000, 0.9238795325112869605, 1.000000000000000000, 0.9238795325112869605, 1.000000000000000000, 0.9238795325112869605, 1.000000000000000000, 0.9238795325112869605, 1.000000000000000000, 0.9238795325112869605, 1.000000000000000000, 0.9238795325112869605, 1.000000000000000000, 0.9238795325112869605, 1.000000000000000000, 0.9238795325112869605, 1.000000000000000000, 0.9238795325112869605, 1.000000000000000000, 0.9238795325112869605, 1.000000000000000000, 0.9238795325112869605, 1.000000000000000000, 0.9238795325112869605, 1.000000000000000000, 0.9238795325112869605, 1.000000000000000000, 0.9238795325112869605, 1.000000000000000000, 0.9238795325112869605, 1.000000000000000000, 0.9238795325112869605, 1.000000000000000000, 0.9238795325112869605, 1.000000000000000000, 0.9238795325112869605, 1.000000000000000000, 0.9238795325112869605, 1.000000000000000000, 0.9238795325112869605, 1.000000000000000000, 0.9238795325112869605, 1.000000000000000000, 0.9238795325112869605, 1.000000000000000000, 0.9238795325112869605, 1.000000000000000000, 0.9238795325112869605, 1.000000000000000000, 0.9238795325112869605, 1.000000000000000000, 0.9238795325112869605, 1.000000000000000000, 0.9238795325112869605, 1.000000000000000000, 0.9238795325112869605, 1.000000000000000000, 0.9238795325112869605, 1.000000000000000000, 0.9238795325112869605, 1.000000000000000000, 0.9238795325112869605, 1.000000000000000000, 0.9238795325112869605, 1.000000000000000000, 0.9238795325112869605, 1.000000000000000000, 0.9238795325112869605, 1.000000000000000000, 0.9238795325112869605, 1.000000000000000000, 0.9238795325112869605, 1.000000000000000000, 0.9238795325112869605, 1.000000000000000000, 0.9238795325112869605, 1.000000000000000000, 0.9238795325112869605, 1.000000000000000000, 0.9238795325112869605, 1.000000000000000000, 0.9238795325112869605, 1.000000000000000000, 0.9238795325112869605, 1.000000000000000000, 0.9238795325112869605, 1.000000000000000000, 0.9238795325112869605, 1.000000000000000000, 0.9238795325112869605, 1.000000000000000000, 0.9238795325112869605, 1.000000000000000000, 0.9238795325112869605, 1.000000000000000000, 0.9238795325112869605, 1.000000000000000000, 0.9238795325112869605, 1.000000000000000000, 0.9238795325112869605, 1.000000000000000000, 0.9238795325112869605, 1.000000000000000000, 0.9238795325112869605, 1.000000000000000000, 0.9238795325112869605, 1.000000000000000000, 0.9238795325112869605, 1.000000000000000000, 0.9238795325112869605, 1.000000000000000000, 0.9238795325112869605, 1.000000000000000000, 0.9238795325112869605, 1.000000000000000000, 0.9238795325112869605, 1.000000000000000000, 0.9238795325112869605, 1.000000000000000000, 0.9238795325112869605, 1.000000000000000000, 0.9238795325112869605, 1.000000000000000000, 0.9238795325112869605, 1.000000000000000000, 0.9238795325112869605, 1.000000000000000000, 0.9238795325112869605, 1.000000000000000000, 0.9238795325112869605, 1.000000000000000000, 0.9238795325112869605, 1.000000000000000000, 0.9238795325112869605, 1.000000000000000000, 0.9238795325112869605, 1.000000000000000000, 0.9238795325112869605, 1.000000000000000000, 0.9238795325112869605, 1.000000000000000000, 0.9238795325112869605, 1.000000000000000000, 0.9238795325112869605, 1.000000000000000000, 0.9238795325112869605, 1.000000000000000000, 0.9238795325112869605, 1.000000000000000000, 0.9238795325112869605, 1.000000000000000000, 0.9238795325112869605, 1.000000000000000000, 0.9238795325112869605, 1.000000000000000000, 0.9238795325112869605, 1.000000000000000000, 0.9238795325112869605, 1.000000000000000000, 0.9238795325112869605, 1.000000000000000000, 0.9238795325112869605, 1.000000000000000000, 0.9238795325112869605, 1.000000000000000000, 0.9238795325112869605, 1.000000000000000000, 0.9238795325112869605, 1.000000000000000000, 0.9238795325112869605, 1.000000000000000000, 0.9238795325112869605, 1.000000000000000000, 0.9238795325112869605, 1.000000000000000000, 0.9238795325112869605, 1.000000000000000000, 0.9238795325112869605, 1.000000000000000000, 0.9238795325112869605, 1.000000000000000000, 0.9238795325112869605, 1.000000000000000000, 0.9238795325112869605, 1.000000000000000000, 0.9238795325112869605, 1.000000000000000000, 0.9238795325112869605, 1.000000000000000000, 0.9238795325112869605, 1.000000000000000000) ) ) 
 REPRESENTATION_ITEM ( '' )  SURFACE ( )  );
#18035 = CARTESIAN_POINT ( 'NONE',  ( 70.19189222814998175, -59.11650476797663600, -36.84940499091918298 ) ) ;
#18036 = CARTESIAN_POINT ( 'NONE',  ( 118.9794681442453026, -9.261995988541697145, -16.69588392320189030 ) ) ;
#18037 = VERTEX_POINT ( 'NONE', #16997 ) ;
#18038 = ORIENTED_EDGE ( 'NONE', *, *, #32620, .T. ) ;
#18039 = DIRECTION ( 'NONE',  ( 0.000000000000000000, -0.3818493186865927203, 0.9242245927363029745 ) ) ;
#18040 = CARTESIAN_POINT ( 'NONE',  ( 116.3166296295247832, -4.863998795839590272, -19.15521520033831493 ) ) ;
#18041 = CARTESIAN_POINT ( 'NONE',  ( 112.3578015045248861, -6.936859964151250502, -18.39754474579286025 ) ) ;
#18042 = CARTESIAN_POINT ( 'NONE',  ( 111.1076452545248259, -9.868328341294098749, -15.46607636864997204 ) ) ;
#18043 = CARTESIAN_POINT ( 'NONE',  ( 112.4272546295247821, -4.863998795839590272, -18.39754474579285315 ) ) ;
#18044 = CIRCLE ( 'NONE', #5629, 6.479565957685750277 ) ;
#18045 = CARTESIAN_POINT ( 'NONE',  ( 124.2550481442452792, -9.988377603198980381, -10.36322818467138518 ) ) ;
#18046 = CARTESIAN_POINT ( 'NONE',  ( 112.8529881442453302, -1.561330072975668060, -17.79121239304076596 ) ) ;
#18047 = ORIENTED_EDGE ( 'NONE', *, *, #2756, .F. ) ;
#18048 = EDGE_CURVE ( 'NONE', #16022, #10767, #14822, .T. ) ;
#18049 = CARTESIAN_POINT ( 'NONE',  ( 113.7606148109119886, -7.894159318335828068, -9.358103419637847864 ) ) ;
#18050 = CARTESIAN_POINT ( 'NONE',  ( 107.6349890045248401, 0.8980012041604421569, -15.77991374673208469 ) ) ;
#18051 = CARTESIAN_POINT ( 'NONE',  ( 119.2631014775786440, -9.565557343593393824, -10.61323700422344274 ) ) ;
#18052 = CARTESIAN_POINT ( 'NONE',  ( 112.1722681442453222, -8.899110576539710493, -16.42337572283490132 ) ) ;
#18053 = EDGE_CURVE ( 'NONE', #2987, #39376, #13378, .T. ) ;
#18054 = ADVANCED_FACE ( 'NONE', ( #37950 ), #40302, .T. ) ;
#18055 = CARTESIAN_POINT ( 'NONE',  ( 124.7088614775786226, 0.2603800115204892296, -16.42320221600525088 ) ) ;
#18056 = CARTESIAN_POINT ( 'NONE',  ( 79.05243529145373316, 4.793396140045460108, -5.736853407927685389 ) ) ;
#18057 = CARTESIAN_POINT ( 'NONE',  ( 117.5613014775786525, 0.9020085738987339008, -11.91225656197089222 ) ) ;
#18058 = CARTESIAN_POINT ( 'NONE',  ( 115.6220983795247861, -0.7896495226426338832, -9.318865927141430916 ) ) ;
#18059 = CARTESIAN_POINT ( 'NONE',  ( 111.3160046295247838, -4.863998795839590272, -18.39754474579285315 ) ) ;
#18060 = ORIENTED_EDGE ( 'NONE', *, *, #40755, .T. ) ;
#18061 = CARTESIAN_POINT ( 'NONE',  ( 70.19189222814998175, -52.61716011954800365, -34.24968978710501943 ) ) ;
#18062 = CARTESIAN_POINT ( 'NONE',  ( 114.6682414775786469, -7.894159318335828068, -9.358103419637847864 ) ) ;
#18063 = CARTESIAN_POINT ( 'NONE',  ( 112.2289948109119848, -1.834011780172310813, -8.268836392978581529 ) ) ;
#18064 = CARTESIAN_POINT ( 'NONE',  ( 111.9453614775786434, -1.561330072975668060, -17.79121239304076596 ) ) ;
#18065 = CARTESIAN_POINT ( 'NONE',  ( 118.4689281442453250, -10.15424416112534622, -14.75197769757730448 ) ) ;
#18066 = CARTESIAN_POINT ( 'NONE',  ( 121.4187148109119789, -3.505236298600246325, -18.68346056562440793 ) ) ;
#18067 = CARTESIAN_POINT ( 'NONE',  ( 117.1074881442453233, 0.4262465694468514643, -12.03445270309931736 ) ) ;
#18068 = ORIENTED_EDGE ( 'NONE', *, *, #33209, .T. ) ;
#18069 = CARTESIAN_POINT ( 'NONE',  ( 120.3685329359119862, -5.367793381288652910, -18.78638297431638904 ) ) ;
#18070 = CARTESIAN_POINT ( 'NONE',  ( 67.30914723170953096, -60.66501133130886814, -38.36331010974746647 ) ) ;
#18071 = CARTESIAN_POINT ( 'NONE',  ( 114.6115148109119986, -6.222761293078241884, -8.102969835052219238 ) ) ;
#18072 = ORIENTED_EDGE ( 'NONE', *, *, #8181, .T. ) ;
#18073 = FACE_OUTER_BOUND ( 'NONE', #33737, .T. ) ;
#18074 = CARTESIAN_POINT ( 'NONE',  ( 106.7320983795247855, -0.7896495226426338832, -9.318865927141430916 ) ) ;
#18075 = CARTESIAN_POINT ( 'NONE',  ( 111.1076452545248259, -9.868328341294098749, -15.46607636864997204 ) ) ;
#18076 = CARTESIAN_POINT ( 'NONE',  ( 124.4819548109119722, -2.084020599724406786, -8.691656652584148546 ) ) ;
#18077 = EDGE_CURVE ( 'NONE', #32023, #12824, #18867, .T. ) ;
#18078 = VERTEX_POINT ( 'NONE', #28537 ) ;
#18079 = CARTESIAN_POINT ( 'NONE',  ( 117.7882081442453170, -3.505236298600246325, -18.68346056562440793 ) ) ;
#18080 = AXIS2_PLACEMENT_3D ( 'NONE', #36883, #43978, #5203 ) ;
#18081 = CARTESIAN_POINT ( 'NONE',  ( 116.5969481442453031, -9.859900752359374465, -12.68260735090039404 ) ) ;
#18082 = CARTESIAN_POINT ( 'NONE',  ( 124.5529552597880638, -9.864862387977231251, -13.33873797166363318 ) ) ;
#18083 = EDGE_CURVE ( 'NONE', #30411, #12824, #27641, .T. ) ;
#18084 = CARTESIAN_POINT ( 'NONE',  ( 121.7575954359119805, -11.07370829466463569, -12.81314460846529002 ) ) ;
#18085 = VERTEX_POINT ( 'NONE', #27476 ) ;
#18086 = FACE_OUTER_BOUND ( 'NONE', #35555, .T. ) ;
#18087 = CARTESIAN_POINT ( 'NONE',  ( 124.9542645564587247, -2.361164406680991146, -6.193652130325402183 ) ) ;
#18088 = EDGE_CURVE ( 'NONE', #26016, #35384, #16768, .T. ) ;
#18089 = CARTESIAN_POINT ( 'NONE',  ( 110.4825671295247815, -10.62599879583958540, -13.39321520033831447 ) ) ;
#18090 = CARTESIAN_POINT ( 'NONE',  ( 112.3991748109119868, -8.166667518702817929, -8.995218007635859436 ) ) ;
#18091 = CARTESIAN_POINT ( 'NONE',  ( 112.1722681442453222, -0.4660016031367893996, -10.09054647747474043 ) ) ;
#18092 = CARTESIAN_POINT ( 'NONE',  ( 116.3133148109120043, -2.084020599724406786, -8.691656652584148546 ) ) ;
#18093 = VERTEX_POINT ( 'NONE', #25113 ) ;
#18094 = CARTESIAN_POINT ( 'NONE',  ( 117.8449348109119938, -1.833838273342659253, -17.42832698103878286 ) ) ;
#18095 = CARTESIAN_POINT ( 'NONE',  ( 115.1359265045248605, -7.250697342233347165, -19.15521520033831138 ) ) ;
#18096 = CARTESIAN_POINT ( 'NONE',  ( 126.2184548109119788, -4.863998795839242995, -13.39321520033831447 ) ) ;
#18097 = DIRECTION ( 'NONE',  ( 0.7871354856660167654, -0.6167752151498625546, -0.002461946824136807422 ) ) ;
#18098 = CARTESIAN_POINT ( 'NONE',  ( 115.4624148109119943, -5.638512984488999180, -18.83840828888717311 ) ) ;
#18099 = ORIENTED_EDGE ( 'NONE', *, *, #16161, .F. ) ;
#18100 = EDGE_CURVE ( 'NONE', #2538, #39913, #6365, .T. ) ;
#18101 = CARTESIAN_POINT ( 'NONE',  ( 118.4122014775786340, 0.5811942927096110934, -14.16772938898807510 ) ) ;
#18102 = DIRECTION ( 'NONE',  ( -0.000000000000000000, -0.9284778069183721172, -0.3713878862591650232 ) ) ;
#18103 = CARTESIAN_POINT ( 'NONE',  ( 110.9687390045248350, 0.8980012041604421569, -15.77991374673208469 ) ) ;
#18104 = CARTESIAN_POINT ( 'NONE',  ( 116.9373081442452929, -8.166667518702817929, -8.995218007635861213 ) ) ;
#18105 = EDGE_CURVE ( 'NONE', #28442, #9192, #38825, .T. ) ;
#18106 = EDGE_CURVE ( 'NONE', #1972, #27420, #19184, .T. ) ;
#18107 = CARTESIAN_POINT ( 'NONE',  ( 115.3489614775786407, -9.261995988541697145, -16.69588392320189030 ) ) ;
#18108 = CARTESIAN_POINT ( 'NONE',  ( 126.2184548109105435, -9.814174330883648878, -12.68911139247483710 ) ) ;
#18109 = DIRECTION ( 'NONE',  ( 0.000000000000000000, -0.3818493186865936084, 0.9242245927363024194 ) ) ;
#18110 = CARTESIAN_POINT ( 'NONE',  ( 109.9269421295247753, -9.868328341294093420, -13.39321520033831447 ) ) ;
#18111 = VERTEX_POINT ( 'NONE', #32825 ) ;
#18112 = CARTESIAN_POINT ( 'NONE',  ( 121.9470836909669913, -24.14644159042263993, -12.62951656296512937 ) ) ;
#18113 = CARTESIAN_POINT ( 'NONE',  ( 109.2294421295618321, -7.227482384100928137, -18.13879607630843793 ) ) ;
#18114 = CARTESIAN_POINT ( 'NONE',  ( 116.5969481442453031, -9.859900752359374465, -12.68260735090039404 ) ) ;
#18115 = CARTESIAN_POINT ( 'NONE',  ( 64.40208719633689327, -13.04080931321579406, -11.16048930627172808 ) ) ;
#18116 = CARTESIAN_POINT ( 'NONE',  ( 116.3166296295247832, -4.863998795839590272, -8.388885654883775800 ) ) ;
#18117 = CARTESIAN_POINT ( 'NONE',  ( 106.1070202545248407, -10.62599879583958717, -15.77991374673208469 ) ) ;
#18118 = FACE_OUTER_BOUND ( 'NONE', #2702, .T. ) ;
#18119 = CARTESIAN_POINT ( 'NONE',  ( 114.8951481442453115, -8.899110576539710493, -16.42337572283490132 ) ) ;
#18120 = CARTESIAN_POINT ( 'NONE',  ( 120.3976348109119812, -7.643976991954104960, -18.09477374809246442 ) ) ;
#18121 = CARTESIAN_POINT ( 'NONE',  ( 122.9503348109119827, 0.5811942927096110934, -14.16772938898807510 ) ) ;
#18122 = CARTESIAN_POINT ( 'NONE',  ( 114.4980614775786592, -7.893985811506177619, -18.51759400769804742 ) ) ;
#18123 = ORIENTED_EDGE ( 'NONE', *, *, #22814, .F. ) ;
#18124 = CARTESIAN_POINT ( 'NONE',  ( 114.5547881442453217, -4.153390946401321671, -8.397313243818183892 ) ) ;
#18125 = LINE ( 'NONE', #14706, #40005 ) ;
#18126 = CARTESIAN_POINT ( 'NONE',  ( 117.9583881442453048, -10.30919188438810075, -12.61870101168855918 ) ) ;
#18127 =( BOUNDED_CURVE ( )  B_SPLINE_CURVE ( 2, ( #41408, #14243, #24724, #41179, #3304, #10164, #3741, #31118, #20865, #30900, #6281, #3524, #27937, #45042, #24294, #41628, #34085 ),
 .UNSPECIFIED., .F., .F. ) 
 B_SPLINE_CURVE_WITH_KNOTS ( ( 3, 2, 2, 2, 2, 2, 2, 2, 3 ),
 ( 0.4035091206787220219, 0.4124999999999999778, 0.4249999999999999889, 0.4375000000000000000, 0.4500000000000000111, 0.4625000000000000222, 0.4749999999999999778, 0.4874999999999999889, 0.4964908793212780003 ),
 .UNSPECIFIED. ) 
 CURVE ( )  GEOMETRIC_REPRESENTATION_ITEM ( )  RATIONAL_B_SPLINE_CURVE ( ( 0.9692594319298230010, 0.9452488050343769155, 1.000000000000000000, 0.9238795325112869605, 1.000000000000000000, 0.9238795325112869605, 1.000000000000000000, 0.9238795325112869605, 1.000000000000000000, 0.9238795325112869605, 1.000000000000000000, 0.9238795325112869605, 1.000000000000000000, 0.9238795325112869605, 1.000000000000000000, 0.9452488050343769155, 0.9692594319298220018 ) ) 
 REPRESENTATION_ITEM ( '' )  );
#18128 = CARTESIAN_POINT ( 'NONE',  ( 119.1496481442453046, -6.222761293078241884, -8.102969835052219238 ) ) ;
#18129 = ORIENTED_EDGE ( 'NONE', *, *, #20701, .F. ) ;
#18130 = CARTESIAN_POINT ( 'NONE',  ( 122.6099748109119929, -0.8288870151387760510, -10.36305467784173118 ) ) ;
#18131 = CARTESIAN_POINT ( 'NONE',  ( 115.5191414775786569, -3.383040157471821630, -19.15922257007629170 ) ) ;
#18132 = CARTESIAN_POINT ( 'NONE',  ( 137.3645353335808750, 0.1036370839169628438, -14.77667914328649879 ) ) ;
#18133 = CARTESIAN_POINT ( 'NONE',  ( 108.6073327545248048, -2.477300249445798297, -19.15521520033831138 ) ) ;
#18134 = CYLINDRICAL_SURFACE ( 'NONE', #26422, 20.00000000000000000 ) ;
#18135 = CARTESIAN_POINT ( 'NONE',  ( 126.2807669870676648, 0.1502658026859126084, -13.80526545341719036 ) ) ;
#18136 = CARTESIAN_POINT ( 'NONE',  ( 115.3442858795247759, -8.402594152722688392, -9.854619843455216355 ) ) ;
#18137 = CARTESIAN_POINT ( 'NONE',  ( 116.4267681442453153, -3.383040157471821630, -19.15922257007629170 ) ) ;
#18138 = CIRCLE ( 'NONE', #20341, 3.000000000000003997 ) ;
#18139 = CIRCLE ( 'NONE', #10896, 1.499999999999996225 ) ;
#18140 = CARTESIAN_POINT ( 'NONE',  ( 136.7478768735761321, -10.46432003856224568, -13.90125341227964917 ) ) ;
#18141 = CARTESIAN_POINT ( 'NONE',  ( 116.3133148109120043, -2.084020599724406786, -8.691656652584148546 ) ) ;
#18142 = DIRECTION ( 'NONE',  ( 0.000000000000000000, -0.4669533266896288004, -0.8842819633428519177 ) ) ;
#18143 = EDGE_CURVE ( 'NONE', #1626, #43799, #4592, .T. ) ;
#18144 = CARTESIAN_POINT ( 'NONE',  ( 117.2776681442452968, -4.153390946401313677, -8.397313243818183892 ) ) ;
#18145 = CARTESIAN_POINT ( 'NONE',  ( 113.2606921295247702, -9.868328341294093420, -13.39321520033831447 ) ) ;
#18146 = FACE_OUTER_BOUND ( 'NONE', #13553, .T. ) ;
#18147 = DIRECTION ( 'NONE',  ( 1.000000000000000000, 0.000000000000000000, -0.000000000000000000 ) ) ;
#18148 = DIRECTION ( 'NONE',  ( -0.8949343913984425525, 0.1703803081152066579, -0.4123869368673873104 ) ) ;
#18150 = CARTESIAN_POINT ( 'NONE',  ( 117.7314814775786260, -4.089484607189486809, -7.948022111789456723 ) ) ;
#18149 = CARTESIAN_POINT ( 'NONE',  ( 62.73792221385235734, -14.56781324038501602, -8.049265019886933104 ) ) ;
#18151 = CARTESIAN_POINT ( 'NONE',  ( 117.6747548109119919, -7.643976991954077427, -18.09477374809248928 ) ) ;
#18152 = CARTESIAN_POINT ( 'NONE',  ( 125.3328548109119964, -9.261995988541697145, -16.69588392320189030 ) ) ;
#18153 = ORIENTED_EDGE ( 'NONE', *, *, #3058, .T. ) ;
#18154 = LINE ( 'NONE', #31829, #39163 ) ;
#18155 = CARTESIAN_POINT ( 'NONE',  ( 123.3474214775786209, -9.988377603198976828, -10.36322818467138340 ) ) ;
#18156 = CARTESIAN_POINT ( 'NONE',  ( 116.1082702545247827, 0.1403307496149616695, -11.32035403202665336 ) ) ;
#18157 = CARTESIAN_POINT ( 'NONE',  ( 119.1496481442453046, -6.222761293078241884, -8.102969835052219238 ) ) ;
#18158 = CARTESIAN_POINT ( 'NONE',  ( 117.6747548109119919, -7.643976991954077427, -18.09477374809248928 ) ) ;
#18159 = CARTESIAN_POINT ( 'NONE',  ( 86.21301144467663846, -26.71832258603155807, -8.459175720980109503 ) ) ;
#18160 = CARTESIAN_POINT ( 'NONE',  ( 112.7745202545247878, -10.62599879583958717, -15.77991374673208469 ) ) ;
#18161 = CARTESIAN_POINT ( 'NONE',  ( 121.7023481442452919, -0.8288870151387760510, -10.36305467784173118 ) ) ;
#18162 = CARTESIAN_POINT ( 'NONE',  ( 122.4965214775786251, 0.1319031606808879209, -14.10382304977623669 ) ) ;
#18163 = CARTESIAN_POINT ( 'NONE',  ( 114.7249681442453237, -9.565557343593411588, -10.61323700422346583 ) ) ;
#18164 = CARTESIAN_POINT ( 'NONE',  ( 109.2294819584304548, -4.447028745678551331, -7.844385157708282819 ) ) ;
#18165 = CARTESIAN_POINT ( 'NONE',  ( 121.9659548109119811, -2.527210466738041728, -8.967976844669124148 ) ) ;
#18166 = CARTESIAN_POINT ( 'NONE',  ( 115.4831921295247952, 0.8980012041604618078, -13.39321520033831447 ) ) ;
#18167 = DIRECTION ( 'NONE',  ( 0.000000000000000000, 0.000000000000000000, -1.000000000000000000 ) ) ;
#18168 = CARTESIAN_POINT ( 'NONE',  ( 117.0507614775786465, -10.30919188438810075, -12.61870101168855918 ) ) ;
#18169 = CARTESIAN_POINT ( 'NONE',  ( 117.7882081442453170, -6.344957434206665248, -7.627207830600338134 ) ) ;
#18170 = CARTESIAN_POINT ( 'NONE',  ( 113.0523327545247838, -2.477300249445798297, -19.15521520033831138 ) ) ;
#18171 = EDGE_CURVE ( 'NONE', #17900, #40637, #29171, .T. ) ;
#18172 = CARTESIAN_POINT ( 'NONE',  ( 113.1933481442453058, -4.089484607189486809, -7.948022111789456723 ) ) ;
#18173 = ORIENTED_EDGE ( 'NONE', *, *, #34453, .F. ) ;
#18174 = CARTESIAN_POINT ( 'NONE',  ( 59.90552009294157898, -2.897503654462289191, -17.89321520033831447 ) ) ;
#18175 = CARTESIAN_POINT ( 'NONE',  ( 117.7882081442453170, -6.344957434206665248, -7.627207830600338134 ) ) ;
#18176 = CIRCLE ( 'NONE', #26933, 2.000000000000000444 ) ;
#18177 = CARTESIAN_POINT ( 'NONE',  ( 122.2128881442453263, -7.643976991954077427, -18.09477374809248928 ) ) ;
#18178 =( NAMED_UNIT ( * ) PLANE_ANGLE_UNIT ( ) SI_UNIT ( $, .RADIAN. ) );
#18179 = AXIS2_PLACEMENT_3D ( 'NONE', #35291, #652, #21185 ) ;
#18180 = CARTESIAN_POINT ( 'NONE',  ( 124.4252281442452812, -9.261995988541697145, -16.69588392320189030 ) ) ;
#18181 = CARTESIAN_POINT ( 'NONE',  ( 122.3263414775786373, -6.344957434206665248, -7.627207830600338134 ) ) ;
#18182 = CARTESIAN_POINT ( 'NONE',  ( 112.0799890045248475, 0.8980012041604421569, -15.77991374673208469 ) ) ;
#18183 = CARTESIAN_POINT ( 'NONE',  ( 114.6115148109119986, -6.222761293078241884, -8.102969835052219238 ) ) ;
#18184 = CARTESIAN_POINT ( 'NONE',  ( 121.5492360609119800, -6.564341423271550902, -7.887810678476487425 ) ) ;
#18185 = CARTESIAN_POINT ( 'NONE',  ( 63.69189222814998175, -50.16718729050181480, -4.893215200338314474 ) ) ;
#18186 = VERTEX_POINT ( 'NONE', #11436 ) ;
#18187 = CARTESIAN_POINT ( 'NONE',  ( 121.5888948109119809, -10.30919188438810075, -12.61870101168855918 ) ) ;
#18188 = CARTESIAN_POINT ( 'NONE',  ( 123.8411891859119862, -8.844754642576884152, -8.592115655440050404 ) ) ;
#18189 = CARTESIAN_POINT ( 'NONE',  ( 120.3409081442453044, -0.4660016031367893996, -10.09054647747474043 ) ) ;
#18190 = ORIENTED_EDGE ( 'NONE', *, *, #42098, .T. ) ;
#18191 = CARTESIAN_POINT ( 'NONE',  ( 125.5597614775786326, -7.894159318335828068, -9.358103419637847864 ) ) ;
#18192 = CARTESIAN_POINT ( 'NONE',  ( -12.36826994950263980, -4.374949827406455327, -7.393215200338315363 ) ) ;
#18193 = CARTESIAN_POINT ( 'NONE',  ( 119.7177477074048966, -2.419733177069661512, -17.89711025544711376 ) ) ;
#18194 = CARTESIAN_POINT ( 'NONE',  ( 114.4413348109119823, -0.8288870151387760510, -10.36305467784173118 ) ) ;
#18195 = DIRECTION ( 'NONE',  ( 0.000000000000000000, 0.9284778069183720062, 0.3713878862591650232 ) ) ;
#18196 = CARTESIAN_POINT ( 'NONE',  ( 64.70066334234053329, -35.74738352678537012, -5.786960771376285173 ) ) ;
#18197 = CARTESIAN_POINT ( 'NONE',  ( 118.0718414775786442, -0.8288870151387760510, -10.36305467784173118 ) ) ;
#18198 = CARTESIAN_POINT ( 'NONE',  ( 115.9294421295247872, -10.76310523276723785, -4.893215200338314474 ) ) ;
#18199 = CARTESIAN_POINT ( 'NONE',  ( 120.6812681442452941, 0.1319031606808879209, -14.10382304977623669 ) ) ;
#18200 = CIRCLE ( 'NONE', #19666, 2.999999999999999556 ) ;
#18201 = DIRECTION ( 'NONE',  ( -1.000000000000000000, 0.000000000000000000, 0.000000000000000000 ) ) ;
#18202 = CARTESIAN_POINT ( 'NONE',  ( 119.0929214775786278, -4.153390946401325223, -8.397313243818185668 ) ) ;
#18203 = CARTESIAN_POINT ( 'NONE',  ( 114.7816948109119863, 0.5811942927096154232, -14.16772938898807155 ) ) ;
#18204 = CARTESIAN_POINT ( 'NONE',  ( 120.3409081442453044, -0.4660016031367893996, -10.09054647747474043 ) ) ;
#18205 = CARTESIAN_POINT ( 'NONE',  ( 113.6471614775786492, -5.638512984488999180, -18.83840828888717311 ) ) ;
#18206 = DIRECTION ( 'NONE',  ( 0.9609149988134837450, -0.1028163501681639419, 0.2570431154366518145 ) ) ;
#18207 = CARTESIAN_POINT ( 'NONE',  ( 121.7590748109119687, -2.084020599724406786, -8.691656652584148546 ) ) ;
#18208 = ORIENTED_EDGE ( 'NONE', *, *, #40630, .T. ) ;
#18209 = CARTESIAN_POINT ( 'NONE',  ( 121.5888948109119809, -10.30919188438810075, -12.61870101168855918 ) ) ;
#18210 = CARTESIAN_POINT ( 'NONE',  ( 111.7327233795247849, -1.325403438956436419, -9.854619843455211026 ) ) ;
#18211 = DIRECTION ( 'NONE',  ( 0.000000000000000000, 0.000000000000000000, -1.000000000000000000 ) ) ;
#18212 = CARTESIAN_POINT ( 'NONE',  ( 114.7192077545248452, -2.791137627527887410, -18.39754474579284249 ) ) ;
#18213 = CONICAL_SURFACE ( 'NONE', #43705, 1.610000000000000986, 0.9599310885968765916 ) ;
#18214 = EDGE_CURVE ( 'NONE', #21938, #40512, #35659, .T. ) ;
#18215 = DIRECTION ( 'NONE',  ( 0.000000000000000000, 0.000000000000000000, -1.000000000000000000 ) ) ;
#18216 = CARTESIAN_POINT ( 'NONE',  ( 126.2404814775786264, -9.261995988541697145, -16.69588392320189030 ) ) ;
#18217 = ORIENTED_EDGE ( 'NONE', *, *, #15156, .T. ) ;
#18218 = AXIS2_PLACEMENT_3D ( 'NONE', #21452, #35335, #18028 ) ;
#18219 = CARTESIAN_POINT ( 'NONE',  ( 64.46696884418977902, -15.35047623416358142, -10.89321734395795893 ) ) ;
#18220 = CARTESIAN_POINT ( 'NONE',  ( 123.1205148109119563, -7.643976991954077427, -18.09477374809248928 ) ) ;
#18221 = COLOUR_RGB ( '',0.7921568627450980005, 0.8196078431372548767, 0.9333333333333333481 ) ;
#18222 = CARTESIAN_POINT ( 'NONE',  ( 120.2990798109119766, -2.173413727453600508, -8.297982527556802879 ) ) ;
#18223 = CARTESIAN_POINT ( 'NONE',  ( 66.01377532187956376, -14.50698776528348688, -16.72205822936306063 ) ) ;
#18224 = PLANE ( 'NONE',  #6438 ) ;
#18225 = CARTESIAN_POINT ( 'NONE',  ( 109.9269421295247753, -9.868328341294093420, -13.39321520033831447 ) ) ;
#18226 = ORIENTED_EDGE ( 'NONE', *, *, #3885, .F. ) ;
#18227 = CARTESIAN_POINT ( 'NONE',  ( 114.8384214775786489, 0.9020085738987339008, -11.91225656197089222 ) ) ;
#18228 = CARTESIAN_POINT ( 'NONE',  ( 115.1220548109119761, -8.166667518702817929, -8.995218007635861213 ) ) ;
#18229 = CARTESIAN_POINT ( 'NONE',  ( 88.68444135278477347, -11.19878434816932611, -14.07504941314370406 ) ) ;
#18230 = CARTESIAN_POINT ( 'NONE',  ( 121.5321681442453183, -0.1624402480850797581, -16.17319339645315424 ) ) ;
#18231 = CARTESIAN_POINT ( 'NONE',  ( 126.9276200068654674, -3.142429669179889196, -8.322895171908893275 ) ) ;
#18232 = CARTESIAN_POINT ( 'NONE',  ( 121.8158014775786171, -5.638512984488999180, -18.83840828888717311 ) ) ;
#18233 = CARTESIAN_POINT ( 'NONE',  ( 112.0020881442453344, -9.565557343593413364, -10.61323700422348004 ) ) ;
#18234 = LINE ( 'NONE', #14365, #20129 ) ;
#18235 = DIRECTION ( 'NONE',  ( 1.000000000000000000, 0.000000000000000000, -0.000000000000000000 ) ) ;
#18236 = CARTESIAN_POINT ( 'NONE',  ( 111.9453614775786434, -1.561330072975668060, -17.79121239304076596 ) ) ;
#18237 = ORIENTED_EDGE ( 'NONE', *, *, #15015, .T. ) ;
#18238 = DIRECTION ( 'NONE',  ( 1.000000000000000000, 0.000000000000000000, -0.000000000000000000 ) ) ;
#18239 = AXIS2_PLACEMENT_3D ( 'NONE', #21966, #18548, #17873 ) ;
#18240 = EDGE_CURVE ( 'NONE', #21444, #41351, #27197, .T. ) ;
#18241 = CARTESIAN_POINT ( 'NONE',  ( 120.9649014775786355, -3.383040157471821630, -19.15922257007629170 ) ) ;
#18242 = CARTESIAN_POINT ( 'NONE',  ( 70.19189222814998175, -66.90480655070588512, -34.57954022122791571 ) ) ;
#18243 = ORIENTED_EDGE ( 'NONE', *, *, #6936, .F. ) ;
#18244 = CARTESIAN_POINT ( 'NONE',  ( 121.3820794150595930, -2.423081321603731908, -17.89265170041263175 ) ) ;
#18245 = CARTESIAN_POINT ( 'NONE',  ( 112.1722681442453222, -8.899110576539710493, -16.42337572283490132 ) ) ;
#18246 = DIRECTION ( 'NONE',  ( -1.000000000000000000, 0.000000000000000000, 0.000000000000000000 ) ) ;
#18247 = CARTESIAN_POINT ( 'NONE',  ( 124.6521348109119884, -7.894159318335828068, -9.358103419637847864 ) ) ;
#18248 = ORIENTED_EDGE ( 'NONE', *, *, #40084, .F. ) ;
#18249 = AXIS2_PLACEMENT_3D ( 'NONE', #31569, #39985, #29499 ) ;
#18250 = CARTESIAN_POINT ( 'NONE',  ( 118.2987481442453088, -1.561330072975668504, -17.79121239304076951 ) ) ;
#18251 = LINE ( 'NONE', #29182, #13930 ) ;
#18252 = AXIS2_PLACEMENT_3D ( 'NONE', #8134, #22035, #29097 ) ;
#18253 = CYLINDRICAL_SURFACE ( 'NONE', #22941, 1.199999999999999512 ) ;
#18254 = CARTESIAN_POINT ( 'NONE',  ( 111.4556253487318997, -2.476252568991189396, -17.82184623478305596 ) ) ;
#18255 = CARTESIAN_POINT ( 'NONE',  ( 111.5482748109120053, -0.1624402480850797581, -16.17319339645315424 ) ) ;
#18256 = CARTESIAN_POINT ( 'NONE',  ( 77.77634386988368931, 3.254514819260763581, -7.393215200338315363 ) ) ;
#18257 = DIRECTION ( 'NONE',  ( -0.9908103287288504424, 0.1352586133457950035, 0.000000000000000000 ) ) ;
#18258 = CARTESIAN_POINT ( 'NONE',  ( 125.2194014775786286, -10.30919188438810075, -12.61870101168855918 ) ) ;
#18260 = CARTESIAN_POINT ( 'NONE',  ( 122.2128881442453263, -7.643976991954077427, -18.09477374809248928 ) ) ;
#18259 = CARTESIAN_POINT ( 'NONE',  ( 123.9146881442452894, 0.9020085738987339008, -11.91225656197089222 ) ) ;
#18261 = CARTESIAN_POINT ( 'NONE',  ( 120.3685329359119862, -5.367793381288652910, -18.78638297431638904 ) ) ;
#18262 = CARTESIAN_POINT ( 'NONE',  ( 123.6877814775786533, -6.222761293078241884, -8.102969835052219238 ) ) ;
#18263 = CARTESIAN_POINT ( 'NONE',  ( 112.5126281442453120, 0.1319031606808879209, -14.10382304977623669 ) ) ;
#18264 = CARTESIAN_POINT ( 'NONE',  ( 118.4689281442453392, 0.9020085738987339008, -11.91225656197089222 ) ) ;
#18265 = ORIENTED_EDGE ( 'NONE', *, *, #9032, .F. ) ;
#18266 = ORIENTED_EDGE ( 'NONE', *, *, #26730, .F. ) ;
#18267 = DIRECTION ( 'NONE',  ( 1.000000000000000000, 0.000000000000000000, -0.000000000000000000 ) ) ;
#18268 = CARTESIAN_POINT ( 'NONE',  ( 115.2053796295247849, -4.863998795839590272, -19.15521520033831493 ) ) ;
#18269 = CARTESIAN_POINT ( 'NONE',  ( 113.6774108795247997, -1.325403438956436419, -16.93181055722141792 ) ) ;
#18270 = CARTESIAN_POINT ( 'NONE',  ( 111.6632702545248605, 0.1403307496149616695, -11.32035403202665336 ) ) ;
#18271 = CARTESIAN_POINT ( 'NONE',  ( 125.4463081442452932, -5.638512984488999180, -18.83840828888717311 ) ) ;
#18272 = CARTESIAN_POINT ( 'NONE',  ( 116.5402214775786405, 0.2603800115204892296, -16.42320221600525088 ) ) ;
#18273 = ORIENTED_EDGE ( 'NONE', *, *, #8860, .F. ) ;
#18274 = CARTESIAN_POINT ( 'NONE',  ( 113.1366214775786432, -7.643976991954077427, -18.09477374809248928 ) ) ;
#18275 = CARTESIAN_POINT ( 'NONE',  ( 105.7597546295248350, -4.863998795839590272, -7.631215200338315796 ) ) ;
#18276 = DIRECTION ( 'NONE',  ( 0.9609149988134837450, -0.1028163501681639419, 0.2570431154366518145 ) ) ;
#18277 = DIRECTION ( 'NONE',  ( 0.9609149988134837450, -0.1028163501681639419, 0.2570431154366518145 ) ) ;
#18278 = CARTESIAN_POINT ( 'NONE',  ( 109.2294520814496650, -0.4000957807073393102, -15.81271325186753351 ) ) ;
#18279 = CARTESIAN_POINT ( 'NONE',  ( 79.38366267499158369, 5.039764807350117337, -6.277090637128386774 ) ) ;
#18280 = CARTESIAN_POINT ( 'NONE',  ( 115.6893214775786447, 0.5811942927096154232, -14.16772938898807155 ) ) ;
#18281 = CARTESIAN_POINT ( 'NONE',  ( 112.7050671295247923, -10.62599879583958540, -13.39321520033831447 ) ) ;
#18282 = CARTESIAN_POINT ( 'NONE',  ( 109.5796765045248122, -2.791137627527939813, -8.388885654883777576 ) ) ;
#18283 = ORIENTED_EDGE ( 'NONE', *, *, #18686, .F. ) ;
#18284 = CARTESIAN_POINT ( 'NONE',  ( 121.9470836909669913, -25.99489077589524300, -13.39321520033831447 ) ) ;
#18285 = CARTESIAN_POINT ( 'NONE',  ( 117.8449348109119938, -1.833838273342659253, -17.42832698103878286 ) ) ;
#18286 = CARTESIAN_POINT ( 'NONE',  ( 115.4056881442453459, -7.893985811506177619, -18.51759400769804742 ) ) ;
#18287 = CARTESIAN_POINT ( 'NONE',  ( 112.3991748109119868, -8.166667518702817929, -8.995218007635859436 ) ) ;
#18288 = VECTOR ( 'NONE', #14922, 1000.000000000000114 ) ;
#18289 = CARTESIAN_POINT ( 'NONE',  ( 125.6164881442453094, -9.565557343593413364, -10.61323700422348004 ) ) ;
#18290 = CARTESIAN_POINT ( 'NONE',  ( 121.5321681442453183, -0.1624402480850797581, -16.17319339645315424 ) ) ;
#18291 = CARTESIAN_POINT ( 'NONE',  ( 117.3343948109119737, -6.222761293078241884, -8.102969835052219238 ) ) ;
#18292 = ORIENTED_EDGE ( 'NONE', *, *, #8110, .T. ) ;
#18293 = CARTESIAN_POINT ( 'NONE',  ( 123.4244704359119709, -10.25716656981731489, -12.88942061488890545 ) ) ;
#18294 = DIRECTION ( 'NONE',  ( 0.000000000000000000, 0.000000000000000000, -1.000000000000000000 ) ) ;
#18295 = CARTESIAN_POINT ( 'NONE',  ( 119.0929214775786278, -4.153390946401325223, -8.397313243818185668 ) ) ;
#18296 = ORIENTED_EDGE ( 'NONE', *, *, #43714, .T. ) ;
#18297 = DIRECTION ( 'NONE',  ( 0.000000000000000000, 0.000000000000000000, 1.000000000000000000 ) ) ;
#18298 = CARTESIAN_POINT ( 'NONE',  ( 113.8173414775786512, 0.2603800115204892296, -16.42320221600525088 ) ) ;
#18299 = CARTESIAN_POINT ( 'NONE',  ( 106.7320983795247855, -8.402594152722688392, -16.93181055722141792 ) ) ;
#18300 = CARTESIAN_POINT ( 'NONE',  ( 113.8740681442453138, -9.859900752359374465, -12.68260735090039404 ) ) ;
#18301 = ORIENTED_EDGE ( 'NONE', *, *, #13860, .F. ) ;
#18302 = VERTEX_POINT ( 'NONE', #8676 ) ;
#18303 = CIRCLE ( 'NONE', #23423, 2.999999999999999556 ) ;
#18304 = CARTESIAN_POINT ( 'NONE',  ( 119.6034614775786196, -3.505236298600246325, -18.68346056562440793 ) ) ;
#18305 = CARTESIAN_POINT ( 'NONE',  ( 119.2063748109119814, -7.894159318335828068, -9.358103419637847864 ) ) ;
#18306 =( BOUNDED_SURFACE ( )  B_SPLINE_SURFACE ( 1, 2, ( 
 ( #13669, #44686, #10248, #17523, #9801, #34390, #37602, #186, #3395, #14104, #41927, #30533, #23711, #27577, #44455, #27120, #37368, #20283, #2941, #24156, #20060, #16871, #20511, #38047, #33942, #3172, #2713, #30761, #13221, #23936, #37818, #6594, #42374, #4507, #3823, #15222, #38704, #22068, #28467, #11135, #18194, #412, #25493, #636, #8162, #35733, #4048, #39397, #4276, #25268, #29129, #28913, #18429, #35959, #18648, #14329, #10691, #10911, #28692, #32321, #42151, #4730, #14549, #1086, #15000, #38476, #24594, #32540, #7252, #35043, #21389, #21839, #21167, #42596, #17970, #17747, #24812, #1310, #31871, #31643, #28243, #7471, #35504, #42823, #11584, #32088, #35271, #25038, #859, #39165, #38930, #7701, #21615, #14777, #11358, #7929, #8829, #22509, #40064, #33205, #5404, #39846, #25938, #22291, #4951, #12265, #8385, #12488, #8610, #36185, #32976, #5173, #1752, #19320, #15451, #18864, #22730, #26159, #1529, #15676, #36630, #29355, #1980, #15906, #32756, #36403, #19091, #29580, #43270, #43719, #43496, #12036, #25716, #29805, #43041, #11809, #39623, #32500, #1274, #11770, #26122, #40259, #43230, #29318, #36143, #36594, #33166, #15186, #8791, #43459, #29543, #43909, #5369, #26351, #32719, #16087, #15413, #22923, #25456, #29090, #19054, #1941, #43675, #39359, #1716, #22473, #8126, #12224, #29764, #15867, #11997, #12450, #9025, #36816, #29992, #33386, #5584, #19508, #39804, #15639, #22028, #25678, #8572, #36367, #40027, #43001, #39584, #8346, #25900, #19287, #2159, #35921, #4688, #22698, #18608, #22248, #4912, #5138, #32940, #18827, #1491, #2391, #34081, #41175, #40490, #34305, #6277, #30673, #20197, #34521, #17223, #9473, #19960, #19729, #37503, #2848, #9935, #37735, #30446, #27261, #23384, #13128, #16780, #16319, #5810, #3299, #37040, #3078, #9250, #30222, #44593, #13356, #23848, #6506, #23159, #20421, #17006, #30895, #44817, #13575, #44142, #27485, #40947, #41404, #27032, #10160, #37269, #24068, #37959, #6735, #6038, #12678, #20645, #31113, #26576, #33614, #12907 ),
 ( #26804, #40714, #33849, #2618, #16550, #44366, #9704, #23617, #14018, #324, #24505, #32000, #10821, #21525, #28154, #7611, #28599, #14685, #14237, #17660, #20859, #17438, #42282, #38176, #18332, #42063, #34737, #21300, #38607, #35183, #763, #38389, #3520, #35412, #11044, #41843, #3960, #4187, #27933, #42510, #11270, #31331, #24718, #7383, #17882, #7162, #21074, #31779, #25178, #105, #551, #10603, #39076, #28369, #7845, #21751, #6954, #34951, #14462, #3737, #31556, #35644, #24946, #38842, #18107, #4418, #45038, #13798, #27710, #41624, #10380, #24290, #18557, #22870, #5316, #43401, #5534, #18782, #26071, #25404, #36763, #15137, #43624, #4864, #32672, #39751, #21975, #1883, #22197, #29711, #12169, #25631, #15810, #25843, #1662, #32225, #19232, #39975, #12398, #40205, #35862, #998, #32449, #5085, #8738, #1223, #26298, #36093, #22646, #36542, #14913, #28824, #8971, #42734, #11499, #42952, #33115, #39303, #19001, #39534, #8074, #4636, #29043, #11718, #8295, #22423, #29488, #1440, #29267, #32888, #8520, #43181, #15362, #11947, #36315, #15586, #30622, #37904, #5985, #13299, #12629, #24016, #2338, #30844, #37213, #19910, #26974, #9197, #34254, #9415, #16950, #44537, #12853, #3029, #13076, #34030, #19451, #37685, #27207, #44767, #27434, #23106, #33334, #19673, #37450, #41125, #5753, #13526, #23327, #9884, #23795, #2108, #16036, #41356, #29944, #43857, #30171, #6458, #26527, #6222, #26754, #40436, #33561, #10113, #40663, #36984, #16267, #2799, #20367, #44088, #33795, #40894, #2567, #16496, #44318, #16725, #30396, #9647, #23569, #20146, #38788, #17610, #28318, #34899, #14408, #35357, #21474, #7116, #24448, #27658, #24234, #3910, #44990, #25126, #21026, #41571, #28102, #273, #42008, #7560, #31279, #10331, #42230, #17828, #3475, #10772, #10994, #34687, #4133, #18055, #38127, #3688, #31502, #14183, #13966, #27877, #24668, #31946, #6898, #38555, #20808, #711, #35128, #14632, #28550, #13749, #17391, #7331, #24895, #53, #31724, #21250, #496, #6682, #42454, #11220, #41791 ) ),
 .UNSPECIFIED., .F., .F., .T. ) 
 B_SPLINE_SURFACE_WITH_KNOTS ( ( 2, 2 ),
 ( 3, 2, 2, 2, 2, 2, 2, 2, 2, 2, 2, 2, 2, 2, 2, 2, 2, 2, 2, 2, 2, 2, 2, 2, 2, 2, 2, 2, 2, 2, 2, 2, 2, 2, 2, 2, 2, 2, 2, 2, 2, 2, 2, 2, 2, 2, 2, 2, 2, 2, 2, 2, 2, 2, 2, 2, 2, 2, 2, 2, 2, 2, 2, 2, 2, 2, 2, 2, 2, 2, 2, 2, 2, 2, 2, 2, 2, 2, 2, 2, 2, 2, 2, 2, 2, 2, 2, 2, 2, 2, 2, 2, 2, 2, 2, 2, 2, 2, 2, 2, 2, 2, 2, 2, 2, 2, 2, 2, 2, 2, 2, 2, 2, 2, 2, 2, 2, 2, 2, 2, 2, 2, 2, 2, 2, 2, 2, 2, 3 ),
 ( 0.000000000000000000, 1.000000000000000000 ),
 ( 0.000000000000000000, 0.007812500000000000000, 0.01562500000000000000, 0.02343750000000000000, 0.03125000000000000000, 0.03906250000000000000, 0.04687500000000000000, 0.05468750000000000000, 0.06250000000000000000, 0.07031250000000000000, 0.07812500000000000000, 0.08593750000000000000, 0.09375000000000000000, 0.1015625000000000000, 0.1093750000000000000, 0.1171875000000000000, 0.1250000000000000000, 0.1328125000000000000, 0.1406250000000000000, 0.1484375000000000000, 0.1562500000000000000, 0.1640625000000000000, 0.1718750000000000000, 0.1796875000000000000, 0.1875000000000000000, 0.1953125000000000000, 0.2031250000000000000, 0.2109375000000000000, 0.2187500000000000000, 0.2265625000000000000, 0.2343750000000000000, 0.2421875000000000000, 0.2500000000000000000, 0.2578125000000000000, 0.2656250000000000000, 0.2734375000000000000, 0.2812500000000000000, 0.2890625000000000000, 0.2968750000000000000, 0.3046875000000000000, 0.3125000000000000000, 0.3203125000000000000, 0.3281250000000000000, 0.3359375000000000000, 0.3437500000000000000, 0.3515625000000000000, 0.3593750000000000000, 0.3671875000000000000, 0.3750000000000000000, 0.3828125000000000000, 0.3906250000000000000, 0.3984375000000000000, 0.4062500000000000000, 0.4140625000000000000, 0.4218750000000000000, 0.4296875000000000000, 0.4375000000000000000, 0.4453125000000000000, 0.4531250000000000000, 0.4609375000000000000, 0.4687500000000000000, 0.4765625000000000000, 0.4843750000000000000, 0.4921875000000000000, 0.5000000000000000000, 0.5078125000000000000, 0.5156250000000000000, 0.5234375000000000000, 0.5312500000000000000, 0.5390625000000000000, 0.5468750000000000000, 0.5546875000000000000, 0.5625000000000000000, 0.5703125000000000000, 0.5781250000000000000, 0.5859375000000000000, 0.5937500000000000000, 0.6015625000000000000, 0.6093750000000000000, 0.6171875000000000000, 0.6250000000000000000, 0.6328125000000000000, 0.6406250000000000000, 0.6484375000000000000, 0.6562500000000000000, 0.6640625000000000000, 0.6718750000000000000, 0.6796875000000000000, 0.6875000000000000000, 0.6953125000000000000, 0.7031250000000000000, 0.7109375000000000000, 0.7187500000000000000, 0.7265625000000000000, 0.7343750000000000000, 0.7421875000000000000, 0.7500000000000000000, 0.7578125000000000000, 0.7656250000000000000, 0.7734375000000000000, 0.7812500000000000000, 0.7890625000000000000, 0.7968750000000000000, 0.8046875000000000000, 0.8125000000000000000, 0.8203125000000000000, 0.8281250000000000000, 0.8359375000000000000, 0.8437500000000000000, 0.8515625000000000000, 0.8593750000000000000, 0.8671875000000000000, 0.8750000000000000000, 0.8828125000000000000, 0.8906250000000000000, 0.8984375000000000000, 0.9062500000000000000, 0.9140625000000000000, 0.9218750000000000000, 0.9296875000000000000, 0.9375000000000000000, 0.9453125000000000000, 0.9531250000000000000, 0.9609375000000000000, 0.9687500000000000000, 0.9765625000000000000, 0.9843750000000000000, 0.9921875000000000000, 1.000000000000000000 ),
 .UNSPECIFIED. ) 
 GEOMETRIC_REPRESENTATION_ITEM ( )  RATIONAL_B_SPLINE_SURFACE ( (
 ( 1.000000000000000000, 0.9238795325112869605, 1.000000000000000000, 0.9238795325112869605, 1.000000000000000000, 0.9238795325112869605, 1.000000000000000000, 0.9238795325112869605, 1.000000000000000000, 0.9238795325112869605, 1.000000000000000000, 0.9238795325112869605, 1.000000000000000000, 0.9238795325112869605, 1.000000000000000000, 0.9238795325112869605, 1.000000000000000000, 0.9238795325112869605, 1.000000000000000000, 0.9238795325112869605, 1.000000000000000000, 0.9238795325112869605, 1.000000000000000000, 0.9238795325112869605, 1.000000000000000000, 0.9238795325112869605, 1.000000000000000000, 0.9238795325112869605, 1.000000000000000000, 0.9238795325112869605, 1.000000000000000000, 0.9238795325112869605, 1.000000000000000000, 0.9238795325112869605, 1.000000000000000000, 0.9238795325112869605, 1.000000000000000000, 0.9238795325112869605, 1.000000000000000000, 0.9238795325112869605, 1.000000000000000000, 0.9238795325112869605, 1.000000000000000000, 0.9238795325112869605, 1.000000000000000000, 0.9238795325112869605, 1.000000000000000000, 0.9238795325112869605, 1.000000000000000000, 0.9238795325112869605, 1.000000000000000000, 0.9238795325112869605, 1.000000000000000000, 0.9238795325112869605, 1.000000000000000000, 0.9238795325112869605, 1.000000000000000000, 0.9238795325112869605, 1.000000000000000000, 0.9238795325112869605, 1.000000000000000000, 0.9238795325112869605, 1.000000000000000000, 0.9238795325112869605, 1.000000000000000000, 0.9238795325112869605, 1.000000000000000000, 0.9238795325112869605, 1.000000000000000000, 0.9238795325112869605, 1.000000000000000000, 0.9238795325112869605, 1.000000000000000000, 0.9238795325112869605, 1.000000000000000000, 0.9238795325112869605, 1.000000000000000000, 0.9238795325112869605, 1.000000000000000000, 0.9238795325112869605, 1.000000000000000000, 0.9238795325112869605, 1.000000000000000000, 0.9238795325112869605, 1.000000000000000000, 0.9238795325112869605, 1.000000000000000000, 0.9238795325112869605, 1.000000000000000000, 0.9238795325112869605, 1.000000000000000000, 0.9238795325112869605, 1.000000000000000000, 0.9238795325112869605, 1.000000000000000000, 0.9238795325112869605, 1.000000000000000000, 0.9238795325112869605, 1.000000000000000000, 0.9238795325112869605, 1.000000000000000000, 0.9238795325112869605, 1.000000000000000000, 0.9238795325112869605, 1.000000000000000000, 0.9238795325112869605, 1.000000000000000000, 0.9238795325112869605, 1.000000000000000000, 0.9238795325112869605, 1.000000000000000000, 0.9238795325112869605, 1.000000000000000000, 0.9238795325112869605, 1.000000000000000000, 0.9238795325112869605, 1.000000000000000000, 0.9238795325112869605, 1.000000000000000000, 0.9238795325112869605, 1.000000000000000000, 0.9238795325112869605, 1.000000000000000000, 0.9238795325112869605, 1.000000000000000000, 0.9238795325112869605, 1.000000000000000000, 0.9238795325112869605, 1.000000000000000000, 0.9238795325112869605, 1.000000000000000000, 0.9238795325112869605, 1.000000000000000000, 0.9238795325112869605, 1.000000000000000000, 0.9238795325112869605, 1.000000000000000000, 0.9238795325112869605, 1.000000000000000000, 0.9238795325112869605, 1.000000000000000000, 0.9238795325112869605, 1.000000000000000000, 0.9238795325112869605, 1.000000000000000000, 0.9238795325112869605, 1.000000000000000000, 0.9238795325112869605, 1.000000000000000000, 0.9238795325112869605, 1.000000000000000000, 0.9238795325112869605, 1.000000000000000000, 0.9238795325112869605, 1.000000000000000000, 0.9238795325112869605, 1.000000000000000000, 0.9238795325112869605, 1.000000000000000000, 0.9238795325112869605, 1.000000000000000000, 0.9238795325112869605, 1.000000000000000000, 0.9238795325112869605, 1.000000000000000000, 0.9238795325112869605, 1.000000000000000000, 0.9238795325112869605, 1.000000000000000000, 0.9238795325112869605, 1.000000000000000000, 0.9238795325112869605, 1.000000000000000000, 0.9238795325112869605, 1.000000000000000000, 0.9238795325112869605, 1.000000000000000000, 0.9238795325112869605, 1.000000000000000000, 0.9238795325112869605, 1.000000000000000000, 0.9238795325112869605, 1.000000000000000000, 0.9238795325112869605, 1.000000000000000000, 0.9238795325112869605, 1.000000000000000000, 0.9238795325112869605, 1.000000000000000000, 0.9238795325112869605, 1.000000000000000000, 0.9238795325112869605, 1.000000000000000000, 0.9238795325112869605, 1.000000000000000000, 0.9238795325112869605, 1.000000000000000000, 0.9238795325112869605, 1.000000000000000000, 0.9238795325112869605, 1.000000000000000000, 0.9238795325112869605, 1.000000000000000000, 0.9238795325112869605, 1.000000000000000000, 0.9238795325112869605, 1.000000000000000000, 0.9238795325112869605, 1.000000000000000000, 0.9238795325112869605, 1.000000000000000000, 0.9238795325112869605, 1.000000000000000000, 0.9238795325112869605, 1.000000000000000000, 0.9238795325112869605, 1.000000000000000000, 0.9238795325112869605, 1.000000000000000000, 0.9238795325112869605, 1.000000000000000000, 0.9238795325112869605, 1.000000000000000000, 0.9238795325112869605, 1.000000000000000000, 0.9238795325112869605, 1.000000000000000000, 0.9238795325112869605, 1.000000000000000000, 0.9238795325112869605, 1.000000000000000000, 0.9238795325112869605, 1.000000000000000000, 0.9238795325112869605, 1.000000000000000000, 0.9238795325112869605, 1.000000000000000000, 0.9238795325112869605, 1.000000000000000000, 0.9238795325112869605, 1.000000000000000000, 0.9238795325112869605, 1.000000000000000000, 0.9238795325112869605, 1.000000000000000000, 0.9238795325112869605, 1.000000000000000000, 0.9238795325112869605, 1.000000000000000000, 0.9238795325112869605, 1.000000000000000000, 0.9238795325112869605, 1.000000000000000000, 0.9238795325112869605, 1.000000000000000000, 0.9238795325112869605, 1.000000000000000000),
 ( 1.000000000000000000, 0.9238795325112869605, 1.000000000000000000, 0.9238795325112869605, 1.000000000000000000, 0.9238795325112869605, 1.000000000000000000, 0.9238795325112869605, 1.000000000000000000, 0.9238795325112869605, 1.000000000000000000, 0.9238795325112869605, 1.000000000000000000, 0.9238795325112869605, 1.000000000000000000, 0.9238795325112869605, 1.000000000000000000, 0.9238795325112869605, 1.000000000000000000, 0.9238795325112869605, 1.000000000000000000, 0.9238795325112869605, 1.000000000000000000, 0.9238795325112869605, 1.000000000000000000, 0.9238795325112869605, 1.000000000000000000, 0.9238795325112869605, 1.000000000000000000, 0.9238795325112869605, 1.000000000000000000, 0.9238795325112869605, 1.000000000000000000, 0.9238795325112869605, 1.000000000000000000, 0.9238795325112869605, 1.000000000000000000, 0.9238795325112869605, 1.000000000000000000, 0.9238795325112869605, 1.000000000000000000, 0.9238795325112869605, 1.000000000000000000, 0.9238795325112869605, 1.000000000000000000, 0.9238795325112869605, 1.000000000000000000, 0.9238795325112869605, 1.000000000000000000, 0.9238795325112869605, 1.000000000000000000, 0.9238795325112869605, 1.000000000000000000, 0.9238795325112869605, 1.000000000000000000, 0.9238795325112869605, 1.000000000000000000, 0.9238795325112869605, 1.000000000000000000, 0.9238795325112869605, 1.000000000000000000, 0.9238795325112869605, 1.000000000000000000, 0.9238795325112869605, 1.000000000000000000, 0.9238795325112869605, 1.000000000000000000, 0.9238795325112869605, 1.000000000000000000, 0.9238795325112869605, 1.000000000000000000, 0.9238795325112869605, 1.000000000000000000, 0.9238795325112869605, 1.000000000000000000, 0.9238795325112869605, 1.000000000000000000, 0.9238795325112869605, 1.000000000000000000, 0.9238795325112869605, 1.000000000000000000, 0.9238795325112869605, 1.000000000000000000, 0.9238795325112869605, 1.000000000000000000, 0.9238795325112869605, 1.000000000000000000, 0.9238795325112869605, 1.000000000000000000, 0.9238795325112869605, 1.000000000000000000, 0.9238795325112869605, 1.000000000000000000, 0.9238795325112869605, 1.000000000000000000, 0.9238795325112869605, 1.000000000000000000, 0.9238795325112869605, 1.000000000000000000, 0.9238795325112869605, 1.000000000000000000, 0.9238795325112869605, 1.000000000000000000, 0.9238795325112869605, 1.000000000000000000, 0.9238795325112869605, 1.000000000000000000, 0.9238795325112869605, 1.000000000000000000, 0.9238795325112869605, 1.000000000000000000, 0.9238795325112869605, 1.000000000000000000, 0.9238795325112869605, 1.000000000000000000, 0.9238795325112869605, 1.000000000000000000, 0.9238795325112869605, 1.000000000000000000, 0.9238795325112869605, 1.000000000000000000, 0.9238795325112869605, 1.000000000000000000, 0.9238795325112869605, 1.000000000000000000, 0.9238795325112869605, 1.000000000000000000, 0.9238795325112869605, 1.000000000000000000, 0.9238795325112869605, 1.000000000000000000, 0.9238795325112869605, 1.000000000000000000, 0.9238795325112869605, 1.000000000000000000, 0.9238795325112869605, 1.000000000000000000, 0.9238795325112869605, 1.000000000000000000, 0.9238795325112869605, 1.000000000000000000, 0.9238795325112869605, 1.000000000000000000, 0.9238795325112869605, 1.000000000000000000, 0.9238795325112869605, 1.000000000000000000, 0.9238795325112869605, 1.000000000000000000, 0.9238795325112869605, 1.000000000000000000, 0.9238795325112869605, 1.000000000000000000, 0.9238795325112869605, 1.000000000000000000, 0.9238795325112869605, 1.000000000000000000, 0.9238795325112869605, 1.000000000000000000, 0.9238795325112869605, 1.000000000000000000, 0.9238795325112869605, 1.000000000000000000, 0.9238795325112869605, 1.000000000000000000, 0.9238795325112869605, 1.000000000000000000, 0.9238795325112869605, 1.000000000000000000, 0.9238795325112869605, 1.000000000000000000, 0.9238795325112869605, 1.000000000000000000, 0.9238795325112869605, 1.000000000000000000, 0.9238795325112869605, 1.000000000000000000, 0.9238795325112869605, 1.000000000000000000, 0.9238795325112869605, 1.000000000000000000, 0.9238795325112869605, 1.000000000000000000, 0.9238795325112869605, 1.000000000000000000, 0.9238795325112869605, 1.000000000000000000, 0.9238795325112869605, 1.000000000000000000, 0.9238795325112869605, 1.000000000000000000, 0.9238795325112869605, 1.000000000000000000, 0.9238795325112869605, 1.000000000000000000, 0.9238795325112869605, 1.000000000000000000, 0.9238795325112869605, 1.000000000000000000, 0.9238795325112869605, 1.000000000000000000, 0.9238795325112869605, 1.000000000000000000, 0.9238795325112869605, 1.000000000000000000, 0.9238795325112869605, 1.000000000000000000, 0.9238795325112869605, 1.000000000000000000, 0.9238795325112869605, 1.000000000000000000, 0.9238795325112869605, 1.000000000000000000, 0.9238795325112869605, 1.000000000000000000, 0.9238795325112869605, 1.000000000000000000, 0.9238795325112869605, 1.000000000000000000, 0.9238795325112869605, 1.000000000000000000, 0.9238795325112869605, 1.000000000000000000, 0.9238795325112869605, 1.000000000000000000, 0.9238795325112869605, 1.000000000000000000, 0.9238795325112869605, 1.000000000000000000, 0.9238795325112869605, 1.000000000000000000, 0.9238795325112869605, 1.000000000000000000, 0.9238795325112869605, 1.000000000000000000, 0.9238795325112869605, 1.000000000000000000, 0.9238795325112869605, 1.000000000000000000, 0.9238795325112869605, 1.000000000000000000, 0.9238795325112869605, 1.000000000000000000, 0.9238795325112869605, 1.000000000000000000, 0.9238795325112869605, 1.000000000000000000, 0.9238795325112869605, 1.000000000000000000, 0.9238795325112869605, 1.000000000000000000, 0.9238795325112869605, 1.000000000000000000, 0.9238795325112869605, 1.000000000000000000, 0.9238795325112869605, 1.000000000000000000) ) ) 
 REPRESENTATION_ITEM ( '' )  SURFACE ( )  );
#18307 = FACE_OUTER_BOUND ( 'NONE', #40274, .T. ) ;
#18308 = EDGE_CURVE ( 'NONE', #43860, #17999, #5214, .T. ) ;
#18309 = CARTESIAN_POINT ( 'NONE',  ( 124.0495485609119584, -10.36940331770106916, -15.09355782777062061 ) ) ;
#18310 = ORIENTED_EDGE ( 'NONE', *, *, #31803, .T. ) ;
#18311 = LINE ( 'NONE', #21952, #9182 ) ;
#18312 = CARTESIAN_POINT ( 'NONE',  ( 119.7434548109119987, -2.601528322103975999, -8.933709204980601726 ) ) ;
#18313 = CARTESIAN_POINT ( 'NONE',  ( 109.9269421295247753, 0.8980012041604618078, -13.39321520033831447 ) ) ;
#18314 = AXIS2_PLACEMENT_3D ( 'NONE', #27655, #10329, #16265 ) ;
#18315 = CARTESIAN_POINT ( 'NONE',  ( 113.9307948109119906, 0.9020085738987339008, -11.91225656197089222 ) ) ;
#18316 = PRODUCT_DEFINITION_SHAPE ( 'NONE', 'NONE',  #15653 ) ;
#18317 = CARTESIAN_POINT ( 'NONE',  ( 126.3539348109119800, -4.153390946401325223, -8.397313243818185668 ) ) ;
#18318 = B_SPLINE_CURVE_WITH_KNOTS ( 'NONE', 3,
 ( #8224, #15740, #15510, #8669, #4341, #43104, #25335, #29417, #12100, #5014, #5241, #22353, #1148, #21901, #22130, #1813, #26004, #22572, #28979, #39460, #7993, #36023, #41831, #14844, #32381, #15065, #18932, #39908, #36474, #39228, #4567, #4791, #925, #35795, #10591, #32819, #19157, #18491, #33038, #24493, #18712, #42884, #39003 ),
 .UNSPECIFIED., .F., .F.,
 ( 4, 2, 2, 2, 1, 1, 1, 2, 2, 2, 2, 2, 2, 2, 2, 2, 2, 2, 2, 2, 2, 2, 4 ),
 ( 0.000000000000000000, 0.1250000000000104361, 0.1875000000000154321, 0.2187500000000180134, 0.2343750000000193456, 0.2421875000000199563, 0.2460937500000199285, 0.2480468750000195954, 0.2500000000000192624, 0.3750000000000177636, 0.4375000000000173195, 0.4687500000000175970, 0.4843750000000168754, 0.4921875000000162093, 0.4960937500000164313, 0.5000000000000166533, 0.6250000000000119904, 0.6875000000000097700, 0.7187500000000087708, 0.7343750000000083267, 0.7500000000000078826, 0.8750000000000039968, 1.000000000000000000 ),
 .UNSPECIFIED. ) ;
#18319 = CARTESIAN_POINT ( 'NONE',  ( 118.2987481442453088, -7.894159318335828068, -9.358103419637847864 ) ) ;
#18320 = LINE ( 'NONE', #42941, #24036 ) ;
#18321 = ORIENTED_EDGE ( 'NONE', *, *, #8072, .T. ) ;
#18322 = CARTESIAN_POINT ( 'NONE',  ( 121.0216281442452981, -7.894159318335828068, -9.358103419637847864 ) ) ;
#18323 = CARTESIAN_POINT ( 'NONE',  ( 116.0286950891469786, 2.331313199634366118, -12.14321520033831625 ) ) ;
#18324 = DIRECTION ( 'NONE',  ( 1.000000000000000000, 0.000000000000000000, -0.000000000000000000 ) ) ;
#18325 = CARTESIAN_POINT ( 'NONE',  ( 121.9470836909669913, -25.99489077589524300, -13.39321520033831447 ) ) ;
#18326 = CARTESIAN_POINT ( 'NONE',  ( 116.2565881442452991, -9.261995988541697145, -16.69588392320189030 ) ) ;
#18327 = EDGE_LOOP ( 'NONE', ( #40806, #39896, #3048, #15797, #22365 ) ) ;
#18328 = CARTESIAN_POINT ( 'NONE',  ( 118.9794681442453026, -9.261995988541697145, -16.69588392320189030 ) ) ;
#18329 = CARTESIAN_POINT ( 'NONE',  ( 113.9875214775786532, -0.4660016031367876232, -10.09054647747474220 ) ) ;
#18330 = CARTESIAN_POINT ( 'NONE',  ( 110.6214733795247867, -8.938348069036489818, -17.46756447353520159 ) ) ;
#18331 = CARTESIAN_POINT ( 'NONE',  ( 114.6682414775786469, -1.561330072975668060, -17.79121239304076596 ) ) ;
#18332 = CARTESIAN_POINT ( 'NONE',  ( 113.0798948109119948, -0.4660016031367893996, -10.09054647747474043 ) ) ;
#18333 = CARTESIAN_POINT ( 'NONE',  ( 60.53937939559665438, -4.256997083809236138, -19.39321520033831447 ) ) ;
#18334 = CYLINDRICAL_SURFACE ( 'NONE', #7477, 1.999999999999998890 ) ;
#18335 = CARTESIAN_POINT ( 'NONE',  ( 70.19189222814998175, -54.83461124330791847, -35.13666250696951465 ) ) ;
#18336 = ADVANCED_FACE ( 'NONE', ( #32609 ), #26482, .T. ) ;
#18337 = VERTEX_POINT ( 'NONE', #11879 ) ;
#18338 = DIRECTION ( 'NONE',  ( -0.7871354856660202071, 0.6167752151498580027, 0.002461946824133919541 ) ) ;
#18339 = CARTESIAN_POINT ( 'NONE',  ( 109.2295187470875817, -2.680572428980009914, -17.98422477323183344 ) ) ;
#18340 = VECTOR ( 'NONE', #11851, 1000.000000000000114 ) ;
#18341 = CARTESIAN_POINT ( 'NONE',  ( 121.0783548109119749, -9.565557343593413364, -10.61323700422348004 ) ) ;
#18342 = CARTESIAN_POINT ( 'NONE',  ( 65.16811225466804558, -13.42767900044409579, -11.91060832829492711 ) ) ;
#18343 = DIRECTION ( 'NONE',  ( 0.000000000000000000, -0.3818493186865927203, 0.9242245927363029745 ) ) ;
#18344 = CARTESIAN_POINT ( 'NONE',  ( 114.0941296295247867, -4.863998795839590272, -8.388885654883775800 ) ) ;
#18345 = CARTESIAN_POINT ( 'NONE',  ( 126.3063647503471998, -4.505965723778011522, -8.361964086144073605 ) ) ;
#18346 = CARTESIAN_POINT ( 'NONE',  ( 113.3635281442453504, -0.1624402480850797581, -16.17319339645315424 ) ) ;
#18347 = CARTESIAN_POINT ( 'NONE',  ( 88.88468749803642766, -10.91782331763674385, -14.14321520033831625 ) ) ;
#18348 = ADVANCED_FACE ( 'NONE', ( #41060 ), #44831, .T. ) ;
#18349 = CARTESIAN_POINT ( 'NONE',  ( 123.1772414775786189, -4.089484607189486809, -7.948022111789456723 ) ) ;
#18350 = CARTESIAN_POINT ( 'NONE',  ( 119.6601881442453106, -8.166667518702819706, -8.995218007635861213 ) ) ;
#18351 = ORIENTED_EDGE ( 'NONE', *, *, #34569, .F. ) ;
#18352 = EDGE_CURVE ( 'NONE', #31472, #2634, #41661, .T. ) ;
#18353 = CARTESIAN_POINT ( 'NONE',  ( 118.5256548109119876, -8.899110576539710493, -16.42337572283490132 ) ) ;
#18354 = CIRCLE ( 'NONE', #43838, 6.500000000000005329 ) ;
#18355 = DIRECTION ( 'NONE',  ( 0.000000000000000000, 0.000000000000000000, -1.000000000000000000 ) ) ;
#18356 = CARTESIAN_POINT ( 'NONE',  ( 116.0864081442453113, -9.988377603198976828, -10.36322818467138340 ) ) ;
#18357 = CARTESIAN_POINT ( 'NONE',  ( 118.5823814775786360, -7.643976991954077427, -18.09477374809248928 ) ) ;
#18358 = ORIENTED_EDGE ( 'NONE', *, *, #43166, .F. ) ;
#18359 = CARTESIAN_POINT ( 'NONE',  ( 124.3117748109119844, 0.1319031606808879209, -14.10382304977623669 ) ) ;
#18360 = ADVANCED_FACE ( 'NONE', ( #39535 ), #14463, .T. ) ;
#18361 = CARTESIAN_POINT ( 'NONE',  ( 121.8725281442453223, -3.383040157471821630, -19.15922257007629170 ) ) ;
#18362 = CARTESIAN_POINT ( 'NONE',  ( 137.5049267796298125, 0.06692046795779585389, -14.26109179921826531 ) ) ;
#18363 = CARTESIAN_POINT ( 'NONE',  ( 108.6767858795247861, -0.7896495226426338832, -17.46756447353520159 ) ) ;
#18364 = ADVANCED_FACE ( 'NONE', ( #42511 ), #232, .T. ) ;
#18365 = EDGE_CURVE ( 'NONE', #17168, #9021, #11271, .T. ) ;
#18366 = EDGE_CURVE ( 'NONE', #24723, #2572, #24948, .T. ) ;
#18367 = DIRECTION ( 'NONE',  ( -0.9659258262890688673, -0.2588190451025190186, 0.000000000000000000 ) ) ;
#18368 = CARTESIAN_POINT ( 'NONE',  ( 126.2896895366256729, 0.1563366305949911439, -13.78536022922076754 ) ) ;
#18369 = CARTESIAN_POINT ( 'NONE',  ( 113.6774108795247997, -1.325403438956436419, -16.93181055722141792 ) ) ;
#18370 = AXIS2_PLACEMENT_3D ( 'NONE', #36532, #29701, #12388 ) ;
#18371 = CARTESIAN_POINT ( 'NONE',  ( 117.0507614775786465, -10.30919188438810075, -12.61870101168855918 ) ) ;
#18372 = APPLICATION_CONTEXT ( 'automotive_design' ) ;
#18373 = LINE ( 'NONE', #25439, #1833 ) ;
#18374 = CARTESIAN_POINT ( 'NONE',  ( 117.1074881442453233, 0.4262465694468514643, -12.03445270309931736 ) ) ;
#18375 = CARTESIAN_POINT ( 'NONE',  ( 126.2184548109108420, -0.8485035689962256988, -10.41384787932543610 ) ) ;
#18376 = CARTESIAN_POINT ( 'NONE',  ( 117.0507614775786465, 0.1319031606808827028, -14.10382304977625445 ) ) ;
#18377 = CARTESIAN_POINT ( 'NONE',  ( 109.2324108795247923, -1.325403438956436419, -16.93181055722141792 ) ) ;
#18378 = CARTESIAN_POINT ( 'NONE',  ( 112.3991748109119868, -1.833838273342658809, -17.42832698103878286 ) ) ;
#18379 = CARTESIAN_POINT ( 'NONE',  ( 123.2855641859119800, -8.321307733199551748, -9.223433127585318303 ) ) ;
#18380 = AXIS2_PLACEMENT_3D ( 'NONE', #30084, #9107, #2707 ) ;
#18381 = DIRECTION ( 'NONE',  ( 0.9705985873829334754, 0.08939452397200674250, -0.2234882575306194330 ) ) ;
#18383 = CARTESIAN_POINT ( 'NONE',  ( 117.9583881442453048, -10.30919188438810075, -12.61870101168855918 ) ) ;
#18382 = CARTESIAN_POINT ( 'NONE',  ( 64.51296881898170454, -15.37845651475741349, -10.94392415253807727 ) ) ;
#18384 = CARTESIAN_POINT ( 'NONE',  ( 119.0929214775786278, -4.153390946401325223, -8.397313243818185668 ) ) ;
#18385 = CARTESIAN_POINT ( 'NONE',  ( 125.2761281442453054, -10.63000616557722466, -14.87417383870573495 ) ) ;
#18386 = ORIENTED_EDGE ( 'NONE', *, *, #22951, .T. ) ;
#18387 = CARTESIAN_POINT ( 'NONE',  ( 137.2352176311238452, -8.690612541390031254, -9.760135143526762036 ) ) ;
#18388 = CARTESIAN_POINT ( 'NONE',  ( 122.1561614775786353, -0.4660016031367893996, -10.09054647747474043 ) ) ;
#18389 = CARTESIAN_POINT ( 'NONE',  ( 113.2606921295247702, -9.868328341294093420, -13.39321520033831447 ) ) ;
#18390 = CARTESIAN_POINT ( 'NONE',  ( 119.4332814775786318, -8.899110576539710493, -16.42337572283490132 ) ) ;
#18391 = CARTESIAN_POINT ( 'NONE',  ( 117.3343948109119737, -6.222761293078241884, -8.102969835052219238 ) ) ;
#18392 = CARTESIAN_POINT ( 'NONE',  ( 84.86020291624612355, -29.99489077589590025, -11.89662724278569073 ) ) ;
#18393 = CARTESIAN_POINT ( 'NONE',  ( 108.1906140045248463, -10.62599879583958717, -11.00651665394454604 ) ) ;
#18394 = CARTESIAN_POINT ( 'NONE',  ( 122.3830681442452857, -1.833838273342659697, -17.42832698103878286 ) ) ;
#18395 = CARTESIAN_POINT ( 'NONE',  ( 125.7866681442452688, -8.899110576539710493, -16.42337572283490132 ) ) ;
#18396 = DIRECTION ( 'NONE',  ( 1.000000000000000000, 0.000000000000000000, -0.000000000000000000 ) ) ;
#18397 = CARTESIAN_POINT ( 'NONE',  ( 109.2294535371698174, -0.3920599432768472337, -10.47762860381350336 ) ) ;
#18398 = CARTESIAN_POINT ( 'NONE',  ( 122.1048610609119720, -6.340755971794695078, -8.611740276972781771 ) ) ;
#18399 = CARTESIAN_POINT ( 'NONE',  ( 115.8999108795247821, -8.938348069036489818, -9.318865927141430916 ) ) ;
#18400 =( BOUNDED_CURVE ( )  B_SPLINE_CURVE ( 2, ( #6172, #20538, #34639, #37634, #6407 ),
 .UNSPECIFIED., .F., .F. ) 
 B_SPLINE_CURVE_WITH_KNOTS ( ( 3, 2, 3 ),
 ( 0.000000000000000000, 0.007812500000000000000, 0.01424533251905851956 ),
 .UNSPECIFIED. ) 
 CURVE ( )  GEOMETRIC_REPRESENTATION_ITEM ( )  RATIONAL_B_SPLINE_CURVE ( ( 1.000000000000000000, 0.9238795325112869605, 1.000000000000000000, 0.9373222120157009840, 0.9778625265000240319 ) ) 
 REPRESENTATION_ITEM ( '' )  );
#18401 = CARTESIAN_POINT ( 'NONE',  ( 86.04230958663552542, -25.82262605124138943, -7.893215200338315363 ) ) ;
#18402 = CARTESIAN_POINT ( 'NONE',  ( 82.50011035870637954, -31.66751168766318614, -23.35869902906633655 ) ) ;
#18403 = CARTESIAN_POINT ( 'NONE',  ( 117.5045748109119756, 0.5811942927096110934, -14.16772938898807510 ) ) ;
#18404 = CARTESIAN_POINT ( 'NONE',  ( 119.9438214775786378, -7.893985811506177619, -18.51759400769804742 ) ) ;
#18405 = CARTESIAN_POINT ( 'NONE',  ( 110.8298327545248299, -2.477300249445798297, -19.15521520033831138 ) ) ;
#18406 = CARTESIAN_POINT ( 'NONE',  ( 113.0231681442453322, 0.9020085738987339008, -11.91225656197089222 ) ) ;
#18407 = ORIENTED_EDGE ( 'NONE', *, *, #14712, .F. ) ;
#18408 = CARTESIAN_POINT ( 'NONE',  ( 117.2146229525735635, -1.111561923218657322, -17.14115599315433158 ) ) ;
#18409 = AXIS2_PLACEMENT_3D ( 'NONE', #20098, #226, #33983 ) ;
#18410 = CARTESIAN_POINT ( 'NONE',  ( 117.3911214775786505, -1.561330072975668504, -17.79121239304076951 ) ) ;
#18411 = CARTESIAN_POINT ( 'NONE',  ( 120.3976348109119812, -7.643976991954077427, -18.09477374809248928 ) ) ;
#18412 = DIRECTION ( 'NONE',  ( 0.000000000000000000, 0.000000000000000000, 1.000000000000000000 ) ) ;
#18413 = CARTESIAN_POINT ( 'NONE',  ( 125.1059481442452750, -8.166667518702819706, -8.995218007635861213 ) ) ;
#18414 = CARTESIAN_POINT ( 'NONE',  ( 122.2696148109119889, -4.089484607189486809, -7.948022111789456723 ) ) ;
#18415 = CARTESIAN_POINT ( 'NONE',  ( 111.5938171295247940, -10.62599879583958540, -13.39321520033831447 ) ) ;
#18416 = VECTOR ( 'NONE', #32030, 1000.000000000000227 ) ;
#18417 = B_SPLINE_CURVE_WITH_KNOTS ( 'NONE', 3,
 ( #35584, #10546, #35125, #38337 ),
 .UNSPECIFIED., .F., .F.,
 ( 4, 4 ),
 ( 0.000000000000000000, 1.000000000000000000 ),
 .UNSPECIFIED. ) ;
#18418 = CARTESIAN_POINT ( 'NONE',  ( 118.0151148109119816, 0.4262465694468514643, -12.03445270309931736 ) ) ;
#18419 = CARTESIAN_POINT ( 'NONE',  ( 120.2990798109119766, -2.173413727453600508, -8.297982527556802879 ) ) ;
#18420 = CARTESIAN_POINT ( 'NONE',  ( 83.72016463086879412, -25.99489077589524300, -13.39321520033831447 ) ) ;
#18421 = VERTEX_POINT ( 'NONE', #4419 ) ;
#18422 = EDGE_CURVE ( 'NONE', #35546, #7942, #38086, .T. ) ;
#18423 = CARTESIAN_POINT ( 'NONE',  ( 120.5768923109119868, -0.4387604401700512802, -15.73000352943951619 ) ) ;
#18424 = CARTESIAN_POINT ( 'NONE',  ( 119.6034614775786196, -6.344957434206665248, -7.627207830600338134 ) ) ;
#18425 = ORIENTED_EDGE ( 'NONE', *, *, #41490, .T. ) ;
#18426 = CARTESIAN_POINT ( 'NONE',  ( 125.0386814775786490, -5.568102603701690967, -18.34339073538286513 ) ) ;
#18427 = CARTESIAN_POINT ( 'NONE',  ( 65.35735161495482259, -2.416243571375609189, -8.473654787043400916 ) ) ;
#18428 = CARTESIAN_POINT ( 'NONE',  ( 121.9966691406318660, 0.3208234527006321724, -15.99825685930877839 ) ) ;
#18429 = CARTESIAN_POINT ( 'NONE',  ( 115.1220548109119761, -1.833838273342658809, -17.42832698103878286 ) ) ;
#18430 = CYLINDRICAL_SURFACE ( 'NONE', #20091, 8.000000000000001776 ) ;
#18431 = EDGE_CURVE ( 'NONE', #38238, #854, #23736, .T. ) ;
#18432 = CARTESIAN_POINT ( 'NONE',  ( 64.01282776924008999, -34.86145050234441811, -5.893215200338315363 ) ) ;
#18433 = CARTESIAN_POINT ( 'NONE',  ( 118.8660148109119774, 0.1319031606808879209, -14.10382304977623669 ) ) ;
#18434 = CYLINDRICAL_SURFACE ( 'NONE', #41141, 1.999999999999998890 ) ;
#18435 = AXIS2_PLACEMENT_3D ( 'NONE', #15531, #12798, #26699 ) ;
#18436 = CARTESIAN_POINT ( 'NONE',  ( 121.4187148109119789, -3.505236298600246325, -18.68346056562440793 ) ) ;
#18437 = CIRCLE ( 'NONE', #35166, 2.000000000000000444 ) ;
#18438 = PLANE ( 'NONE',  #22321 ) ;
#18439 = CARTESIAN_POINT ( 'NONE',  ( 122.2128881442453263, -7.643976991954077427, -18.09477374809248928 ) ) ;
#18440 = CARTESIAN_POINT ( 'NONE',  ( 112.3991748109119868, -8.166667518702817929, -8.995218007635859436 ) ) ;
#18441 = CARTESIAN_POINT ( 'NONE',  ( 120.7379948109119709, -10.63000616557722466, -14.87417383870573495 ) ) ;
#18442 = CARTESIAN_POINT ( 'NONE',  ( 113.4202548109119846, -10.30919188438810075, -12.61870101168855918 ) ) ;
#18443 = LINE ( 'NONE', #10922, #38001 ) ;
#18444 = CARTESIAN_POINT ( 'NONE',  ( 120.7947214775786193, -0.8288870151387760510, -10.36305467784173118 ) ) ;
#18445 = ORIENTED_EDGE ( 'NONE', *, *, #3885, .T. ) ;
#18446 = CARTESIAN_POINT ( 'NONE',  ( 119.0929214775786278, -5.638512984488999180, -18.83840828888717311 ) ) ;
#18447 = CARTESIAN_POINT ( 'NONE',  ( 114.4413952545248350, -9.868328341294098749, -15.46607636864997204 ) ) ;
#18448 = LINE ( 'NONE', #24829, #2976 ) ;
#18449 = CONICAL_SURFACE ( 'NONE', #10449, 1.610000000000000986, 0.9599310885968765916 ) ;
#18450 = LINE ( 'NONE', #42617, #35537 ) ;
#18451 = CARTESIAN_POINT ( 'NONE',  ( 119.8338581739443072, -4.756192495830076084, -19.39047411591439385 ) ) ;
#18452 = CARTESIAN_POINT ( 'NONE',  ( 124.9357681442453014, -1.834011780172310813, -8.268836392978581529 ) ) ;
#18453 = VERTEX_POINT ( 'NONE', #9198 ) ;
#18454 = CARTESIAN_POINT ( 'NONE',  ( 122.2696148109119889, -5.574606645277164318, -18.38911715685844683 ) ) ;
#18455 = CARTESIAN_POINT ( 'NONE',  ( 120.1601735609119856, 0.6414057260225851653, -11.69287257290600657 ) ) ;
#18456 = DIRECTION ( 'NONE',  ( 0.000000000000000000, 0.000000000000000000, -1.000000000000000000 ) ) ;
#18457 = CARTESIAN_POINT ( 'NONE',  ( 125.7866681442452688, -0.4660016031367893996, -10.09054647747474043 ) ) ;
#18458 = CARTESIAN_POINT ( 'NONE',  ( 109.7880358795247986, -8.402594152722688392, -9.854619843455216355 ) ) ;
#18459 = ORIENTED_EDGE ( 'NONE', *, *, #6734, .F. ) ;
#18460 = CARTESIAN_POINT ( 'NONE',  ( 114.9518748109119883, -1.834011780172310813, -8.268836392978581529 ) ) ;
#18461 = CARTESIAN_POINT ( 'NONE',  ( 125.4463081442452932, -5.638512984488999180, -18.83840828888717311 ) ) ;
#18462 = CARTESIAN_POINT ( 'NONE',  ( 120.1707281442453166, -9.565557343593413364, -10.61323700422348004 ) ) ;
#18463 = CARTESIAN_POINT ( 'NONE',  ( 126.4750299824202102, -3.550610268942888670, -8.435960360623607102 ) ) ;
#18464 =( NAMED_UNIT ( * ) SI_UNIT ( $, .STERADIAN. ) SOLID_ANGLE_UNIT ( ) );
#18465 = CARTESIAN_POINT ( 'NONE',  ( 111.6617281442453304, 0.4262465694468514643, -12.03445270309931736 ) ) ;
#18466 = CARTESIAN_POINT ( 'NONE',  ( 69.69189222815028018, -41.76310523276638520, -15.89321520033831447 ) ) ;
#18467 = DIRECTION ( 'NONE',  ( -0.5735764363510450492, -0.3127926500124816878, 0.7570804645221038687 ) ) ;
#18468 = CARTESIAN_POINT ( 'NONE',  ( 111.8319081442453182, -5.638512984488999180, -18.83840828888717311 ) ) ;
#18469 = ORIENTED_EDGE ( 'NONE', *, *, #29924, .F. ) ;
#18470 = EDGE_CURVE ( 'NONE', #1411, #30218, #19358, .T. ) ;
#18471 = CARTESIAN_POINT ( 'NONE',  ( 115.6220983795247861, -8.402594152722688392, -16.93181055722141792 ) ) ;
#18472 = AXIS2_PLACEMENT_3D ( 'NONE', #24235, #34688, #3476 ) ;
#18473 = CARTESIAN_POINT ( 'NONE',  ( 120.5110881442453206, -6.344957434206665248, -7.627207830600338134 ) ) ;
#18474 = CARTESIAN_POINT ( 'NONE',  ( 66.56178116512437271, 0.2059559948650140082, -15.23405342170197940 ) ) ;
#18475 = ORIENTED_EDGE ( 'NONE', *, *, #9456, .T. ) ;
#18476 = CARTESIAN_POINT ( 'NONE',  ( 121.1981266692503851, -2.311015703046761072, -18.04188382666269774 ) ) ;
#18477 = CARTESIAN_POINT ( 'NONE',  ( 124.3685014775786328, -10.63000616557722466, -14.87417383870573495 ) ) ;
#18478 = CARTESIAN_POINT ( 'NONE',  ( 127.0915067942438270, -4.531132641640684078, -18.81955951406810712 ) ) ;
#18479 = CARTESIAN_POINT ( 'NONE',  ( 124.7655881442452852, -9.859900752359378018, -12.68260735090039759 ) ) ;
#18480 = AXIS2_PLACEMENT_3D ( 'NONE', #38829, #10809, #24932 ) ;
#18481 = VERTEX_POINT ( 'NONE', #8972 ) ;
#18482 = CARTESIAN_POINT ( 'NONE',  ( 118.0151148109119816, -10.63000616557722466, -14.87417383870573495 ) ) ;
#18483 = ADVANCED_FACE ( 'NONE', ( #39976 ), #2339, .F. ) ;
#18484 = CARTESIAN_POINT ( 'NONE',  ( 79.43841117369071014, 5.060937148469339064, -20.42529936998274209 ) ) ;
#18485 = LINE ( 'NONE', #4333, #33078 ) ;
#18486 = CARTESIAN_POINT ( 'NONE',  ( 112.0588148109119828, -9.859900752359374465, -12.68260735090039404 ) ) ;
#18487 = CARTESIAN_POINT ( 'NONE',  ( 151.2860562277021472, -4.863998795839242995, -13.39321520033831447 ) ) ;
#18488 = FACE_OUTER_BOUND ( 'NONE', #23538, .T. ) ;
#18489 = CARTESIAN_POINT ( 'NONE',  ( 111.4915481442453142, -1.833838273342658365, -17.42832698103878286 ) ) ;
#18490 = CARTESIAN_POINT ( 'NONE',  ( 124.4252281442452812, -0.8288870151387760510, -10.36305467784173118 ) ) ;
#18491 = CARTESIAN_POINT ( 'NONE',  ( 116.7165501589519749, -6.821145072361184170, -18.12697020542095672 ) ) ;
#18492 = CARTESIAN_POINT ( 'NONE',  ( 124.5954081442453116, -6.222761293078241884, -8.102969835052219238 ) ) ;
#18493 = CARTESIAN_POINT ( 'NONE',  ( 112.8529881442453302, -7.894159318335828068, -9.358103419637847864 ) ) ;
#18494 = CARTESIAN_POINT ( 'NONE',  ( 119.0361948109119652, -7.893985811506177619, -18.51759400769804742 ) ) ;
#18495 = VECTOR ( 'NONE', #26504, 1000.000000000000227 ) ;
#18496 = CARTESIAN_POINT ( 'NONE',  ( 126.4162218615820450, -8.599963967683439847, -16.86356328481144118 ) ) ;
#18497 = DIRECTION ( 'NONE',  ( 0.8636456077245080465, -0.5040994586965603652, 0.000000000000000000 ) ) ;
#18498 = CARTESIAN_POINT ( 'NONE',  ( 115.7610046295247912, -4.863998795839590272, -18.39754474579285315 ) ) ;
#18499 = CARTESIAN_POINT ( 'NONE',  ( 114.7886608795247696, -1.325403438956436419, -16.93181055722141792 ) ) ;
#18500 = CARTESIAN_POINT ( 'NONE',  ( 126.7702028005534061, -9.890968229443798165, -11.79150890346986280 ) ) ;
#18501 = CARTESIAN_POINT ( 'NONE',  ( 115.4624148109119943, -5.638512984488999180, -18.83840828888717311 ) ) ;
#18502 = ORIENTED_EDGE ( 'NONE', *, *, #2285, .T. ) ;
#18503 = CARTESIAN_POINT ( 'NONE',  ( 113.4202548109119846, 0.1319031606808879209, -14.10382304977623669 ) ) ;
#18504 = CARTESIAN_POINT ( 'NONE',  ( 108.1211608795247798, -8.938348069036489818, -9.318865927141430916 ) ) ;
#18505 = CARTESIAN_POINT ( 'NONE',  ( 70.19189222814998175, -53.54563792646638376, -34.62107767336419073 ) ) ;
#18506 = CARTESIAN_POINT ( 'NONE',  ( 112.4559014775786778, -0.1624402480850797581, -16.17319339645315424 ) ) ;
#18507 = CARTESIAN_POINT ( 'NONE',  ( 122.4965214775786251, 0.1319031606808862001, -14.10382304977622603 ) ) ;
#18508 = DIRECTION ( 'NONE',  ( 0.000000000000000000, 0.000000000000000000, 1.000000000000000000 ) ) ;
#18509 = CARTESIAN_POINT ( 'NONE',  ( 117.6180281442453150, -0.4660016031367893996, -10.09054647747474043 ) ) ;
#18510 = CARTESIAN_POINT ( 'NONE',  ( 110.4825671295247815, -10.62599879583958540, -13.39321520033831447 ) ) ;
#18511 = CARTESIAN_POINT ( 'NONE',  ( 111.0381921295247878, -9.868328341294093420, -13.39321520033831447 ) ) ;
#18512 = ORIENTED_EDGE ( 'NONE', *, *, #15069, .T. ) ;
#18513 = CARTESIAN_POINT ( 'NONE',  ( 126.4262034847003520, -7.476899408362951860, -9.008790208301181934 ) ) ;
#18514 = CARTESIAN_POINT ( 'NONE',  ( 118.0151148109119816, 0.4262465694468514643, -12.03445270309931736 ) ) ;
#18515 = CARTESIAN_POINT ( 'NONE',  ( 116.3133148109119759, -7.893985811506177619, -18.51759400769804742 ) ) ;
#18516 = PLANE ( 'NONE',  #42363 ) ;
#18517 = CARTESIAN_POINT ( 'NONE',  ( 69.36136150295220659, -61.83659016559353461, -34.83262201967072258 ) ) ;
#18518 = CARTESIAN_POINT ( 'NONE',  ( 121.5888948109119809, 0.1319031606808879209, -14.10382304977623669 ) ) ;
#18519 = CARTESIAN_POINT ( 'NONE',  ( 116.1431348109119881, 0.1319031606808879209, -14.10382304977623669 ) ) ;
#18520 = ORIENTED_EDGE ( 'NONE', *, *, #27569, .T. ) ;
#18521 = CARTESIAN_POINT ( 'NONE',  ( 123.5633766859119760, -9.033780868592240054, -16.85052413769862056 ) ) ;
#18522 = LINE ( 'NONE', #14878, #22224 ) ;
#18523 = CARTESIAN_POINT ( 'NONE',  ( 118.7525614775786380, -1.833838273342659253, -17.42832698103878286 ) ) ;
#18524 = VERTEX_POINT ( 'NONE', #40664 ) ;
#18525 = CARTESIAN_POINT ( 'NONE',  ( 127.7429221096414977, -10.18827139786943370, -15.59882366901442019 ) ) ;
#18526 = CARTESIAN_POINT ( 'NONE',  ( 113.7038881442453402, -3.383040157471821630, -19.15922257007629170 ) ) ;
#18527 = CIRCLE ( 'NONE', #326, 1.199999999999999067 ) ;
#18528 = CARTESIAN_POINT ( 'NONE',  ( 114.7886608795247696, -8.938348069036489818, -9.318865927141430916 ) ) ;
#18529 = CARTESIAN_POINT ( 'NONE',  ( 125.7299414775786346, -10.15424416112533912, -14.75197769757731336 ) ) ;
#18530 = ORIENTED_EDGE ( 'NONE', *, *, #31267, .F. ) ;
#18531 = ORIENTED_EDGE ( 'NONE', *, *, #861, .T. ) ;
#18532 = CARTESIAN_POINT ( 'NONE',  ( 122.0994348109119443, -10.15424416112533912, -14.75197769757731336 ) ) ;
#18533 = ADVANCED_FACE ( 'NONE', ( #19911 ), #40206, .T. ) ;
#18534 = CARTESIAN_POINT ( 'NONE',  ( 117.5613014775786525, -10.15424416112533912, -14.75197769757731336 ) ) ;
#18535 = CARTESIAN_POINT ( 'NONE',  ( 111.2184548109119788, -2.495269033102075262, -17.79652296963211455 ) ) ;
#18536 = DIRECTION ( 'NONE',  ( 0.000000000000000000, 0.000000000000000000, 1.000000000000000000 ) ) ;
#18537 = ORIENTED_EDGE ( 'NONE', *, *, #28384, .T. ) ;
#18538 = CARTESIAN_POINT ( 'NONE',  ( 112.1441723425591590, -8.920991669690657488, -16.34987411667529145 ) ) ;
#18539 = CARTESIAN_POINT ( 'NONE',  ( 61.80837279822206654, -65.83902806826597498, -43.67070380127381668 ) ) ;
#18540 = CARTESIAN_POINT ( 'NONE',  ( 111.0381921295247878, 0.8980012041604618078, -13.39321520033831447 ) ) ;
#18541 = CARTESIAN_POINT ( 'NONE',  ( 113.9875214775786532, -0.4660016031367893996, -10.09054647747474043 ) ) ;
#18542 = CARTESIAN_POINT ( 'NONE',  ( 125.7866681442452688, -8.899110576539710493, -16.42337572283490132 ) ) ;
#18543 = CARTESIAN_POINT ( 'NONE',  ( 119.7736414775786358, 0.1319031606808879209, -14.10382304977623669 ) ) ;
#18544 = DIRECTION ( 'NONE',  ( 0.000000000000000000, -0.6161630946014903243, -0.7876185884367603585 ) ) ;
#18545 = VERTEX_POINT ( 'NONE', #2568 ) ;
#18546 = CARTESIAN_POINT ( 'NONE',  ( 120.2274548109119934, -9.859900752359374465, -12.68260735090039404 ) ) ;
#18547 = VECTOR ( 'NONE', #139, 999.9999999999998863 ) ;
#18548 = DIRECTION ( 'NONE',  ( 1.000000000000000000, 0.000000000000000000, 0.000000000000000000 ) ) ;
#18549 = CARTESIAN_POINT ( 'NONE',  ( 117.0111608795247946, -1.325403438956436419, -16.93181055722141792 ) ) ;
#18550 = CARTESIAN_POINT ( 'NONE',  ( 114.6497546295247929, -4.863998795839590272, -7.631215200338315796 ) ) ;
#18551 = CARTESIAN_POINT ( 'NONE',  ( 118.0151148109119816, -10.63000616557722466, -14.87417383870573495 ) ) ;
#18552 = ORIENTED_EDGE ( 'NONE', *, *, #6433, .F. ) ;
#18553 = CARTESIAN_POINT ( 'NONE',  ( 117.7882081442453170, -6.344957434206665248, -7.627207830600338134 ) ) ;
#18554 = CARTESIAN_POINT ( 'NONE',  ( 92.32016463086877422, -25.99489077589524300, -13.39321520033831447 ) ) ;
#18555 = CARTESIAN_POINT ( 'NONE',  ( 107.3571765045248299, -7.250697342233347165, -19.15521520033831138 ) ) ;
#18556 = CARTESIAN_POINT ( 'NONE',  ( 116.3133148109119759, -7.893985811506177619, -18.51759400769804742 ) ) ;
#18557 = CARTESIAN_POINT ( 'NONE',  ( 115.8027748109119841, -0.4660016031367893996, -10.09054647747474043 ) ) ;
#18559 = CIRCLE ( 'NONE', #9092, 0.8509999999999994236 ) ;
#18558 = CARTESIAN_POINT ( 'NONE',  ( 126.3243314201118466, -9.906486255840077249, -13.06818223642682675 ) ) ;
#18560 = CARTESIAN_POINT ( 'NONE',  ( 79.05243529145373316, 4.793396140045460108, -4.893215200338314474 ) ) ;
#18561 = CARTESIAN_POINT ( 'NONE',  ( 107.2182702545248105, 0.1403307496149616695, -11.32035403202665336 ) ) ;
#18562 = VERTEX_POINT ( 'NONE', #16497 ) ;
#18563 = CARTESIAN_POINT ( 'NONE',  ( 115.9693640045247776, -10.62599879583958540, -11.00651665394454604 ) ) ;
#18564 = CARTESIAN_POINT ( 'NONE',  ( 109.2294435684327141, -10.04426263482621273, -15.20456221528482388 ) ) ;
#18565 = CARTESIAN_POINT ( 'NONE',  ( 121.1918081442452859, -10.15424416112533912, -14.75197769757731336 ) ) ;
#18566 = CARTESIAN_POINT ( 'NONE',  ( 113.1912390045248031, -9.868328341294098749, -11.32035403202665869 ) ) ;
#18567 = CARTESIAN_POINT ( 'NONE',  ( 107.2877233795247776, -8.938348069036489818, -17.46756447353520159 ) ) ;
#18568 = CARTESIAN_POINT ( 'NONE',  ( 112.8529881442453302, -7.894159318335828068, -9.358103419637847864 ) ) ;
#18569 = CARTESIAN_POINT ( 'NONE',  ( 114.2144281442453178, -1.833838273342658809, -17.42832698103878286 ) ) ;
#18570 = DIRECTION ( 'NONE',  ( 0.000000000000000000, -1.000000000000000000, 0.000000000000000000 ) ) ;
#18571 = CARTESIAN_POINT ( 'NONE',  ( 122.6099748109119929, -9.261995988541697145, -16.69588392320189030 ) ) ;
#18572 = CARTESIAN_POINT ( 'NONE',  ( 119.7169148109119874, -9.988377603198976828, -10.36322818467138340 ) ) ;
#18573 = ORIENTED_EDGE ( 'NONE', *, *, #3448, .T. ) ;
#18574 = CARTESIAN_POINT ( 'NONE',  ( 118.7525614775786380, -1.833838273342659253, -17.42832698103878286 ) ) ;
#18575 = DIRECTION ( 'NONE',  ( 0.1352586133457950590, 0.9908103287288504424, 0.000000000000000000 ) ) ;
#18576 = CARTESIAN_POINT ( 'NONE',  ( 120.2274548109119934, 0.5811942927096110934, -14.16772938898807510 ) ) ;
#18577 = CARTESIAN_POINT ( 'NONE',  ( 121.2485348109119769, -8.899110576539710493, -16.42337572283490132 ) ) ;
#18578 = ORIENTED_EDGE ( 'NONE', *, *, #35388, .F. ) ;
#18579 = CARTESIAN_POINT ( 'NONE',  ( 123.9146881442452894, -10.15424416112533912, -14.75197769757731336 ) ) ;
#18580 =( BOUNDED_CURVE ( )  B_SPLINE_CURVE ( 3, ( #9463, #9016, #2382, #40249 ),
 .UNSPECIFIED., .F., .F. ) 
 B_SPLINE_CURVE_WITH_KNOTS ( ( 4, 4 ),
 ( 3.141592653589795336, 4.712388980384689674 ),
 .UNSPECIFIED. ) 
 CURVE ( )  GEOMETRIC_REPRESENTATION_ITEM ( )  RATIONAL_B_SPLINE_CURVE ( ( 1.000000000000000000, 0.8047378541243649375, 0.8047378541243649375, 1.000000000000000000 ) ) 
 REPRESENTATION_ITEM ( '' )  );
#18581 = CARTESIAN_POINT ( 'NONE',  ( 119.4332814775786318, -0.4660016031367893996, -10.09054647747474043 ) ) ;
#18582 = CARTESIAN_POINT ( 'NONE',  ( 112.2289948109119848, -7.643976991954077427, -18.09477374809248928 ) ) ;
#18583 = CARTESIAN_POINT ( 'NONE',  ( 110.5520202545248054, -10.62599879583958717, -15.77991374673208469 ) ) ;
#18584 = AXIS2_PLACEMENT_3D ( 'NONE', #15320, #11683, #25589 ) ;
#18585 = CARTESIAN_POINT ( 'NONE',  ( 61.55121550910386219, -14.46605081255136049, -8.868903071359692802 ) ) ;
#18586 = CARTESIAN_POINT ( 'NONE',  ( 126.5495342817341253, 0.3014387667525698089, -13.43723796351942923 ) ) ;
#18587 = EDGE_CURVE ( 'NONE', #38119, #21905, #19772, .T. ) ;
#18588 = CARTESIAN_POINT ( 'NONE',  ( 112.2188952545247531, -9.868328341294098749, -15.46607636864997204 ) ) ;
#18589 = CARTESIAN_POINT ( 'NONE',  ( 118.6391081442452986, -4.089484607189486809, -7.948022111789456723 ) ) ;
#18590 = DIRECTION ( 'NONE',  ( 0.000000000000000000, 0.6004852223388321697, -0.7996358532186279566 ) ) ;
#18591 = CARTESIAN_POINT ( 'NONE',  ( 117.5613014775786525, -10.15424416112533912, -14.75197769757731336 ) ) ;
#18592 = CARTESIAN_POINT ( 'NONE',  ( 111.8886348109120092, -6.222761293078241884, -8.102969835052219238 ) ) ;
#18593 = CARTESIAN_POINT ( 'NONE',  ( 65.00050459711196993, -13.33302880096658249, -15.05917699090357509 ) ) ;
#18594 = CARTESIAN_POINT ( 'NONE',  ( 110.0658483795247804, -8.402594152722688392, -16.93181055722141792 ) ) ;
#18595 = CARTESIAN_POINT ( 'NONE',  ( 115.4056881442453317, -7.893985811506194494, -18.51759400769804031 ) ) ;
#18596 = CARTESIAN_POINT ( 'NONE',  ( 115.0644952477523901, -1.220279397241700758, -16.99638242193885063 ) ) ;
#18597 = EDGE_CURVE ( 'NONE', #2964, #23812, #15587, .T. ) ;
#18598 = CARTESIAN_POINT ( 'NONE',  ( 67.84197459855160162, -56.44012947280842241, -36.50803721828817316 ) ) ;
#18600 = CARTESIAN_POINT ( 'NONE',  ( 120.6812681442452941, -10.30919188438810075, -12.61870101168855918 ) ) ;
#18599 = CARTESIAN_POINT ( 'NONE',  ( 61.15360158040112282, -14.46165722119120822, -7.573710289374333549 ) ) ;
#18601 = CARTESIAN_POINT ( 'NONE',  ( 117.7882081442453170, -3.505236298600246325, -18.68346056562440793 ) ) ;
#18602 = CARTESIAN_POINT ( 'NONE',  ( 114.0442481442453300, -7.643976991954077427, -18.09477374809248928 ) ) ;
#18603 = ORIENTED_EDGE ( 'NONE', *, *, #3313, .T. ) ;
#18604 = CARTESIAN_POINT ( 'NONE',  ( 70.19189222814998175, -55.19510675323109439, -35.28085945431567438 ) ) ;
#18605 = FACE_OUTER_BOUND ( 'NONE', #4707, .T. ) ;
#18606 = CARTESIAN_POINT ( 'NONE',  ( 112.3578015045248861, -6.936859964151250502, -18.39754474579286025 ) ) ;
#18607 = CARTESIAN_POINT ( 'NONE',  ( 120.3409081442453044, -8.899110576539710493, -16.42337572283490132 ) ) ;
#18608 = CARTESIAN_POINT ( 'NONE',  ( 123.1772414775786189, -5.574606645277164318, -18.38911715685844683 ) ) ;
#18609 = CARTESIAN_POINT ( 'NONE',  ( 116.2565881442453133, -0.8288870151387760510, -10.36305467784173118 ) ) ;
#18610 = CARTESIAN_POINT ( 'NONE',  ( 86.21326076097346913, -26.71771895156159715, -8.459066486029300336 ) ) ;
#18611 = CARTESIAN_POINT ( 'NONE',  ( 108.7462390045248242, 0.8980012041604421569, -15.77991374673208469 ) ) ;
#18612 = CIRCLE ( 'NONE', #17864, 2.000000000000000444 ) ;
#18613 = CARTESIAN_POINT ( 'NONE',  ( 124.8223148109119762, -10.15424416112533912, -14.75197769757731336 ) ) ;
#18614 = CARTESIAN_POINT ( 'NONE',  ( 124.3685014775786328, 0.4262465694468514643, -12.03445270309931736 ) ) ;
#18615 = DIRECTION ( 'NONE',  ( 0.000000000000000000, 0.6004852223388321697, -0.7996358532186279566 ) ) ;
#18616 = DIRECTION ( 'NONE',  ( 0.9609149988134838560, -0.1028163501681645386, 0.2570431154366520921 ) ) ;
#18617 = CARTESIAN_POINT ( 'NONE',  ( 119.3267360609119692, -3.387241619883791355, -18.17469012370385073 ) ) ;
#18618 = CARTESIAN_POINT ( 'NONE',  ( 114.6497546295247929, -4.863998795839590272, -7.631215200338315796 ) ) ;
#18619 = EDGE_CURVE ( 'NONE', #24335, #31497, #36543, .T. ) ;
#18620 = DIRECTION ( 'NONE',  ( 0.000000000000000000, 0.000000000000000000, 1.000000000000000000 ) ) ;
#18621 = CARTESIAN_POINT ( 'NONE',  ( 94.20708369096698220, -25.77760949922539879, -12.57042127303408385 ) ) ;
#18622 = CARTESIAN_POINT ( 'NONE',  ( 117.7314814775786260, -4.089484607189486809, -7.948022111789456723 ) ) ;
#18623 = CARTESIAN_POINT ( 'NONE',  ( 117.3911214775786505, -1.561330072975668504, -17.79121239304076951 ) ) ;
#18624 = CARTESIAN_POINT ( 'NONE',  ( 108.0517077545248696, -7.250697342233347165, -7.631215200338321125 ) ) ;
#18625 = CARTESIAN_POINT ( 'NONE',  ( 114.1577014775786552, -6.344957434206662583, -7.627207830600332805 ) ) ;
#18626 = EDGE_CURVE ( 'NONE', #6780, #15033, #43236, .T. ) ;
#18627 = ADVANCED_FACE ( 'NONE', ( #20147 ), #27878, .F. ) ;
#18628 = DIRECTION ( 'NONE',  ( 0.3445294493088594256, 0.9387755102040817867, 0.000000000000000000 ) ) ;
#18629 = ORIENTED_EDGE ( 'NONE', *, *, #20936, .T. ) ;
#18630 = CARTESIAN_POINT ( 'NONE',  ( 116.3198046295247963, -4.863998795839590272, -8.393215200338314474 ) ) ;
#18631 = CIRCLE ( 'NONE', #12083, 1.499999999999996225 ) ;
#18632 = CARTESIAN_POINT ( 'NONE',  ( 117.1642148109119859, -9.261995988541697145, -16.69588392320189030 ) ) ;
#18633 = CARTESIAN_POINT ( 'NONE',  ( 122.3263414775786373, -3.505236298600246325, -18.68346056562440793 ) ) ;
#18634 = CARTESIAN_POINT ( 'NONE',  ( 112.7395348109119766, -4.153390946401321671, -8.397313243818183892 ) ) ;
#18635 = CARTESIAN_POINT ( 'NONE',  ( 120.3409081442453044, -0.4660016031367893996, -10.09054647747474043 ) ) ;
#18636 = CARTESIAN_POINT ( 'NONE',  ( 115.6915515045247531, -2.477300249445798297, -7.631215200338321125 ) ) ;
#18637 = CARTESIAN_POINT ( 'NONE',  ( 118.1285681442453068, -2.084020599724406786, -8.691656652584148546 ) ) ;
#18638 = CARTESIAN_POINT ( 'NONE',  ( 120.4379860609119675, -6.564341423271550902, -7.887810678476487425 ) ) ;
#18639 = CARTESIAN_POINT ( 'NONE',  ( 85.83930302032702286, -9.140269361470597431, -14.14321520033831625 ) ) ;
#18640 = ORIENTED_EDGE ( 'NONE', *, *, #13888, .F. ) ;
#18641 = CARTESIAN_POINT ( 'NONE',  ( 124.1190016859119680, -9.665098340737509730, -17.37397104707595474 ) ) ;
#18642 = CARTESIAN_POINT ( 'NONE',  ( 119.0361948109119652, -7.893985811506177619, -18.51759400769804742 ) ) ;
#18643 = EDGE_CURVE ( 'NONE', #42460, #39949, #5988, .T. ) ;
#18644 = ORIENTED_EDGE ( 'NONE', *, *, #20054, .F. ) ;
#18645 = CARTESIAN_POINT ( 'NONE',  ( 60.19189222814998175, -66.20485342690169261, -45.06987807991851724 ) ) ;
#18646 = DIRECTION ( 'NONE',  ( 0.9498278979187094739, 0.3127730236694427068, -0.000000000000000000 ) ) ;
#18647 = DIRECTION ( 'NONE',  ( -0.000000000000000000, -0.9284778069183721172, -0.3713878862591650232 ) ) ;
#18648 = CARTESIAN_POINT ( 'NONE',  ( 115.2355081442453155, 0.1319031606808879209, -14.10382304977623669 ) ) ;
#18649 = DIRECTION ( 'NONE',  ( -0.000000000000000000, -0.9284778069183718952, -0.3713878862591649677 ) ) ;
#18650 = CARTESIAN_POINT ( 'NONE',  ( 64.35867204304231848, -35.30545456751979572, -5.871741255084275579 ) ) ;
#18651 = CARTESIAN_POINT ( 'NONE',  ( 121.9292548109119849, -7.894159318335828068, -9.358103419637847864 ) ) ;
#18652 = CARTESIAN_POINT ( 'NONE',  ( 121.2485348109119769, -0.4660016031367928413, -10.09054647747473510 ) ) ;
#18653 = VECTOR ( 'NONE', #25308, 999.9999999999998863 ) ;
#18654 = CARTESIAN_POINT ( 'NONE',  ( 125.7866681442452688, -8.899110576539710493, -16.42337572283490132 ) ) ;
#18655 = EDGE_CURVE ( 'NONE', #27212, #32081, #17392, .T. ) ;
#18656 =( GEOMETRIC_REPRESENTATION_CONTEXT ( 3 ) GLOBAL_UNCERTAINTY_ASSIGNED_CONTEXT ( ( #27891 ) ) GLOBAL_UNIT_ASSIGNED_CONTEXT ( ( #14138, #13313, #27220 ) ) REPRESENTATION_CONTEXT ( 'NONE', 'WORKASPACE' ) );
#18657 = CARTESIAN_POINT ( 'NONE',  ( 125.2958570204316118, -11.52802372718165103, -16.06387753721113754 ) ) ;
#18658 = CARTESIAN_POINT ( 'NONE',  ( 122.4965214775786251, 0.1319031606808879209, -14.10382304977623669 ) ) ;
#18659 = CARTESIAN_POINT ( 'NONE',  ( 112.3424481442453384, -6.344957434206662583, -7.627207830600332805 ) ) ;
#18660 = CARTESIAN_POINT ( 'NONE',  ( 118.6958348109119754, -6.344957434206665248, -7.627207830600338134 ) ) ;
#18661 = CARTESIAN_POINT ( 'NONE',  ( 112.3424481442453384, -6.344957434206662583, -7.627207830600332805 ) ) ;
#18662 = CARTESIAN_POINT ( 'NONE',  ( 121.9470836909669913, -24.14644159042263993, -12.62951656296512937 ) ) ;
#18663 = CARTESIAN_POINT ( 'NONE',  ( 119.7169148109119874, -0.1624402480850797581, -16.17319339645315424 ) ) ;
#18664 = ORIENTED_EDGE ( 'NONE', *, *, #19476, .T. ) ;
#18665 = CARTESIAN_POINT ( 'NONE',  ( 119.3765548109119834, 0.9020085738987339008, -11.91225656197089222 ) ) ;
#18666 = CARTESIAN_POINT ( 'NONE',  ( 112.8439733795247832, -1.325403438956436419, -9.854619843455211026 ) ) ;
#18667 = CARTESIAN_POINT ( 'NONE',  ( 82.59722093989569203, -31.76965857943681826, -23.00835853622210436 ) ) ;
#18668 = CARTESIAN_POINT ( 'NONE',  ( 113.7606148109119886, -7.894159318335828068, -9.358103419637847864 ) ) ;
#18669 = CARTESIAN_POINT ( 'NONE',  ( 120.0907204359119760, 1.345710702986149920, -13.97328579221134071 ) ) ;
#18670 = AXIS2_PLACEMENT_3D ( 'NONE', #44543, #13755, #27884 ) ;
#18671 = CARTESIAN_POINT ( 'NONE',  ( 125.5030348109119558, -3.383040157471821630, -19.15922257007629170 ) ) ;
#18672 = VERTEX_POINT ( 'NONE', #2800 ) ;
#18673 = CARTESIAN_POINT ( 'NONE',  ( 121.5321681442453183, -0.1624402480850797581, -16.17319339645315424 ) ) ;
#18674 = CARTESIAN_POINT ( 'NONE',  ( 121.6881423109119709, -9.959231468620755479, -10.70263013195267199 ) ) ;
#18675 = CARTESIAN_POINT ( 'NONE',  ( 123.2161110609119561, -3.163656168406935087, -18.89861972220014508 ) ) ;
#18676 = ADVANCED_FACE ( 'NONE', ( #41792 ), #1720, .T. ) ;
#18677 = CARTESIAN_POINT ( 'NONE',  ( 111.8424481442453242, -6.210324830718715994, -8.151390318758329201 ) ) ;
#18678 = CARTESIAN_POINT ( 'NONE',  ( 106.2459265045248173, -2.791137627527939813, -8.388885654883777576 ) ) ;
#18679 = CIRCLE ( 'NONE', #44177, 4.699999999999999289 ) ;
#18680 = VERTEX_POINT ( 'NONE', #27208 ) ;
#18681 = CARTESIAN_POINT ( 'NONE',  ( 116.2565881442452991, -9.261995988541697145, -16.69588392320189030 ) ) ;
#18682 = CARTESIAN_POINT ( 'NONE',  ( 65.10287265247757205, -0.4742552606671820992, -16.39321520033831447 ) ) ;
#18683 = CARTESIAN_POINT ( 'NONE',  ( 122.4965214775786251, 0.1319031606808879209, -14.10382304977623669 ) ) ;
#18684 = CARTESIAN_POINT ( 'NONE',  ( 90.06246830635160450, -25.99489077589524300, -13.39321520033831625 ) ) ;
#18685 = LINE ( 'NONE', #8196, #13302 ) ;
#18686 = EDGE_CURVE ( 'NONE', #16965, #10924, #27435, .T. ) ;
#18687 = CARTESIAN_POINT ( 'NONE',  ( 90.04708369096697140, -26.47086644115443832, -13.58986759946190936 ) ) ;
#18688 = CARTESIAN_POINT ( 'NONE',  ( 123.7637130757767352, -0.9924539043446216624, -17.29976612834909133 ) ) ;
#18689 = PRESENTATION_STYLE_ASSIGNMENT (( #7971 ) ) ;
#18690 = VERTEX_POINT ( 'NONE', #7117 ) ;
#18691 = VECTOR ( 'NONE', #16870, 1000.000000000000000 ) ;
#18692 = CARTESIAN_POINT ( 'NONE',  ( 117.1500671295247713, 0.1403307496149613920, -13.39321520033831447 ) ) ;
#18693 = CARTESIAN_POINT ( 'NONE',  ( 119.3198281442452924, 0.5811942927096110934, -14.16772938898807510 ) ) ;
#18694 = CARTESIAN_POINT ( 'NONE',  ( 137.1799701741892932, -8.482991601570400775, -17.29899319809113578 ) ) ;
#18695 = EDGE_LOOP ( 'NONE', ( #26979, #19101, #44226, #22335, #9535 ) ) ;
#18696 = CARTESIAN_POINT ( 'NONE',  ( 112.1155414775786454, 0.9020085738987339008, -11.91225656197089222 ) ) ;
#18697 = CARTESIAN_POINT ( 'NONE',  ( 124.7655881442452852, 0.5811942927096110934, -14.16772938898807510 ) ) ;
#18698 = CARTESIAN_POINT ( 'NONE',  ( 123.1205148109119563, -7.643976991954077427, -18.09477374809248928 ) ) ;
#18699 = ORIENTED_EDGE ( 'NONE', *, *, #25117, .F. ) ;
#18700 = CARTESIAN_POINT ( 'NONE',  ( 116.4267681442453153, -3.383040157471821630, -19.15922257007629170 ) ) ;
#18702 = CARTESIAN_POINT ( 'NONE',  ( 124.5059548109119731, -4.863998795839242995, -13.39321520033831447 ) ) ;
#18701 = CONICAL_SURFACE ( 'NONE', #28896, 2.999999999999999556, 0.9599310885968830309 ) ;
#18703 = DIRECTION ( 'NONE',  ( -1.000000000000000000, 0.000000000000000000, 0.000000000000000000 ) ) ;
#18704 = DIRECTION ( 'NONE',  ( 0.000000000000000000, -1.000000000000000000, -6.938893903907222067E-15 ) ) ;
#18705 = CARTESIAN_POINT ( 'NONE',  ( 111.4361666677645957, -2.488018885432666139, -17.80617762523714021 ) ) ;
#18706 = CARTESIAN_POINT ( 'NONE',  ( 126.1837548109119211, -10.63000616557722466, -14.87417383870573495 ) ) ;
#18707 = AXIS2_PLACEMENT_3D ( 'NONE', #36599, #5375, #19292 ) ;
#18708 = CARTESIAN_POINT ( 'NONE',  ( 90.45092582798827152, -27.84333996136784961, -14.15691383771150136 ) ) ;
#18709 = DIRECTION ( 'NONE',  ( -0.8949343913984423304, 0.1703803081152067689, -0.4123869368673877545 ) ) ;
#18710 = CARTESIAN_POINT ( 'NONE',  ( 111.6617281442453304, 0.4262465694468514643, -12.03445270309931736 ) ) ;
#18711 = CARTESIAN_POINT ( 'NONE',  ( 126.5808414775786446, -9.859900752359378018, -12.68260735090039759 ) ) ;
#18712 = CARTESIAN_POINT ( 'NONE',  ( 116.7470998475920254, -5.364568849815520402, -18.53181687022155799 ) ) ;
#18713 = CARTESIAN_POINT ( 'NONE',  ( 123.0637881442452937, -8.899110576539710493, -16.42337572283490132 ) ) ;
#18714 = CARTESIAN_POINT ( 'NONE',  ( 85.45605303719084134, -15.74807682313488222, -13.39321520033831447 ) ) ;
#18715 = CARTESIAN_POINT ( 'NONE',  ( 119.8870948109119752, -9.261995988541697145, -16.69588392320189030 ) ) ;
#18716 = ADVANCED_FACE ( 'NONE', ( #44538 ), #7513, .F. ) ;
#18717=STYLED_ITEM('',(#45162),#6587);
#18718 = CARTESIAN_POINT ( 'NONE',  ( 117.4836465278262807, -1.036737761566197014, -17.24079555149560861 ) ) ;
#18719 = CARTESIAN_POINT ( 'NONE',  ( 115.8999108795247821, -8.938348069036489818, -9.318865927141430916 ) ) ;
#18720 = CARTESIAN_POINT ( 'NONE',  ( 109.8574890045248509, -9.868328341294098749, -11.32035403202665869 ) ) ;
#18721 = CARTESIAN_POINT ( 'NONE',  ( 110.8992858795247827, -8.402594152722688392, -9.854619843455216355 ) ) ;
#18722 = DIRECTION ( 'NONE',  ( 0.000000000000000000, -0.3818493186865936084, 0.9242245927363024194 ) ) ;
#18723 = CARTESIAN_POINT ( 'NONE',  ( 116.5969481442453031, 0.5811942927096154232, -14.16772938898807155 ) ) ;
#18724 = ORIENTED_EDGE ( 'NONE', *, *, #30687, .F. ) ;
#18725 = CARTESIAN_POINT ( 'NONE',  ( 115.7460481442453357, -10.15424416112533912, -14.75197769757731336 ) ) ;
#18726 = CARTESIAN_POINT ( 'NONE',  ( 108.9545983795247821, -0.7896495226426338832, -9.318865927141430916 ) ) ;
#18727 = FACE_OUTER_BOUND ( 'NONE', #30156, .T. ) ;
#18728 = CARTESIAN_POINT ( 'NONE',  ( 126.0135748109119902, -8.166667518702819706, -8.995218007635861213 ) ) ;
#18729 = CYLINDRICAL_SURFACE ( 'NONE', #11682, 2.000000000000003109 ) ;
#18730 = CARTESIAN_POINT ( 'NONE',  ( -13.78505786849295411, -3.796669023460440329, -18.09332867002095213 ) ) ;
#18731 = CARTESIAN_POINT ( 'NONE',  ( 116.9373081442452929, -8.166667518702817929, -8.995218007635861213 ) ) ;
#18732 = CARTESIAN_POINT ( 'NONE',  ( 109.8574890045247940, 0.8980012041604421569, -15.77991374673208469 ) ) ;
#18733 = CARTESIAN_POINT ( 'NONE',  ( 109.7880358795247986, -8.402594152722688392, -9.854619843455216355 ) ) ;
#18734 = EDGE_LOOP ( 'NONE', ( #26412, #27883, #19705 ) ) ;
#18735 = DIRECTION ( 'NONE',  ( -0.4461977533474357216, 0.8271203734159378040, 0.3417300876246930907 ) ) ;
#18736 = CARTESIAN_POINT ( 'NONE',  ( 117.2776681442452968, -4.153390946401321671, -8.397313243818183892 ) ) ;
#18737 = CARTESIAN_POINT ( 'NONE',  ( 115.0653281442453277, -6.344957434206662583, -7.627207830600332805 ) ) ;
#18738 = CIRCLE ( 'NONE', #36194, 1.199999999999999512 ) ;
#18739 = EDGE_CURVE ( 'NONE', #29216, #37171, #167, .T. ) ;
#18740 = DIRECTION ( 'NONE',  ( -0.3127730236694430399, 0.9498278979187092519, 0.000000000000000000 ) ) ;
#18741 = CARTESIAN_POINT ( 'NONE',  ( 125.7866681442452688, -8.899110576539710493, -16.42337572283490132 ) ) ;
#18742 = CARTESIAN_POINT ( 'NONE',  ( 123.4608748109119745, 0.4262465694468514643, -12.03445270309931736 ) ) ;
#18743 = CARTESIAN_POINT ( 'NONE',  ( 116.3700414775786527, -4.153390946401321671, -8.397313243818183892 ) ) ;
#18744 = ORIENTED_EDGE ( 'NONE', *, *, #7475, .F. ) ;
#18745 = CARTESIAN_POINT ( 'NONE',  ( 120.6463454359119822, -11.07370829466463569, -12.81314460846529002 ) ) ;
#18746 = DIRECTION ( 'NONE',  ( 1.000000000000000000, 0.000000000000000000, -0.000000000000000000 ) ) ;
#18747 = CARTESIAN_POINT ( 'NONE',  ( 119.3765548109119834, -10.15424416112533912, -14.75197769757731336 ) ) ;
#18748 = EDGE_LOOP ( 'NONE', ( #15474, #5038 ) ) ;
#18749 = CARTESIAN_POINT ( 'NONE',  ( 120.2990798109119766, -7.200787124940443817, -17.81845355600750835 ) ) ;
#18750 = CARTESIAN_POINT ( 'NONE',  ( 113.9875214775786532, -0.4660016031367893996, -10.09054647747474043 ) ) ;
#18751 = VECTOR ( 'NONE', #2389, 1000.000000000000000 ) ;
#18752 = CARTESIAN_POINT ( 'NONE',  ( 107.2182702545248105, 0.1403307496149616695, -11.32035403202665336 ) ) ;
#18753 = CARTESIAN_POINT ( 'NONE',  ( 113.5337081442453240, -0.8288870151387760510, -10.36305467784173118 ) ) ;
#18754 = EDGE_LOOP ( 'NONE', ( #43981, #37874, #26009, #9388, #31433 ) ) ;
#18755 = ORIENTED_EDGE ( 'NONE', *, *, #40058, .F. ) ;
#18756 = CARTESIAN_POINT ( 'NONE',  ( 122.3263414775786373, -3.505236298600246325, -18.68346056562440793 ) ) ;
#18757 = CARTESIAN_POINT ( 'NONE',  ( 116.5402214775786405, -9.565557343593413364, -10.61323700422348004 ) ) ;
#18758 = CARTESIAN_POINT ( 'NONE',  ( 124.5444919965972161, -9.856391046268592859, -13.09751618074382584 ) ) ;
#18759 = CARTESIAN_POINT ( 'NONE',  ( 116.2565881442453133, -0.8288870151387560670, -10.36305467784175605 ) ) ;
#18760 = ORIENTED_EDGE ( 'NONE', *, *, #20644, .T. ) ;
#18761 = CYLINDRICAL_SURFACE ( 'NONE', #15005, 5.999999999999997335 ) ;
#18762 = CARTESIAN_POINT ( 'NONE',  ( 61.78267613169789740, -65.90120773829286804, -43.52498728833642616 ) ) ;
#18763 = CARTESIAN_POINT ( 'NONE',  ( 112.9828796295247884, -4.863998795839590272, -19.15521520033831493 ) ) ;
#18764 = AXIS2_PLACEMENT_3D ( 'NONE', #24264, #3273, #44566 ) ;
#18765 = CARTESIAN_POINT ( 'NONE',  ( 116.6536748109119941, 0.9020085738987339008, -11.91225656197089222 ) ) ;
#18767 = CARTESIAN_POINT ( 'NONE',  ( 116.0864081442453113, -0.1624402480850797581, -16.17319339645315424 ) ) ;
#18766 = CARTESIAN_POINT ( 'NONE',  ( 112.6260814775786514, -9.261995988541697145, -16.69588392320189030 ) ) ;
#18768 = CARTESIAN_POINT ( 'NONE',  ( 120.0005481442453146, -4.153390946401325223, -8.397313243818185668 ) ) ;
#18769 = CARTESIAN_POINT ( 'NONE',  ( 59.44377208703740223, -12.82110557137145967, -19.39321520033831447 ) ) ;
#18770 = ORIENTED_EDGE ( 'NONE', *, *, #12948, .F. ) ;
#18771 = CARTESIAN_POINT ( 'NONE',  ( 118.8092881442453290, -0.1624402480850797581, -16.17319339645315424 ) ) ;
#18772 = CARTESIAN_POINT ( 'NONE',  ( 85.15861813568058380, -25.99489077589524300, -13.39321520033831625 ) ) ;
#18773 = CARTESIAN_POINT ( 'NONE',  ( 111.6632702545248605, -10.62599879583958717, -15.77991374673208469 ) ) ;
#18774 = CARTESIAN_POINT ( 'NONE',  ( 116.5944421295247793, -9.868328341294093420, -13.39321520033831447 ) ) ;
#18775 = CARTESIAN_POINT ( 'NONE',  ( 116.2471765045247594, -7.250697342233347165, -19.15521520033831138 ) ) ;
#18776 = CARTESIAN_POINT ( 'NONE',  ( 117.1074881442453233, -10.63000616557722466, -14.87417383870573495 ) ) ;
#18777 = VERTEX_POINT ( 'NONE', #24017 ) ;
#18778 = CARTESIAN_POINT ( 'NONE',  ( 121.6456214775786293, -10.63000616557722466, -14.87417383870573495 ) ) ;
#18779 = CARTESIAN_POINT ( 'NONE',  ( 90.72400676789006013, -26.60966817898065884, -11.90521360603286816 ) ) ;
#18780 = CARTESIAN_POINT ( 'NONE',  ( 107.9128015045248219, -2.477300249445798297, -7.631215200338321125 ) ) ;
#18781 = CARTESIAN_POINT ( 'NONE',  ( 116.7104014775786425, -0.4660016031367893996, -10.09054647747474043 ) ) ;
#18782 = CARTESIAN_POINT ( 'NONE',  ( 116.0864081442453113, -9.988377603198976828, -10.36322818467138340 ) ) ;
#18783 = DIRECTION ( 'NONE',  ( 0.000000000000000000, 0.000000000000000000, -1.000000000000000000 ) ) ;
#18784 = CARTESIAN_POINT ( 'NONE',  ( 113.2858169107182249, -2.467220198592768199, -17.83387418641523325 ) ) ;
#18785 = CARTESIAN_POINT ( 'NONE',  ( 123.5880035264548837, -8.247323210606174015, -17.08054893949881858 ) ) ;
#18786 = ORIENTED_EDGE ( 'NONE', *, *, #28523, .T. ) ;
#18787 = DIRECTION ( 'NONE',  ( -0.000000000000000000, -0.9284778069183721172, -0.3713878862591650232 ) ) ;
#18788 = CARTESIAN_POINT ( 'NONE',  ( 109.2294421295247844, -8.865838614420134434, -9.247624522711900497 ) ) ;
#18789 = CARTESIAN_POINT ( 'NONE',  ( 119.9438214775786378, -2.084020599724406786, -8.691656652584148546 ) ) ;
#18790 = EDGE_CURVE ( 'NONE', #24351, #21469, #32287, .T. ) ;
#18791 = CARTESIAN_POINT ( 'NONE',  ( 112.3578015045248861, -6.936859964151250502, -18.39754474579286025 ) ) ;
#18792 = CARTESIAN_POINT ( 'NONE',  ( 106.8710046295248759, -4.863998795839590272, -7.631215200338315796 ) ) ;
#18793 = CARTESIAN_POINT ( 'NONE',  ( 114.0442481442453300, -7.643976991954077427, -18.09477374809248928 ) ) ;
#18794 = CARTESIAN_POINT ( 'NONE',  ( 54.86886719809545809, -45.79521720516596872, -17.39321520033831447 ) ) ;
#18795 = CARTESIAN_POINT ( 'NONE',  ( 112.0588148109119828, -9.859900752359374465, -12.68260735090039404 ) ) ;
#18796 = CARTESIAN_POINT ( 'NONE',  ( 118.1285681442453068, -7.893985811506177619, -18.51759400769804742 ) ) ;
#18797 = EDGE_LOOP ( 'NONE', ( #7336, #34147, #8471, #10744 ) ) ;
#18798 = CARTESIAN_POINT ( 'NONE',  ( 119.6601881442453106, -1.833838273342659253, -17.42832698103878286 ) ) ;
#18799 = CARTESIAN_POINT ( 'NONE',  ( 115.0653281442453277, -6.344957434206662583, -7.627207830600332805 ) ) ;
#18800 = CARTESIAN_POINT ( 'NONE',  ( 122.7801548109119665, -3.383040157471821630, -19.15922257007629170 ) ) ;
#18801 = CARTESIAN_POINT ( 'NONE',  ( 121.0216281442452981, -7.894159318335828068, -9.358103419637847864 ) ) ;
#18802 = EDGE_LOOP ( 'NONE', ( #39861, #1746, #14260, #36054 ) ) ;
#18803 = LINE ( 'NONE', #16748, #38348 ) ;
#18804 = CARTESIAN_POINT ( 'NONE',  ( 122.0994348109119443, 0.9020085738987339008, -11.91225656197089222 ) ) ;
#18805 = CARTESIAN_POINT ( 'NONE',  ( 112.4559014775786778, -0.1624402480850797581, -16.17319339645315424 ) ) ;
#18806 = FACE_OUTER_BOUND ( 'NONE', #44789, .T. ) ;
#18807 = CARTESIAN_POINT ( 'NONE',  ( 127.7184548109119788, -3.484218720211406772, -13.98160872758045947 ) ) ;
#18808 = CARTESIAN_POINT ( 'NONE',  ( 114.7192077545248594, -2.791137627527939813, -18.39754474579286025 ) ) ;
#18809 = CARTESIAN_POINT ( 'NONE',  ( 113.7414098793805408, -2.191907684172563986, -18.20049396185734025 ) ) ;
#18810 = LINE ( 'NONE', #28079, #28806 ) ;
#18811 = CARTESIAN_POINT ( 'NONE',  ( 116.7671281442453335, -7.643976991954077427, -18.09477374809248928 ) ) ;
#18812 = CARTESIAN_POINT ( 'NONE',  ( 126.0135748109119902, -8.166667518702819706, -8.995218007635861213 ) ) ;
#18813 = CARTESIAN_POINT ( 'NONE',  ( 95.28169473643895060, -22.43346506512310512, -11.92178932409649228 ) ) ;
#18814 = DIRECTION ( 'NONE',  ( -0.1352586133457952255, -0.9908103287288504424, 0.000000000000000000 ) ) ;
#18815 = CARTESIAN_POINT ( 'NONE',  ( 111.9410827545248708, -6.936859964151250502, -8.388885654883777576 ) ) ;
#18816 = CARTESIAN_POINT ( 'NONE',  ( 115.1220548109119761, -1.833838273342658809, -17.42832698103878286 ) ) ;
#18817 = DIRECTION ( 'NONE',  ( 0.000000000000000000, -0.9242245927363027524, -0.3818493186865929423 ) ) ;
#18818 = CARTESIAN_POINT ( 'NONE',  ( -1.769543856513131397, -6.815240831730628557, -18.52879468264121243 ) ) ;
#18820 = CARTESIAN_POINT ( 'NONE',  ( 117.8449348109119938, -8.166667518702817929, -8.995218007635861213 ) ) ;
#18819 = CARTESIAN_POINT ( 'NONE',  ( 60.37068618338318515, -13.41750073646542241, -7.433261549074098973 ) ) ;
#18821 = CARTESIAN_POINT ( 'NONE',  ( 123.2906948109119867, -1.833838273342659697, -17.42832698103878286 ) ) ;
#18822 = EDGE_LOOP ( 'NONE', ( #18296, #11494 ) ) ;
#18823 = DIRECTION ( 'NONE',  ( -0.1957579692570466934, -0.9088796992199469349, 0.3682614693641134140 ) ) ;
#18824 = CARTESIAN_POINT ( 'NONE',  ( 126.0703014775786102, -9.988377603198980381, -10.36322818467138518 ) ) ;
#18825 = CARTESIAN_POINT ( 'NONE',  ( 108.1906140045248037, 0.1403307496149616695, -15.46607636864997204 ) ) ;
#18826 = CARTESIAN_POINT ( 'NONE',  ( 121.0783548109119749, -9.565557343593413364, -10.61323700422348004 ) ) ;
#18827 = CARTESIAN_POINT ( 'NONE',  ( 123.4608748109119745, 0.4262465694468514643, -12.03445270309931736 ) ) ;
#18828 = CARTESIAN_POINT ( 'NONE',  ( 116.5969481442453031, -9.859900752359374465, -12.68260735090039404 ) ) ;
#18829 = CARTESIAN_POINT ( 'NONE',  ( 119.6419022310133471, -1.244021962887374544, -16.96476564598603076 ) ) ;
#18830 = CARTESIAN_POINT ( 'NONE',  ( 109.5102233795247884, -8.938348069036489818, -17.46756447353520159 ) ) ;
#18831 = CARTESIAN_POINT ( 'NONE',  ( 122.5532481442453019, 0.4262465694468514643, -12.03445270309931736 ) ) ;
#18832 = CARTESIAN_POINT ( 'NONE',  ( 125.1626748109119802, -0.1624402480850797581, -16.17319339645315424 ) ) ;
#18833 = CARTESIAN_POINT ( 'NONE',  ( 72.54180985774836188, -51.37213739997068984, -33.02251202313252065 ) ) ;
#18834 = LINE ( 'NONE', #4696, #41583 ) ;
#18835 = CARTESIAN_POINT ( 'NONE',  ( 119.8129079359119942, -4.360204210389833968, -8.000047426360245240 ) ) ;
#18836 = CARTESIAN_POINT ( 'NONE',  ( 106.5931921295248372, -9.868328341294093420, -13.39321520033831447 ) ) ;
#18837 = DIRECTION ( 'NONE',  ( 0.000000000000000000, -0.3818493186865936084, 0.9242245927363024194 ) ) ;
#18838 = CARTESIAN_POINT ( 'NONE',  ( 82.71771818927497577, -31.37104225293308701, -22.09381113811972597 ) ) ;
#18839 = CARTESIAN_POINT ( 'NONE',  ( 119.6601881442453106, -8.166667518702819706, -8.995218007635861213 ) ) ;
#18840 = CARTESIAN_POINT ( 'NONE',  ( 116.7104014775786425, -0.4660016031367893996, -10.09054647747474043 ) ) ;
#18841 = DIRECTION ( 'NONE',  ( -0.000000000000000000, -0.9284778069183720062, -0.3713878862591650232 ) ) ;
#18842 =( BOUNDED_CURVE ( )  B_SPLINE_CURVE ( 2, ( #21194, #28719, #14577, #42625, #11387, #32784, #15706, #18677, #36216, #8639, #22539, #26418, #1335 ),
 .UNSPECIFIED., .F., .F. ) 
 B_SPLINE_CURVE_WITH_KNOTS ( ( 3, 2, 2, 2, 2, 2, 3 ),
 ( 0.2742732506792635028, 0.3750000000000000000, 0.5000000000000000000, 0.6250000000000000000, 0.7500000000000000000, 0.8750000000000000000, 0.9969031111431658765 ),
 .UNSPECIFIED. ) 
 CURVE ( )  GEOMETRIC_REPRESENTATION_ITEM ( )  RATIONAL_B_SPLINE_CURVE ( ( 0.9761776733140110629, 0.9386610620246970127, 1.000000000000000000, 0.9238795325112869605, 1.000000000000000000, 0.9238795325112869605, 1.000000000000000000, 0.9238795325112869605, 1.000000000000000000, 0.9238795325112869605, 1.000000000000000000, 0.9257654255316289937, 0.9963216603765929769 ) ) 
 REPRESENTATION_ITEM ( '' )  );
#18843 = CARTESIAN_POINT ( 'NONE',  ( 113.9307948109119906, 0.9020085738987339008, -11.91225656197089222 ) ) ;
#18844 = LINE ( 'NONE', #43018, #33744 ) ;
#18845 = EDGE_LOOP ( 'NONE', ( #30530, #3, #25991, #13324 ) ) ;
#18846 = CARTESIAN_POINT ( 'NONE',  ( 112.6609831777918913, -0.01829820670813664396, -14.64321520033831447 ) ) ;
#18847 = CARTESIAN_POINT ( 'NONE',  ( 115.3489614775786407, -9.261995988541697145, -16.69588392320189030 ) ) ;
#18848 = CARTESIAN_POINT ( 'NONE',  ( 125.5030348109119558, -6.222761293078241884, -8.102969835052219238 ) ) ;
#18849 =( NAMED_UNIT ( * ) SI_UNIT ( $, .STERADIAN. ) SOLID_ANGLE_UNIT ( ) );
#18850 = CARTESIAN_POINT ( 'NONE',  ( 112.6828081442453282, -2.084020599724406786, -8.691656652584148546 ) ) ;
#18851 = CARTESIAN_POINT ( 'NONE',  ( 125.6164881442453094, 0.2603800115204892296, -16.42320221600525088 ) ) ;
#18852 = CARTESIAN_POINT ( 'NONE',  ( 115.2053796295247849, -4.863998795839590272, -19.15521520033831493 ) ) ;
#18853 = CIRCLE ( 'NONE', #34873, 2.999999999999999556 ) ;
#18854 = CARTESIAN_POINT ( 'NONE',  ( 121.4754414775786131, -1.833838273342659697, -17.42832698103878286 ) ) ;
#18855 = CARTESIAN_POINT ( 'NONE',  ( 110.4825671295247815, -10.62599879583958540, -13.39321520033834290 ) ) ;
#18856 = CARTESIAN_POINT ( 'NONE',  ( 123.6794958213048261, -6.000051279993413367, -18.26434597752674094 ) ) ;
#18857 = ORIENTED_EDGE ( 'NONE', *, *, #40402, .T. ) ;
#18858 = CARTESIAN_POINT ( 'NONE',  ( 119.4656423109119743, -0.4387604401700512802, -15.73000352943951619 ) ) ;
#18859 = CARTESIAN_POINT ( 'NONE',  ( 120.7379948109119709, -10.63000616557722466, -14.87417383870573495 ) ) ;
#18860 = VERTEX_POINT ( 'NONE', #39247 ) ;
#18861 = CARTESIAN_POINT ( 'NONE',  ( 125.0836727849689254, -3.941856523015305314, -18.57470496855022901 ) ) ;
#18862 = CARTESIAN_POINT ( 'NONE',  ( -13.32377113153209436, -5.100909530930224811, -7.393215200338312698 ) ) ;
#18863 = CARTESIAN_POINT ( 'NONE',  ( 2.384484203314607420, -10.01861149699890063, -19.39321520033831447 ) ) ;
#18864 = CARTESIAN_POINT ( 'NONE',  ( 118.6958348109119754, -3.505236298600246325, -18.68346056562440793 ) ) ;
#18865 = CARTESIAN_POINT ( 'NONE',  ( 67.71887983560293378, -0.3398796721086269068, -16.39321520033832158 ) ) ;
#18866 = CARTESIAN_POINT ( 'NONE',  ( 124.5295211713731049, -9.813149682921396888, -12.67736657363807851 ) ) ;
#18867 = B_SPLINE_CURVE_WITH_KNOTS ( 'NONE', 3,
 ( #44583, #23608, #17212, #32162, #931, #31934, #30886, #700, #14620, #27251 ),
 .UNSPECIFIED., .F., .F.,
 ( 4, 3, 3, 4 ),
 ( 0.000000000000000000, 0.0002476487219222849707, 0.0004952974148303769834, 0.0009534114850261750764 ),
 .UNSPECIFIED. ) ;
#18868 = CARTESIAN_POINT ( 'NONE',  ( 121.8158014775786171, -4.153390946401325223, -8.397313243818185668 ) ) ;
#18869 = ADVANCED_FACE ( 'NONE', ( #4809, #21475 ), #32398, .F. ) ;
#18870 = CARTESIAN_POINT ( 'NONE',  ( 121.5321681442453041, -9.988377603198957289, -10.36322818467135498 ) ) ;
#18871 = CARTESIAN_POINT ( 'NONE',  ( 135.4265380376270684, -4.105408494840631306, -19.34504733371668195 ) ) ;
#18872 = CARTESIAN_POINT ( 'NONE',  ( 125.3390168672558218, -11.72568323628656906, -15.16441118647451169 ) ) ;
#18873 = CARTESIAN_POINT ( 'NONE',  ( 119.3198281442452924, -9.859900752359374465, -12.68260735090039404 ) ) ;
#18874 = CARTESIAN_POINT ( 'NONE',  ( 124.7088614775786226, -9.565557343593413364, -10.61323700422348004 ) ) ;
#18875 = CARTESIAN_POINT ( 'NONE',  ( 118.8092881442453290, -9.988377603198976828, -10.36322818467138340 ) ) ;
#18876 = CARTESIAN_POINT ( 'NONE',  ( 116.5402214775786405, 0.2603800115204892296, -16.42320221600525088 ) ) ;
#18877 = CARTESIAN_POINT ( 'NONE',  ( 115.0664733795247798, -1.325403438956436419, -9.854619843455211026 ) ) ;
#18878 = CARTESIAN_POINT ( 'NONE',  ( 124.3685014775786328, 0.4262465694468514643, -12.03445270309931736 ) ) ;
#18879 = ORIENTED_EDGE ( 'NONE', *, *, #44579, .F. ) ;
#18880 = CARTESIAN_POINT ( 'NONE',  ( 119.2063748109119814, -1.561330072975668504, -17.79121239304076951 ) ) ;
#18881 = CARTESIAN_POINT ( 'NONE',  ( 116.4555358795247884, -0.7896495226426338832, -17.46756447353520159 ) ) ;
#18882 = CARTESIAN_POINT ( 'NONE',  ( 107.0099108795247815, -1.325403438956436419, -16.93181055722141792 ) ) ;
#18883 = CARTESIAN_POINT ( 'NONE',  ( 63.69189222814998175, -40.21211973637273474, -4.893215200338314474 ) ) ;
#18884 = CARTESIAN_POINT ( 'NONE',  ( 113.1366214775786432, -7.643976991954077427, -18.09477374809248928 ) ) ;
#18885 = CIRCLE ( 'NONE', #39266, 1.499999999999998002 ) ;
#18886 = CARTESIAN_POINT ( 'NONE',  ( 120.7643014478796459, -9.877548923986811502, -16.68609415519376427 ) ) ;
#18887 = CARTESIAN_POINT ( 'NONE',  ( 125.2761281442453054, -10.63000616557722466, -14.87417383870573495 ) ) ;
#18888 = ORIENTED_EDGE ( 'NONE', *, *, #14610, .F. ) ;
#18889 = AXIS2_PLACEMENT_3D ( 'NONE', #14678, #7603, #38599 ) ;
#18890 = CARTESIAN_POINT ( 'NONE',  ( 125.7299414775786346, -10.15424416112533912, -14.75197769757731336 ) ) ;
#18891 = CARTESIAN_POINT ( 'NONE',  ( 94.20708369096698220, -25.14343533174585943, -14.10537061818067883 ) ) ;
#18892 = CARTESIAN_POINT ( 'NONE',  ( 123.7022829359119811, -4.283928203966213211, -7.183505701512925334 ) ) ;
#18893 = FACE_OUTER_BOUND ( 'NONE', #12105, .T. ) ;
#18894 = CARTESIAN_POINT ( 'NONE',  ( 105.6903015045248253, -6.936859964151250502, -18.39754474579286025 ) ) ;
#18895 = EDGE_CURVE ( 'NONE', #22022, #32220, #6821, .T. ) ;
#18896 = ORIENTED_EDGE ( 'NONE', *, *, #13074, .F. ) ;
#18897 = CARTESIAN_POINT ( 'NONE',  ( 113.0798948109119948, -0.4660016031367893996, -10.09054647747474043 ) ) ;
#18898 = CARTESIAN_POINT ( 'NONE',  ( 88.69221322696461129, -11.18906686396361749, -14.08003406886638764 ) ) ;
#18899 = CARTESIAN_POINT ( 'NONE',  ( 121.2485348109119769, -8.899110576539710493, -16.42337572283490132 ) ) ;
#18900 = CARTESIAN_POINT ( 'NONE',  ( 113.3635281442453504, -0.1624402480850797581, -16.17319339645315424 ) ) ;
#18901 = DIRECTION ( 'NONE',  ( 0.9970811988817434024, -0.07634843047859753151, 0.000000000000000000 ) ) ;
#18902 = CARTESIAN_POINT ( 'NONE',  ( 124.1415948109119540, -6.344957434206689229, -7.627207830600343463 ) ) ;
#18903 = EDGE_CURVE ( 'NONE', #9021, #36955, #37266, .T. ) ;
#18904 = CARTESIAN_POINT ( 'NONE',  ( 125.1059481442452750, -1.833838273342660141, -17.42832698103878286 ) ) ;
#18905 = ADVANCED_FACE ( 'NONE', ( #25573, #4134 ), #38556, .T. ) ;
#18906 = CYLINDRICAL_SURFACE ( 'NONE', #41656, 3.000000000000003997 ) ;
#18907 = CARTESIAN_POINT ( 'NONE',  ( 123.6877814775786533, -3.383040157471821630, -19.15922257007629170 ) ) ;
#18908 = CARTESIAN_POINT ( 'NONE',  ( 136.7741008876061244, -8.463785208514361003, -17.69369302188813364 ) ) ;
#18909 = ORIENTED_EDGE ( 'NONE', *, *, #20009, .F. ) ;
#18910 = CARTESIAN_POINT ( 'NONE',  ( 112.7962614775786676, -3.383040157471821630, -19.15922257007629170 ) ) ;
#18911 = CARTESIAN_POINT ( 'NONE',  ( 124.2550481442452792, -9.988377603198980381, -10.36322818467138518 ) ) ;
#18912 = EDGE_CURVE ( 'NONE', #42996, #2964, #38114, .T. ) ;
#18913 = CARTESIAN_POINT ( 'NONE',  ( 110.8298327545248299, -6.936859964151250502, -8.388885654883788234 ) ) ;
#18914 = CARTESIAN_POINT ( 'NONE',  ( 125.2194014775786286, 0.1319031606808879209, -14.10382304977623669 ) ) ;
#18915 = VERTEX_POINT ( 'NONE', #32623 ) ;
#18916 = CARTESIAN_POINT ( 'NONE',  ( 117.8449348109119938, -8.166667518702817929, -8.995218007635861213 ) ) ;
#18917 = AXIS2_PLACEMENT_3D ( 'NONE', #7101, #13732, #34673 ) ;
#18918 = CARTESIAN_POINT ( 'NONE',  ( 68.07789357685331311, -68.58957386525776201, -38.44539312525987640 ) ) ;
#18919 = CARTESIAN_POINT ( 'NONE',  ( 110.2047546295247855, -4.863998795839541422, -18.39754474579285315 ) ) ;
#18920 = EDGE_CURVE ( 'NONE', #11018, #9245, #31861, .T. ) ;
#18921 = CARTESIAN_POINT ( 'NONE',  ( 111.8319081442453182, -4.153390946401313677, -8.397313243818183892 ) ) ;
#18922 = ADVANCED_FACE ( 'NONE', ( #7332 ), #21251, .T. ) ;
#18923 = EDGE_CURVE ( 'NONE', #36064, #43343, #3911, .T. ) ;
#18924 = CARTESIAN_POINT ( 'NONE',  ( 136.7860375664303376, -5.353572327191975511, -7.813356190730346817 ) ) ;
#18925 = CARTESIAN_POINT ( 'NONE',  ( 115.7460481442453357, -10.15424416112533912, -14.75197769757731336 ) ) ;
#18926 = PLANE ( 'NONE',  #64 ) ;
#18927 = AXIS2_PLACEMENT_3D ( 'NONE', #12724, #33435, #32992 ) ;
#18928 = CARTESIAN_POINT ( 'NONE',  ( 124.9511461828809473, -3.739606423682455993, -20.93492623671060926 ) ) ;
#18929 = CARTESIAN_POINT ( 'NONE',  ( 125.9001214775786224, -4.089484607189486809, -7.948022111789456723 ) ) ;
#18930 = AXIS2_PLACEMENT_3D ( 'NONE', #5301, #4623, #12155 ) ;
#18931 = CARTESIAN_POINT ( 'NONE',  ( 125.7866681442452688, -8.899110576539710493, -16.42337572283490132 ) ) ;
#18932 = CARTESIAN_POINT ( 'NONE',  ( 116.6779416893911616, -8.401490633876564473, -17.04399421721747743 ) ) ;
#18933 = CARTESIAN_POINT ( 'NONE',  ( 124.1983214775786166, -1.833838273342659697, -17.42832698103878286 ) ) ;
#18934 = DIRECTION ( 'NONE',  ( 1.000000000000000000, 0.000000000000000000, -0.000000000000000000 ) ) ;
#18935 = CARTESIAN_POINT ( 'NONE',  ( 118.4122014775786340, 0.5811942927096110934, -14.16772938898807510 ) ) ;
#18936 = CARTESIAN_POINT ( 'NONE',  ( 121.4754414775786131, -8.166667518702819706, -8.995218007635861213 ) ) ;
#18937 = CARTESIAN_POINT ( 'NONE',  ( 114.6998541094426969, 0.3591747506842615789, -12.14321520033831625 ) ) ;
#18938 = CARTESIAN_POINT ( 'NONE',  ( 114.3719421295247827, 0.8980012041604618078, -13.39321520033831447 ) ) ;
#18939 = CARTESIAN_POINT ( 'NONE',  ( 110.8992858795247827, -8.402594152722688392, -9.854619843455216355 ) ) ;
#18940 = CARTESIAN_POINT ( 'NONE',  ( 110.3436608795247764, -1.325403438956436419, -16.93181055722141792 ) ) ;
#18941 = CARTESIAN_POINT ( 'NONE',  ( 126.4750299824207502, -9.821253635553782502, -12.07982667344025884 ) ) ;
#18942 = CARTESIAN_POINT ( 'NONE',  ( 115.8595014775786609, -1.834011780172310813, -8.268836392978581529 ) ) ;
#18943 = ORIENTED_EDGE ( 'NONE', *, *, #20045, .T. ) ;
#18944 = CARTESIAN_POINT ( 'NONE',  ( 106.6626452545248611, 0.8980012041604421569, -11.00651665394454071 ) ) ;
#18945 = DIRECTION ( 'NONE',  ( -1.000000000000000000, 0.000000000000000000, 0.000000000000000000 ) ) ;
#18946 = CARTESIAN_POINT ( 'NONE',  ( 126.0703014775786102, -9.988377603198980381, -10.36322818467138518 ) ) ;
#18947 = CARTESIAN_POINT ( 'NONE',  ( 109.2295909607760933, -0.1191545588266860467, -15.28045812891908284 ) ) ;
#18948 = CARTESIAN_POINT ( 'NONE',  ( 89.12784890491134604, -25.99489077589524300, -13.39321520033831625 ) ) ;
#18949 = CARTESIAN_POINT ( 'NONE',  ( 120.7947214775786193, -9.261995988541697145, -16.69588392320189030 ) ) ;
#18950 = CARTESIAN_POINT ( 'NONE',  ( 110.7603796295247918, -4.863998795839590272, -19.15521520033831493 ) ) ;
#18951 = DIRECTION ( 'NONE',  ( -0.7871354856660202071, 0.6167752151498580027, 0.002461946824133919541 ) ) ;
#18952 = VERTEX_POINT ( 'NONE', #497 ) ;
#18953 = CARTESIAN_POINT ( 'NONE',  ( 121.1350814775786233, -9.859900752359369136, -12.68260735090035318 ) ) ;
#18954 = CARTESIAN_POINT ( 'NONE',  ( 120.0005481442453146, -4.153390946401325223, -8.397313243818185668 ) ) ;
#18955 = CARTESIAN_POINT ( 'NONE',  ( 116.6536748109119941, 0.9020085738987339008, -11.91225656197089222 ) ) ;
#18956 = VECTOR ( 'NONE', #27321, 1000.000000000000114 ) ;
#18957 = CARTESIAN_POINT ( 'NONE',  ( 112.1155414775786454, 0.9020085738987339008, -11.91225656197089222 ) ) ;
#18958 = CYLINDRICAL_SURFACE ( 'NONE', #29294, 2.000000000000000000 ) ;
#18959 = CARTESIAN_POINT ( 'NONE',  ( 124.0281414775786146, -7.643976991954077427, -18.09477374809248928 ) ) ;
#18960 = CARTESIAN_POINT ( 'NONE',  ( 114.3278814775786429, 0.1319031606808879209, -14.10382304977623669 ) ) ;
#18961 = ORIENTED_EDGE ( 'NONE', *, *, #11674, .T. ) ;
#18962 = CARTESIAN_POINT ( 'NONE',  ( 122.7993923109119692, -0.4387604401700512802, -15.73000352943951619 ) ) ;
#18963 = CIRCLE ( 'NONE', #42246, 2.000000000000000444 ) ;
#18964 = CARTESIAN_POINT ( 'NONE',  ( 96.46827370896536991, -24.99618726903056753, -13.53781830588664903 ) ) ;
#18965 = CARTESIAN_POINT ( 'NONE',  ( 115.9162281442453093, -5.574606645277164318, -18.38911715685844683 ) ) ;
#18966 = ORIENTED_EDGE ( 'NONE', *, *, #6669, .T. ) ;
#18967 = AXIS2_PLACEMENT_3D ( 'NONE', #41986, #3454, #3004 ) ;
#18968 = CARTESIAN_POINT ( 'NONE',  ( 120.3685329359119862, -5.367793381288652910, -18.78638297431638904 ) ) ;
#18969 = CARTESIAN_POINT ( 'NONE',  ( 115.9729548109119861, -6.344957434206662583, -7.627207830600332805 ) ) ;
#18970 = CARTESIAN_POINT ( 'NONE',  ( 108.2600671295247992, 0.1403307496149613920, -13.39321520033831447 ) ) ;
#18971 = CARTESIAN_POINT ( 'NONE',  ( 113.2500748109119968, -3.505236298600246325, -18.68346056562440793 ) ) ;
#18972 = EDGE_CURVE ( 'NONE', #11934, #16272, #40025, .T. ) ;
#18973 = ORIENTED_EDGE ( 'NONE', *, *, #39430, .T. ) ;
#18974 = EDGE_LOOP ( 'NONE', ( #1991, #33150, #34587, #13389, #35032 ) ) ;
#18975 = CARTESIAN_POINT ( 'NONE',  ( 120.6812681442452941, 0.1319031606808879209, -14.10382304977623669 ) ) ;
#18976 = CARTESIAN_POINT ( 'NONE',  ( 118.0718414775786442, -0.8288870151387760510, -10.36305467784173118 ) ) ;
#18977 = ORIENTED_EDGE ( 'NONE', *, *, #24470, .F. ) ;
#18978 = DIRECTION ( 'NONE',  ( 0.8636456077245090457, -0.5040994586965586999, 0.000000000000000000 ) ) ;
#18979 = CARTESIAN_POINT ( 'NONE',  ( 62.68840920241336789, -64.78138427943380862, -45.84136708138180438 ) ) ;
#18980 = CARTESIAN_POINT ( 'NONE',  ( 107.7738952545248310, 0.8980012041604421569, -11.00651665394454071 ) ) ;
#18981 = AXIS2_PLACEMENT_3D ( 'NONE', #36084, #28143, #21742 ) ;
#18982 = CARTESIAN_POINT ( 'NONE',  ( 116.9373081442452929, -8.166667518702817929, -8.995218007635861213 ) ) ;
#18984 = CARTESIAN_POINT ( 'NONE',  ( 115.6893214775786447, -9.859900752359374465, -12.68260735090039404 ) ) ;
#18983 = CARTESIAN_POINT ( 'NONE',  ( 113.7606148109119886, -1.561330072975668060, -17.79121239304076596 ) ) ;
#18985 = EDGE_CURVE ( 'NONE', #38956, #23418, #14007, .T. ) ;
#18986 = CARTESIAN_POINT ( 'NONE',  ( 119.7169148109119874, -0.1624402480850797581, -16.17319339645315424 ) ) ;
#18987 = CARTESIAN_POINT ( 'NONE',  ( 35.90261398037149121, 14.17005867477686820, -19.39321520033831447 ) ) ;
#18988 = ORIENTED_EDGE ( 'NONE', *, *, #22220, .T. ) ;
#18989 = CARTESIAN_POINT ( 'NONE',  ( 120.6245414775786458, -0.1624402480850797581, -16.17319339645315424 ) ) ;
#18990 = CARTESIAN_POINT ( 'NONE',  ( 125.6732148109119862, -9.859900752359378018, -12.68260735090039759 ) ) ;
#18991 = CARTESIAN_POINT ( 'NONE',  ( 111.2465515045248168, -2.477300249445798297, -7.631215200338321125 ) ) ;
#18992 = CARTESIAN_POINT ( 'NONE',  ( 115.8304577545247582, -2.791137627527939813, -18.39754474579286025 ) ) ;
#18993 = CARTESIAN_POINT ( 'NONE',  ( 110.4131140045248287, -10.62599879583958717, -11.00651665394454604 ) ) ;
#18994 = CARTESIAN_POINT ( 'NONE',  ( 120.2841814775786276, 0.9020085738987339008, -11.91225656197089222 ) ) ;
#18995 = ORIENTED_EDGE ( 'NONE', *, *, #44338, .T. ) ;
#18996 = CIRCLE ( 'NONE', #38636, 1.200000000000000178 ) ;
#18997 = CARTESIAN_POINT ( 'NONE',  ( 120.8514481442452961, -7.893985811506177619, -18.51759400769804742 ) ) ;
#18998 = DIRECTION ( 'NONE',  ( 7.002829358989538952E-15, -0.3818493186865928868, 0.9242245927363027524 ) ) ;
#18999 = CARTESIAN_POINT ( 'NONE',  ( 106.5237390045248418, 0.8980012041604421569, -15.77991374673208469 ) ) ;
#19000 = CARTESIAN_POINT ( 'NONE',  ( 118.0718414775786300, -9.261995988541697145, -16.69588392320189030 ) ) ;
#19001 = CARTESIAN_POINT ( 'NONE',  ( 118.4122014775786340, 0.5811942927096110934, -14.16772938898807510 ) ) ;
#19002 = DIRECTION ( 'NONE',  ( -0.3127730236694430399, 0.9498278979187092519, 0.000000000000000000 ) ) ;
#19003 = CARTESIAN_POINT ( 'NONE',  ( 116.6195842771102917, -11.86478987849519662, -6.418176294668409554 ) ) ;
#19004 = ORIENTED_EDGE ( 'NONE', *, *, #23925, .T. ) ;
#19005 = DIRECTION ( 'NONE',  ( 0.000000000000000000, 0.000000000000000000, -1.000000000000000000 ) ) ;
#19006 = CARTESIAN_POINT ( 'NONE',  ( 109.2296195588419749, -9.603284990525381204, -16.08186249415100733 ) ) ;
#19007 = CARTESIAN_POINT ( 'NONE',  ( 120.5110881442453206, -3.505236298600246325, -18.68346056562440793 ) ) ;
#19008 = CARTESIAN_POINT ( 'NONE',  ( 112.2188952545247531, -9.868328341294098749, -15.46607636864997204 ) ) ;
#19009 = CARTESIAN_POINT ( 'NONE',  ( 115.5526452545247622, -9.868328341294098749, -15.46607636864997204 ) ) ;
#19010 = CARTESIAN_POINT ( 'NONE',  ( 113.4769814775786330, 0.4262465694468514643, -12.03445270309931736 ) ) ;
#19011 = DIRECTION ( 'NONE',  ( -0.9609149988134837450, 0.1028163501681639419, -0.2570431154366518145 ) ) ;
#19012 = CARTESIAN_POINT ( 'NONE',  ( 71.36090047007586179, -25.24828423334623650, -5.221195830130035631 ) ) ;
#19013 = CARTESIAN_POINT ( 'NONE',  ( 111.4915481442453142, -1.833838273342658365, -17.42832698103878286 ) ) ;
#19014 = CARTESIAN_POINT ( 'NONE',  ( 119.6034614775786196, -6.344957434206665248, -7.627207830600338134 ) ) ;
#19015 = ORIENTED_EDGE ( 'NONE', *, *, #41411, .T. ) ;
#19016 = CARTESIAN_POINT ( 'NONE',  ( 119.1496481442453046, -6.222761293078241884, -8.102969835052219238 ) ) ;
#19017 = CARTESIAN_POINT ( 'NONE',  ( 115.2355081442453155, -10.30919188438810075, -12.61870101168855918 ) ) ;
#19018 = VECTOR ( 'NONE', #7720, 1000.000000000000000 ) ;
#19019 = CARTESIAN_POINT ( 'NONE',  ( 120.2841814775786276, 0.9020085738987339008, -11.91225656197089222 ) ) ;
#19020 = CARTESIAN_POINT ( 'NONE',  ( 121.5888948109119809, 0.1319031606808879209, -14.10382304977623669 ) ) ;
#19021 = ORIENTED_EDGE ( 'NONE', *, *, #21715, .F. ) ;
#19022 = CARTESIAN_POINT ( 'NONE',  ( 124.5954081442453116, -6.222761293078241884, -8.102969835052219238 ) ) ;
#19023 = EDGE_CURVE ( 'NONE', #39913, #6217, #17738, .T. ) ;
#19024 = AXIS2_PLACEMENT_3D ( 'NONE', #6327, #41227, #31164 ) ;
#19025 = CARTESIAN_POINT ( 'NONE',  ( 120.0572748109119772, -3.383040157471821630, -19.15922257007629170 ) ) ;
#19026 = CARTESIAN_POINT ( 'NONE',  ( 112.6828081442453282, -2.084020599724406786, -8.691656652584148546 ) ) ;
#19027 = CARTESIAN_POINT ( 'NONE',  ( 120.6245414775786458, -9.988377603198976828, -10.36322818467138340 ) ) ;
#19028 = CARTESIAN_POINT ( 'NONE',  ( 105.7597546295248350, -4.863998795839590272, -7.631215200338315796 ) ) ;
#19029 = CARTESIAN_POINT ( 'NONE',  ( 120.2990798109119766, -7.200787124940443817, -17.81845355600750835 ) ) ;
#19030 = CARTESIAN_POINT ( 'NONE',  ( 118.8886742554890787, -2.372251574601201174, -17.96033910819751611 ) ) ;
#19031 = CARTESIAN_POINT ( 'NONE',  ( 114.0941296295247867, -4.863998795839590272, -8.388885654883775800 ) ) ;
#19032 = EDGE_CURVE ( 'NONE', #19992, #18672, #35205, .T. ) ;
#19033 = FACE_OUTER_BOUND ( 'NONE', #20795, .T. ) ;
#19034 = DIRECTION ( 'NONE',  ( 0.6383198453882299450, 0.7697712484781087383, -9.200178928217186715E-17 ) ) ;
#19035 = CARTESIAN_POINT ( 'NONE',  ( 119.1496481442453046, -6.222761293078241884, -8.102969835052219238 ) ) ;
#19036 = CARTESIAN_POINT ( 'NONE',  ( 124.3685014775786328, -10.63000616557722466, -14.87417383870573495 ) ) ;
#19037 = CARTESIAN_POINT ( 'NONE',  ( 111.9884129883171084, -8.997528177137620986, -16.20962724730194537 ) ) ;
#19038 = ORIENTED_EDGE ( 'NONE', *, *, #20015, .T. ) ;
#19039 = CARTESIAN_POINT ( 'NONE',  ( 112.1243801106810167, -8.918668529216430940, -16.32041580884654053 ) ) ;
#19040 = CARTESIAN_POINT ( 'NONE',  ( 109.5102233795247884, -1.325403438956436419, -9.854619843455211026 ) ) ;
#19041 = CARTESIAN_POINT ( 'NONE',  ( 116.1998614775786507, 0.4262465694468514643, -12.03445270309931736 ) ) ;
#19042 = CARTESIAN_POINT ( 'NONE',  ( 113.4036376481213892, -2.395992375830784837, -17.92872468182854107 ) ) ;
#19044 = AXIS2_PLACEMENT_3D ( 'NONE', #16532, #34721, #30879 ) ;
#19043 = DIRECTION ( 'NONE',  ( -1.000000000000000000, 0.000000000000000000, 0.000000000000000000 ) ) ;
#19045 = CARTESIAN_POINT ( 'NONE',  ( -2.109783507832979854, -6.917548591251819090, -19.00710507435085361 ) ) ;
#19047 = CARTESIAN_POINT ( 'NONE',  ( 122.3263414775786373, -6.344957434206665248, -7.627207830600338134 ) ) ;
#19046 = CARTESIAN_POINT ( 'NONE',  ( 63.70438564670760684, -13.53232477329181727, -8.402906900370389565 ) ) ;
#19048 = CARTESIAN_POINT ( 'NONE',  ( 123.1205148109119563, -7.643976991954077427, -18.09477374809248928 ) ) ;
#19049 = EDGE_LOOP ( 'NONE', ( #24151, #40916, #27833, #3461, #12789 ) ) ;
#19050 = CARTESIAN_POINT ( 'NONE',  ( 114.8834831777918879, -0.01829820670803256055, -14.64321520033831447 ) ) ;
#19051 = DIRECTION ( 'NONE',  ( -0.9908103287288504424, 0.1352586133457952533, 0.000000000000000000 ) ) ;
#19052 = CARTESIAN_POINT ( 'NONE',  ( 107.8433483795247838, -8.402594152722688392, -16.93181055722141792 ) ) ;
#19053 = CARTESIAN_POINT ( 'NONE',  ( 123.3474214775786209, -0.1624402480850797581, -16.17319339645315424 ) ) ;
#19054 = CARTESIAN_POINT ( 'NONE',  ( 121.2485348109119769, -8.899110576539710493, -16.42337572283490132 ) ) ;
#19055 = CARTESIAN_POINT ( 'NONE',  ( 116.3700414775786527, -4.153390946401321671, -8.397313243818183892 ) ) ;
#19056 = DIRECTION ( 'NONE',  ( -0.000000000000000000, -0.9284778069183720062, -0.3713878862591650232 ) ) ;
#19057 = CARTESIAN_POINT ( 'NONE',  ( 106.7320983795247855, -0.7896495226426338832, -9.318865927141430916 ) ) ;
#19058 = CONICAL_SURFACE ( 'NONE', #43810, 2.000000000000000444, 0.9599310885968830309 ) ;
#19059 = DIRECTION ( 'NONE',  ( 0.9609149988134843001, -0.1028163501681632064, 0.2570431154366505933 ) ) ;
#19060 = CARTESIAN_POINT ( 'NONE',  ( 71.09163384711422395, -63.88803250098678888, -42.12154107070359288 ) ) ;
#19061 = DIRECTION ( 'NONE',  ( -1.000000000000000000, 0.000000000000000000, 0.000000000000000000 ) ) ;
#19062 = EDGE_CURVE ( 'NONE', #6756, #17138, #4699, .T. ) ;
#19063 = CARTESIAN_POINT ( 'NONE',  ( 112.7050671295247923, -10.62599879583958540, -13.39321520033831447 ) ) ;
#19064 = CARTESIAN_POINT ( 'NONE',  ( -13.36027627234077109, -3.983708254697501783, -18.97278025920458688 ) ) ;
#19065 = CARTESIAN_POINT ( 'NONE',  ( 82.45341866970989031, -31.73112455768813689, -22.62568415223593377 ) ) ;
#19066 = CARTESIAN_POINT ( 'NONE',  ( 122.7234281442452755, -5.638512984488999180, -18.83840828888717311 ) ) ;
#19067 = CARTESIAN_POINT ( 'NONE',  ( 118.5823814775786360, -1.834011780172310813, -8.268836392978581529 ) ) ;
#19068 = CARTESIAN_POINT ( 'NONE',  ( 106.5237390045248418, 0.8980012041604421569, -15.77991374673208469 ) ) ;
#19069 = CARTESIAN_POINT ( 'NONE',  ( 117.5613014775786525, 0.9020085738987339008, -11.91225656197089222 ) ) ;
#19070 = LINE ( 'NONE', #8807, #4616 ) ;
#19071 = ORIENTED_EDGE ( 'NONE', *, *, #28346, .T. ) ;
#19072 = CARTESIAN_POINT ( 'NONE',  ( 112.6135934012278881, 0.04929351793716424401, -14.64321520033828961 ) ) ;
#19073 = CARTESIAN_POINT ( 'NONE',  ( 123.2906948109119867, -8.166667518702819706, -8.995218007635861213 ) ) ;
#19074 = CARTESIAN_POINT ( 'NONE',  ( 120.6245414775786458, -9.988377603198976828, -10.36322818467138340 ) ) ;
#19075 = CARTESIAN_POINT ( 'NONE',  ( 125.3328548109119964, -0.8288870151387760510, -10.36305467784173118 ) ) ;
#19076 = CARTESIAN_POINT ( 'NONE',  ( 0.000000000000000000, 0.000000000000000000, 0.000000000000000000 ) ) ;
#19077 = CARTESIAN_POINT ( 'NONE',  ( 112.4559014775786778, -0.1624402480850797581, -16.17319339645315424 ) ) ;
#19078 = CARTESIAN_POINT ( 'NONE',  ( 112.0588148109119828, -9.859900752359374465, -12.68260735090039404 ) ) ;
#19079 = CARTESIAN_POINT ( 'NONE',  ( 110.3436608795247764, -8.938348069036489818, -9.318865927141430916 ) ) ;
#19080 = CIRCLE ( 'NONE', #8864, 20.00000000000000000 ) ;
#19081 = CARTESIAN_POINT ( 'NONE',  ( 119.9438214775786378, -2.084020599724406786, -8.691656652584148546 ) ) ;
#19082 = DIRECTION ( 'NONE',  ( 1.000000000000000000, 0.000000000000000000, 0.000000000000000000 ) ) ;
#19083 = CARTESIAN_POINT ( 'NONE',  ( 116.0388171295248014, -10.62599879583958540, -13.39321520033831447 ) ) ;
#19084 = ORIENTED_EDGE ( 'NONE', *, *, #3556, .F. ) ;
#19085 = CARTESIAN_POINT ( 'NONE',  ( 121.6881423109119709, -0.4387604401700512802, -15.73000352943951619 ) ) ;
#19086 = CARTESIAN_POINT ( 'NONE',  ( 123.6877814775786533, -3.383040157471821630, -19.15922257007629170 ) ) ;
#19087 = FACE_OUTER_BOUND ( 'NONE', #9236, .T. ) ;
#19088 = CARTESIAN_POINT ( 'NONE',  ( 64.74132663541574573, -2.651366324200352231, -8.204703752599687760 ) ) ;
#19089 = CARTESIAN_POINT ( 'NONE',  ( 115.0664888068194927, 0.1168444861213632779, -12.14321520033831625 ) ) ;
#19090 = EDGE_CURVE ( 'NONE', #42815, #44289, #23590, .T. ) ;
#19091 = CARTESIAN_POINT ( 'NONE',  ( 119.3198281442452924, -9.859900752359374465, -12.68260735090039404 ) ) ;
#19092 = CARTESIAN_POINT ( 'NONE',  ( 66.98520468312386811, -0.07767352569349476876, -16.39321520033831447 ) ) ;
#19093 = CARTESIAN_POINT ( 'NONE',  ( 124.5155214467870479, -9.741323495560987311, -12.29181226416380390 ) ) ;
#19094 = CARTESIAN_POINT ( 'NONE',  ( 123.5176014775786228, -0.8288870151387760510, -10.36305467784173118 ) ) ;
#19095 = DIRECTION ( 'NONE',  ( 0.000000000000000000, 0.9284778069183720062, 0.3713878862591650232 ) ) ;
#19096 = CARTESIAN_POINT ( 'NONE',  ( 125.2761281442453054, 0.4262465694468514643, -12.03445270309931736 ) ) ;
#19097 = CARTESIAN_POINT ( 'NONE',  ( 125.3096478272239835, -11.83614581139350541, -14.99072624410023202 ) ) ;
#19098 = CARTESIAN_POINT ( 'NONE',  ( 123.0637881442452937, -0.4660016031367893996, -10.09054647747474043 ) ) ;
#19099 = CARTESIAN_POINT ( 'NONE',  ( 119.0361948109119652, -2.084020599724406786, -8.691656652584148546 ) ) ;
#19100 = CARTESIAN_POINT ( 'NONE',  ( 121.5888948109119809, 0.1319031606808879209, -14.10382304977623669 ) ) ;
#19101 = ORIENTED_EDGE ( 'NONE', *, *, #13618, .F. ) ;
#19102 = CARTESIAN_POINT ( 'NONE',  ( 123.6310548109119765, -5.638512984488999180, -18.83840828888717311 ) ) ;
#19103 = CARTESIAN_POINT ( 'NONE',  ( 115.6893214775786447, 0.5811942927096154232, -14.16772938898807155 ) ) ;
#19104 = FACE_OUTER_BOUND ( 'NONE', #2501, .T. ) ;
#19105 = CARTESIAN_POINT ( 'NONE',  ( 113.3635281442453504, -9.988377603198976828, -10.36322818467138340 ) ) ;
#19106 =( BOUNDED_SURFACE ( )  B_SPLINE_SURFACE ( 3, 2, ( 
 ( #7955, #7728, #17551 ),
 ( #17772, #4532, #41952 ),
 ( #25295, #38500, #31667 ),
 ( #28493, #21640, #34846 ),
 ( #15029, #39422, #35761 ),
 ( #436, #4301, #21866 ),
 ( #32344, #32117, #35529 ),
 ( #3632, #42848, #42398 ),
 ( #10935, #1111, #11608 ),
 ( #28266, #11162, #31894 ),
 ( #42175, #25519, #31445 ),
 ( #38728, #38960, #214 ),
 ( #7500, #25067, #28044 ),
 ( #18223, #14127, #10716 ),
 ( #24617, #14804, #661 ),
 ( #28717, #24837, #21192 ) ),
 .UNSPECIFIED., .F., .F., .T. ) 
 B_SPLINE_SURFACE_WITH_KNOTS ( ( 4, 2, 2, 2, 2, 2, 2, 4 ),
 ( 3, 3 ),
 ( 0.000000000000000000, 0.001721917349777002610, 0.002582876024665504023, 0.003443834699554005219, 0.004304793374442506849, 0.005165752049331008046, 0.006026710724219509242, 0.006887669399108010439 ),
 ( 0.000000000000000000, 1.000000000000000000 ),
 .UNSPECIFIED. ) 
 GEOMETRIC_REPRESENTATION_ITEM ( )  RATIONAL_B_SPLINE_SURFACE ( (
 ( 1.000000000000000000, 0.7145271066604784727, 1.000000000000000000),
 ( 1.000000000000000000, 0.7222082868831993796, 1.000000000000000000),
 ( 1.000000000000000000, 0.7248468039590466594, 1.000000000000000000),
 ( 1.000000000000000000, 0.7198065179285114690, 1.000000000000000000),
 ( 1.000000000000000000, 0.7166470691620621114, 1.000000000000000000),
 ( 1.000000000000000000, 0.7075588989364935966, 1.000000000000000000),
 ( 1.000000000000000000, 0.7016239504775774183, 1.000000000000000000),
 ( 1.000000000000000000, 0.6870381831995848732, 1.000000000000000000),
 ( 1.000000000000000000, 0.6784604258937906307, 1.000000000000000000),
 ( 1.000000000000000000, 0.6592551312636351080, 1.000000000000000000),
 ( 1.000000000000000000, 0.6485902070625576554, 1.000000000000000000),
 ( 1.000000000000000000, 0.6253227720994979366, 1.000000000000000000),
 ( 1.000000000000000000, 0.6127475771026407170, 1.000000000000000000),
 ( 1.000000000000000000, 0.5864501210668879860, 1.000000000000000000),
 ( 1.000000000000000000, 0.5726586895731697879, 1.000000000000000000),
 ( 1.000000000000000000, 0.5583166281429867706, 1.000000000000000000) ) ) 
 REPRESENTATION_ITEM ( '' )  SURFACE ( )  );
#19107 = CARTESIAN_POINT ( 'NONE',  ( 123.0637881442452937, -8.899110576539710493, -16.42337572283490132 ) ) ;
#19108 = VERTEX_POINT ( 'NONE', #41018 ) ;
#19110 = CARTESIAN_POINT ( 'NONE',  ( 120.0572748109119772, -3.383040157471821630, -19.15922257007629170 ) ) ;
#19109 = VECTOR ( 'NONE', #25753, 1000.000000000000000 ) ;
#19111 = CARTESIAN_POINT ( 'NONE',  ( 114.9970202545248412, -10.62599879583958717, -15.77991374673208469 ) ) ;
#19112 = CARTESIAN_POINT ( 'NONE',  ( 109.3713171295247832, 0.1403307496149613920, -13.39321520033831447 ) ) ;
#19113 = DIRECTION ( 'NONE',  ( -1.000000000000000000, 0.000000000000000000, 0.000000000000000000 ) ) ;
#19114 = CARTESIAN_POINT ( 'NONE',  ( 114.6115148109119986, -6.222761293078241884, -8.102969835052219238 ) ) ;
#19115 = AXIS2_PLACEMENT_3D ( 'NONE', #5973, #36974, #26743 ) ;
#19116 = CARTESIAN_POINT ( 'NONE',  ( 64.69189222814998175, -41.76310523276723785, -4.893215200338314474 ) ) ;
#19117 = CARTESIAN_POINT ( 'NONE',  ( 116.1082702545247827, 0.1403307496149616695, -11.32035403202665336 ) ) ;
#19118 = ORIENTED_EDGE ( 'NONE', *, *, #11080, .T. ) ;
#19119 = CARTESIAN_POINT ( 'NONE',  ( 125.8433948109119456, -7.643976991954077427, -18.09477374809248928 ) ) ;
#19120 = CARTESIAN_POINT ( 'NONE',  ( 121.8965016859119856, -9.665098340737509730, -17.37397104707595474 ) ) ;
#19121 = CARTESIAN_POINT ( 'NONE',  ( 120.9936110609119737, -3.163656168406935087, -18.89861972220014508 ) ) ;
#19122 = AXIS2_PLACEMENT_3D ( 'NONE', #19076, #43482, #14760 ) ;
#19123 = DIRECTION ( 'NONE',  ( -0.000000000000000000, -0.9284778069183721172, -0.3713878862591650232 ) ) ;
#19124 = CARTESIAN_POINT ( 'NONE',  ( 109.5102233795247884, -1.325403438956436419, -9.854619843455211026 ) ) ;
#19125 = ORIENTED_EDGE ( 'NONE', *, *, #19698, .T. ) ;
#19126 = AXIS2_PLACEMENT_3D ( 'NONE', #22556, #29177, #4999 ) ;
#19127 = CARTESIAN_POINT ( 'NONE',  ( 115.6893214775786447, 0.5811942927096154232, -14.16772938898807155 ) ) ;
#19128 = CARTESIAN_POINT ( 'NONE',  ( 61.94466824697356344, -46.76115691171892053, -16.39321520033831447 ) ) ;
#19129 = CARTESIAN_POINT ( 'NONE',  ( 125.9001214775786224, -5.574606645277164318, -18.38911715685844683 ) ) ;
#19130 = CARTESIAN_POINT ( 'NONE',  ( 113.0231681442453180, -10.15424416112533912, -14.75197769757731336 ) ) ;
#19131 = CARTESIAN_POINT ( 'NONE',  ( 79.63740429864273551, 3.112009832785464614, -19.89321520033831447 ) ) ;
#19132 = CYLINDRICAL_SURFACE ( 'NONE', #12846, 20.00000000000000355 ) ;
#19133 = CARTESIAN_POINT ( 'NONE',  ( 113.9307948109119906, 0.9020085738987339008, -11.91225656197089222 ) ) ;
#19134 = EDGE_CURVE ( 'NONE', #11788, #26749, #43952, .T. ) ;
#19135 = CARTESIAN_POINT ( 'NONE',  ( 113.3995983795247895, -8.402594152722688392, -16.93181055722141792 ) ) ;
#19136 = CARTESIAN_POINT ( 'NONE',  ( 124.7655881442452852, 0.5811942927096110934, -14.16772938898807510 ) ) ;
#19137 = SURFACE_STYLE_USAGE ( .BOTH. , #2701 ) ;
#19138 = ORIENTED_EDGE ( 'NONE', *, *, #35998, .F. ) ;
#19139 = CARTESIAN_POINT ( 'NONE',  ( 115.4056881442453459, -7.893985811506177619, -18.51759400769804742 ) ) ;
#19140 = CARTESIAN_POINT ( 'NONE',  ( 124.8790414775786246, -0.4660016031367893996, -10.09054647747474043 ) ) ;
#19141 = DIRECTION ( 'NONE',  ( -0.9986099732815398866, -0.05270788615228313989, 0.000000000000000000 ) ) ;
#19142 = CARTESIAN_POINT ( 'NONE',  ( 112.5693548109119888, -10.63000616557722466, -14.87417383870573495 ) ) ;
#19143 = EDGE_LOOP ( 'NONE', ( #36097, #37751, #5601, #5482, #43808 ) ) ;
#19144 = CARTESIAN_POINT ( 'NONE',  ( 117.0507614775786465, -10.30919188438810075, -12.61870101168855918 ) ) ;
#19145 = DIRECTION ( 'NONE',  ( -1.000000000000000000, 0.000000000000000000, 0.000000000000000000 ) ) ;
#19146 = B_SPLINE_CURVE_WITH_KNOTS ( 'NONE', 3,
 ( #39878, #15035, #28946, #7736, #4307, #36220, #38967, #11169, #18898, #32789, #18229, #42854, #11613, #8643, #22543, #25524, #32573, #35535, #32123, #1340, #15254, #39195, #7961, #42630 ),
 .UNSPECIFIED., .F., .F.,
 ( 4, 2, 2, 1, 1, 2, 2, 2, 2, 2, 2, 2, 4 ),
 ( 0.000000000000000000, 0.1250000000000380806, 0.1875000000000567879, 0.2187500000000661415, 0.2343750000000627276, 0.2421875000000603961, 0.2500000000000580647, 0.3750000000000387468, 0.4375000000000208722, 0.4687500000000185962, 0.5000000000000163203, 0.7500000000000082157, 1.000000000000000000 ),
 .UNSPECIFIED. ) ;
#19147 = CARTESIAN_POINT ( 'NONE',  ( 116.0506660444391969, -1.267766418764730840, -16.93314635290706605 ) ) ;
#19148 = LINE ( 'NONE', #33031, #14937 ) ;
#19149 = CARTESIAN_POINT ( 'NONE',  ( 123.6535389976226469, -4.507869723015496710, -15.11657223165913599 ) ) ;
#19150 = CARTESIAN_POINT ( 'NONE',  ( 114.8951481442453115, -8.899110576539710493, -16.42337572283490132 ) ) ;
#19151 = ADVANCED_FACE ( 'NONE', ( #44428 ), #5778, .T. ) ;
#19152 = DIRECTION ( 'NONE',  ( 0.000000000000000000, -0.3818493186865927203, 0.9242245927363029745 ) ) ;
#19153 = AXIS2_PLACEMENT_3D ( 'NONE', #38637, #8102, #28852 ) ;
#19154 = CARTESIAN_POINT ( 'NONE',  ( 124.8979611532368494, -3.762709360267329828, -20.98360247027872916 ) ) ;
#19155 = CARTESIAN_POINT ( 'NONE',  ( 125.8433948109119456, -1.834011780172310813, -8.268836392978581529 ) ) ;
#19156 = CARTESIAN_POINT ( 'NONE',  ( 111.7184548109119788, -9.261995988541697145, -16.69588392320189030 ) ) ;
#19157 = CARTESIAN_POINT ( 'NONE',  ( 116.7153894074022418, -6.872978516340015886, -18.10395076569972517 ) ) ;
#19158 = CARTESIAN_POINT ( 'NONE',  ( 122.3830681442452857, -1.833838273342659697, -17.42832698103878286 ) ) ;
#19159 = DIRECTION ( 'NONE',  ( 0.000000000000000000, 0.3818493186865927203, -0.9242245927363029745 ) ) ;
#19160 = CARTESIAN_POINT ( 'NONE',  ( 121.8158014775786171, -5.638512984488999180, -18.83840828888717311 ) ) ;
#19161 = ADVANCED_FACE ( 'NONE', ( #21484 ), #508, .T. ) ;
#19162 = CARTESIAN_POINT ( 'NONE',  ( 121.4187148109119789, -6.344957434206665248, -7.627207830600338134 ) ) ;
#19163 = VERTEX_POINT ( 'NONE', #18517 ) ;
#19164 = CARTESIAN_POINT ( 'NONE',  ( 117.4103264091100840, -0.9924539043446216624, -17.29976612834909133 ) ) ;
#19165 = EDGE_CURVE ( 'NONE', #21938, #4879, #10462, .T. ) ;
#19166 = CARTESIAN_POINT ( 'NONE',  ( 112.4967077545247633, -7.250697342233347165, -7.631215200338321125 ) ) ;
#19167 = CARTESIAN_POINT ( 'NONE',  ( 111.1770983795247787, -8.402594152722688392, -16.93181055722141792 ) ) ;
#19168 = CARTESIAN_POINT ( 'NONE',  ( 109.1629577545248395, -2.791137627527939813, -18.39754474579286025 ) ) ;
#19169 = CARTESIAN_POINT ( 'NONE',  ( 86.09323753712084226, -25.99489077589524300, -13.39321520033831625 ) ) ;
#19170 = CARTESIAN_POINT ( 'NONE',  ( 113.9307948109119906, 0.9020085738987339008, -11.91225656197089222 ) ) ;
#19171 = ORIENTED_EDGE ( 'NONE', *, *, #25857, .F. ) ;
#19172 = CARTESIAN_POINT ( 'NONE',  ( 70.89562859596755118, -66.92613143246303764, -42.60403544796190545 ) ) ;
#19173 = FACE_OUTER_BOUND ( 'NONE', #36530, .T. ) ;
#19174 = CARTESIAN_POINT ( 'NONE',  ( 114.7816948109119863, -9.859900752359374465, -12.68260735090039404 ) ) ;
#19175 = CARTESIAN_POINT ( 'NONE',  ( 112.9903542721482950, -2.287189184988692059, -18.07361239780447448 ) ) ;
#19176 = CARTESIAN_POINT ( 'NONE',  ( 120.2274548109119934, 0.5811942927096110934, -14.16772938898807510 ) ) ;
#19177 = EDGE_CURVE ( 'NONE', #39489, #12241, #8695, .T. ) ;
#19178 = VECTOR ( 'NONE', #37584, 1000.000000000000000 ) ;
#19179 = CARTESIAN_POINT ( 'NONE',  ( 110.0658483795247804, -0.7896495226426338832, -9.318865927141430916 ) ) ;
#19180 = DIRECTION ( 'NONE',  ( -0.2768435750659266059, -0.3568721902840680249, 0.8921882507333128709 ) ) ;
#19181 = ORIENTED_EDGE ( 'NONE', *, *, #7719, .F. ) ;
#19182 = LINE ( 'NONE', #11896, #30356 ) ;
#19183 = CARTESIAN_POINT ( 'NONE',  ( 117.5613014775786525, -10.15424416112533912, -14.75197769757731336 ) ) ;
#19184 = CIRCLE ( 'NONE', #20663, 0.5000000000000004441 ) ;
#19185 = CARTESIAN_POINT ( 'NONE',  ( 115.6893214775786447, 0.5811942927096154232, -14.16772938898807155 ) ) ;
#19186 = CARTESIAN_POINT ( 'NONE',  ( 114.6115148109119986, -3.383040157471821630, -19.15922257007629170 ) ) ;
#19187 = EDGE_CURVE ( 'NONE', #24192, #12356, #43135, .T. ) ;
#19188 = CARTESIAN_POINT ( 'NONE',  ( 41.72636039845269096, -11.37347657059392070, -8.893215200338314474 ) ) ;
#19189 = CARTESIAN_POINT ( 'NONE',  ( 121.7590748109119687, -2.084020599724406786, -8.691656652584148546 ) ) ;
#19190 = CARTESIAN_POINT ( 'NONE',  ( 120.6812681442452941, 0.1319031606808879209, -14.10382304977623669 ) ) ;
#19191 = ORIENTED_EDGE ( 'NONE', *, *, #30164, .T. ) ;
#19192 = EDGE_CURVE ( 'NONE', #5970, #43660, #19866, .T. ) ;
#19193 = EDGE_CURVE ( 'NONE', #22775, #22330, #33754, .T. ) ;
#19194 = CARTESIAN_POINT ( 'NONE',  ( 123.9800954359119771, 0.5291689781388270175, -13.89700978578772705 ) ) ;
#19195 = CIRCLE ( 'NONE', #11190, 0.8509999999999994236 ) ;
#19196 = CARTESIAN_POINT ( 'NONE',  ( 113.5337081442453240, -9.261995988541697145, -16.69588392320189030 ) ) ;
#19197 = CARTESIAN_POINT ( 'NONE',  ( 118.6958348109119754, -3.505236298600246325, -18.68346056562440793 ) ) ;
#19198 = VERTEX_POINT ( 'NONE', #29671 ) ;
#19199 = CARTESIAN_POINT ( 'NONE',  ( 120.6463454359119822, 0.5291689781388270175, -13.89700978578772705 ) ) ;
#19200 = CARTESIAN_POINT ( 'NONE',  ( 114.6682414775786469, -1.561330072975668060, -17.79121239304076596 ) ) ;
#19201 = CARTESIAN_POINT ( 'NONE',  ( 108.3295202545248657, 0.1403307496149616695, -11.32035403202665336 ) ) ;
#19202 = CARTESIAN_POINT ( 'NONE',  ( 117.3911214775786505, -7.894159318335828068, -9.358103419637847864 ) ) ;
#19203 = VERTEX_POINT ( 'NONE', #26707 ) ;
#19204 = ORIENTED_EDGE ( 'NONE', *, *, #9220, .T. ) ;
#19205 = CARTESIAN_POINT ( 'NONE',  ( 121.9859814775786333, -9.565557343593413364, -10.61323700422348004 ) ) ;
#19206 = CARTESIAN_POINT ( 'NONE',  ( 119.6601881442453106, -1.833838273342659253, -17.42832698103878286 ) ) ;
#19207 = CARTESIAN_POINT ( 'NONE',  ( 78.69189222814998175, -69.76310523276724496, -0.9932152003383157846 ) ) ;
#19208 = ORIENTED_EDGE ( 'NONE', *, *, #1346, .F. ) ;
#19209 = CIRCLE ( 'NONE', #6083, 25.00000000000000355 ) ;
#19210 = DIRECTION ( 'NONE',  ( 1.000000000000000000, 0.000000000000000000, -0.000000000000000000 ) ) ;
#19211 = CARTESIAN_POINT ( 'NONE',  ( 61.70909112414298647, -66.14783507974324550, -42.93797631241571366 ) ) ;
#19212 = CARTESIAN_POINT ( 'NONE',  ( 107.0793640045248196, -10.62599879583958717, -11.00651665394454604 ) ) ;
#19213 = CARTESIAN_POINT ( 'NONE',  ( 114.7249681442453237, 0.2603800115204892296, -16.42320221600525088 ) ) ;
#19215 = CARTESIAN_POINT ( 'NONE',  ( 114.5547881442453217, -4.153390946401321671, -8.397313243818183892 ) ) ;
#19214 = CARTESIAN_POINT ( 'NONE',  ( 115.5758681442453053, -1.561330072975668060, -17.79121239304076951 ) ) ;
#19216 = CARTESIAN_POINT ( 'NONE',  ( 120.9649014775786355, -6.222761293078241884, -8.102969835052219238 ) ) ;
#19217 = CARTESIAN_POINT ( 'NONE',  ( 151.2860562277021472, -4.863998795839242995, -13.39321520033831447 ) ) ;
#19218 = ORIENTED_EDGE ( 'NONE', *, *, #35001, .F. ) ;
#19219 = CARTESIAN_POINT ( 'NONE',  ( 120.2841814775786276, -10.15424416112533912, -14.75197769757731336 ) ) ;
#19220 = EDGE_CURVE ( 'NONE', #23072, #31245, #26947, .T. ) ;
#19221 = CARTESIAN_POINT ( 'NONE',  ( 77.12856116249137983, -44.30583187727815186, -4.893215200338314474 ) ) ;
#19222 = CARTESIAN_POINT ( 'NONE',  ( 111.0381921295247878, 0.8980012041604618078, -13.39321520033831447 ) ) ;
#19223 = AXIS2_PLACEMENT_3D ( 'NONE', #16991, #37250, #33372 ) ;
#19224 = CARTESIAN_POINT ( 'NONE',  ( 113.7798197424434363, -0.9924539043446216624, -17.29976612834909133 ) ) ;
#19225 = CARTESIAN_POINT ( 'NONE',  ( 110.0658483795247804, -0.7896495226426338832, -9.318865927141430916 ) ) ;
#19226 = CARTESIAN_POINT ( 'NONE',  ( 118.0718414775786300, -9.261995988541697145, -16.69588392320189030 ) ) ;
#19227 = ORIENTED_EDGE ( 'NONE', *, *, #35637, .T. ) ;
#19228 = CARTESIAN_POINT ( 'NONE',  ( 121.9292548109119849, -1.561330072975668948, -17.79121239304076951 ) ) ;
#19229 = CARTESIAN_POINT ( 'NONE',  ( 62.74672096151675760, -37.51679531015581404, -5.130621874892657530 ) ) ;
#19230 = CARTESIAN_POINT ( 'NONE',  ( 106.4542858795248179, -0.7896495226426338832, -17.46756447353520159 ) ) ;
#19231 = CARTESIAN_POINT ( 'NONE',  ( 119.1496481442453046, -3.383040157471821630, -19.15922257007629170 ) ) ;
#19232 = CARTESIAN_POINT ( 'NONE',  ( 117.1642148109119859, -9.261995988541697145, -16.69588392320189030 ) ) ;
#19233 = CARTESIAN_POINT ( 'NONE',  ( 75.95778847736481509, -3.256761025687722189, -18.64321520033831803 ) ) ;
#19234 = CARTESIAN_POINT ( 'NONE',  ( 120.8933699480702586, -6.365377317481695663, -18.95617363400926081 ) ) ;
#19235 = VERTEX_POINT ( 'NONE', #33516 ) ;
#19236 = DIRECTION ( 'NONE',  ( 0.7697712484781088493, -0.6383198453882299450, 0.000000000000000000 ) ) ;
#19237 = CARTESIAN_POINT ( 'NONE',  ( 109.2292917470664833, -9.019994622780936666, -16.84346519180415669 ) ) ;
#19238 = CARTESIAN_POINT ( 'NONE',  ( 120.9649014775786355, -6.222761293078241884, -8.102969835052219238 ) ) ;
#19239 = CARTESIAN_POINT ( 'NONE',  ( 111.6632702545248605, 0.1403307496149616695, -11.32035403202665336 ) ) ;
#19240 = CARTESIAN_POINT ( 'NONE',  ( 109.7880358795247986, -8.402594152722688392, -9.854619843455216355 ) ) ;
#19241 = CARTESIAN_POINT ( 'NONE',  ( 116.5402214775786405, -9.565557343593413364, -10.61323700422348004 ) ) ;
#19242 = LINE ( 'NONE', #26081, #28473 ) ;
#19243 = CARTESIAN_POINT ( 'NONE',  ( 70.55229225240181279, -24.89194276641628889, -5.467054258871676176 ) ) ;
#19244 = CARTESIAN_POINT ( 'NONE',  ( 112.1722681442453222, -8.899110576539710493, -16.42337572283490132 ) ) ;
#19245 = CARTESIAN_POINT ( 'NONE',  ( 118.4122014775786340, 0.5811942927096110934, -14.16772938898807510 ) ) ;
#19246 = EDGE_LOOP ( 'NONE', ( #20854, #516, #44773, #30176 ) ) ;
#19247 = ADVANCED_FACE ( 'NONE', ( #43815 ), #18958, .F. ) ;
#19248 = CIRCLE ( 'NONE', #14849, 4.999999999999998224 ) ;
#19249 = CARTESIAN_POINT ( 'NONE',  ( 119.5467348109119712, -5.574606645277164318, -18.38911715685844683 ) ) ;
#19250 = CARTESIAN_POINT ( 'NONE',  ( 116.1998614775786507, -10.63000616557722466, -14.87417383870573495 ) ) ;
#19251 = EDGE_CURVE ( 'NONE', #27626, #25810, #9152, .T. ) ;
#19252 = CARTESIAN_POINT ( 'NONE',  ( 121.1918081442452859, 0.9020085738987339008, -11.91225656197089222 ) ) ;
#19253 = B_SPLINE_CURVE_WITH_KNOTS ( 'NONE', 3,
 ( #15183, #22695, #19284, #33163, #39581, #1939, #15865, #43907, #9023, #22921, #5581, #30670, #9701, #17004, #34519, #27707, #44591, #5808, #37957, #37265, #26801, #41621, #30893, #37038, #16317, #37733, #41173, #12905, #6275, #2846 ),
 .UNSPECIFIED., .F., .F.,
 ( 4, 2, 2, 1, 2, 2, 2, 1, 1, 2, 2, 2, 1, 1, 1, 2, 2, 4 ),
 ( 0.000000000000000000, 0.03125000000003415324, 0.06250000000006830647, 0.09375000000010245971, 0.1093750000001204037, 0.1250000000001383338, 0.1875000000001745826, 0.2187500000001919298, 0.2343750000002013112, 0.2421875000002059741, 0.2500000000002106648, 0.3750000000002041145, 0.4375000000001891820, 0.4687500000001709743, 0.4843750000001516565, 0.4921875000001525446, 0.5000000000001534328, 1.000000000000000000 ),
 .UNSPECIFIED. ) ;
#19254 = CARTESIAN_POINT ( 'NONE',  ( 121.9859814775786333, -9.565557343593413364, -10.61323700422348004 ) ) ;
#19255 = EDGE_LOOP ( 'NONE', ( #6819, #35614, #14591, #30381 ) ) ;
#19256 = EDGE_CURVE ( 'NONE', #15722, #1202, #23058, .T. ) ;
#19257 = CARTESIAN_POINT ( 'NONE',  ( 124.3685014775786328, 0.4262465694468514643, -12.03445270309931736 ) ) ;
#19258 = CARTESIAN_POINT ( 'NONE',  ( 123.2906948109119867, -8.166667518702819706, -8.995218007635861213 ) ) ;
#19259 = CARTESIAN_POINT ( 'NONE',  ( 125.2512653913849476, -6.287234879411991884, -6.272089152466438833 ) ) ;
#19260 = CARTESIAN_POINT ( 'NONE',  ( 125.6732148109119862, 0.5811942927096110934, -14.16772938898807510 ) ) ;
#19261 = CARTESIAN_POINT ( 'NONE',  ( 107.8433483795247838, -0.7896495226426338832, -9.318865927141430916 ) ) ;
#19262 = DIRECTION ( 'NONE',  ( 1.000000000000000000, 0.000000000000000000, -0.000000000000000000 ) ) ;
#19263 = CARTESIAN_POINT ( 'NONE',  ( 137.6867508019752506, -1.431738907681169959, -16.71479246807979635 ) ) ;
#19264 = AXIS2_PLACEMENT_3D ( 'NONE', #36293, #36519, #5292 ) ;
#19265 = CARTESIAN_POINT ( 'NONE',  ( 111.5938171295247940, 0.1403307496149613920, -13.39321520033831447 ) ) ;
#19266 = CARTESIAN_POINT ( 'NONE',  ( 79.72353890764954087, 4.236894767232761261, -4.893215200338314474 ) ) ;
#19267 = CARTESIAN_POINT ( 'NONE',  ( 137.1886586612148449, -9.913721899296946916, -11.71924858516633705 ) ) ;
#19268 = CARTESIAN_POINT ( 'NONE',  ( 120.1140014775786398, -7.894159318335828068, -9.358103419637847864 ) ) ;
#19269 = CARTESIAN_POINT ( 'NONE',  ( 125.9568481442452850, -6.344957434206665248, -7.627207830600338134 ) ) ;
#19270 = DIRECTION ( 'NONE',  ( 0.9609149988134843001, -0.1028163501681632064, 0.2570431154366505933 ) ) ;
#19271 = ORIENTED_EDGE ( 'NONE', *, *, #22576, .T. ) ;
#19272 = CARTESIAN_POINT ( 'NONE',  ( 116.5976171295247923, -9.863998795839538758, -13.39321520033831447 ) ) ;
#19273 = CARTESIAN_POINT ( 'NONE',  ( 107.9128015045248219, -6.936859964151250502, -18.39754474579286025 ) ) ;
#19274 = CARTESIAN_POINT ( 'NONE',  ( 116.2565881442453133, -0.8288870151387760510, -10.36305467784173118 ) ) ;
#19275 = VECTOR ( 'NONE', #18025, 1000.000000000000000 ) ;
#19276 = DIRECTION ( 'NONE',  ( 0.000000000000000000, -0.9242245927363026414, -0.3818493186865934419 ) ) ;
#19277 = CARTESIAN_POINT ( 'NONE',  ( 67.83464944830059551, -0.4399173918952799522, -10.39321520033831803 ) ) ;
#19278 = CARTESIAN_POINT ( 'NONE',  ( 122.5249188928271167, -8.278628333885240664, -17.13983228602120690 ) ) ;
#19280 = CARTESIAN_POINT ( 'NONE',  ( 121.4187148109119789, -6.344957434206665248, -7.627207830600338134 ) ) ;
#19279 = CARTESIAN_POINT ( 'NONE',  ( 53.69308256885118169, -7.449060273445263114, -17.89321520033831447 ) ) ;
#19281 = CARTESIAN_POINT ( 'NONE',  ( 122.6667014775786413, -2.084020599724406786, -8.691656652584148546 ) ) ;
#19282 = ORIENTED_EDGE ( 'NONE', *, *, #30927, .T. ) ;
#19283 = CARTESIAN_POINT ( 'NONE',  ( 110.2010952706806819, 0.3193521225029610777, -14.64321520033831447 ) ) ;
#19284 = CARTESIAN_POINT ( 'NONE',  ( 126.2202699136552866, 0.07868665426861087830, -14.15465197137595155 ) ) ;
#19285 = CARTESIAN_POINT ( 'NONE',  ( 112.0105358795247810, -8.402594152722688392, -9.854619843455216355 ) ) ;
#19286 = EDGE_CURVE ( 'NONE', #44000, #38238, #30129, .T. ) ;
#19287 = CARTESIAN_POINT ( 'NONE',  ( 122.8936081442453059, -9.565557343593413364, -10.61323700422348004 ) ) ;
#19288 = CARTESIAN_POINT ( 'NONE',  ( 120.2274548109119934, -9.859900752359378018, -12.68260735090039759 ) ) ;
#19289 = CARTESIAN_POINT ( 'NONE',  ( 124.7442371152574196, 2.518403514258475528, -15.85449577716609859 ) ) ;
#19290 = CARTESIAN_POINT ( 'NONE',  ( 109.6491296295247793, -4.863998795839590272, -19.15521520033831493 ) ) ;
#19291 = DIRECTION ( 'NONE',  ( 0.000000000000000000, -0.9242245927363027524, -0.3818493186865929978 ) ) ;
#19292 = DIRECTION ( 'NONE',  ( -0.9908103287288505534, 0.1352586133457950590, 0.000000000000000000 ) ) ;
#19293 = PLANE ( 'NONE',  #2988 ) ;
#19294 = CARTESIAN_POINT ( 'NONE',  ( 110.9687390045248350, 0.8980012041604421569, -15.77991374673208469 ) ) ;
#19295 = CARTESIAN_POINT ( 'NONE',  ( -13.46025930250415925, -4.921265112563996347, -18.14637807345946996 ) ) ;
#19296 = CARTESIAN_POINT ( 'NONE',  ( 116.4555358795247884, -0.7896495226426338832, -17.46756447353520159 ) ) ;
#19297 = CARTESIAN_POINT ( 'NONE',  ( 119.6034614775786196, -6.344957434206665248, -7.627207830600338134 ) ) ;
#19298 = CARTESIAN_POINT ( 'NONE',  ( 122.2128881442453263, -1.834011780172310813, -8.268836392978581529 ) ) ;
#19299 = CARTESIAN_POINT ( 'NONE',  ( 107.1488171295247867, -10.62599879583958540, -13.39321520033831447 ) ) ;
#19300 = CARTESIAN_POINT ( 'NONE',  ( 116.7671281442453335, -1.834011780172310813, -8.268836392978581529 ) ) ;
#19301 = CARTESIAN_POINT ( 'NONE',  ( 73.07463722459043254, -52.92560917005250332, -33.47856044079506432 ) ) ;
#19302 = ORIENTED_EDGE ( 'NONE', *, *, #4309, .F. ) ;
#19303 = DIRECTION ( 'NONE',  ( -1.000000000000000000, 0.000000000000000000, 0.000000000000000000 ) ) ;
#19304 = AXIS2_PLACEMENT_3D ( 'NONE', #37369, #45127, #34391 ) ;
#19305 = CARTESIAN_POINT ( 'NONE',  ( 121.1350814775786233, 0.5811942927096110934, -14.16772938898807510 ) ) ;
#19306 = CARTESIAN_POINT ( 'NONE',  ( 119.8303681442453126, -10.63000616557722466, -14.87417383870573495 ) ) ;
#19307 = EDGE_CURVE ( 'NONE', #19331, #21938, #11203, .T. ) ;
#19308 = CARTESIAN_POINT ( 'NONE',  ( 126.2972081442452890, -2.084020599724406786, -8.691656652584148546 ) ) ;
#19309 = CARTESIAN_POINT ( 'NONE',  ( 115.0653281442453277, -3.505236298600246325, -18.68346056562440793 ) ) ;
#19310 = CARTESIAN_POINT ( 'NONE',  ( 123.8579614775786126, 0.5811942927096110934, -14.16772938898807510 ) ) ;
#19311 = AXIS2_PLACEMENT_3D ( 'NONE', #38165, #45027, #20408 ) ;
#19312 = CARTESIAN_POINT ( 'NONE',  ( 109.6491296295247793, -4.863998795839590272, -19.15521520033831493 ) ) ;
#19313 = CARTESIAN_POINT ( 'NONE',  ( 119.0361948109119652, -2.084020599724406786, -8.691656652584148546 ) ) ;
#19314 = CARTESIAN_POINT ( 'NONE',  ( 121.9470836909669913, -27.84333996136784961, -14.15691383771150136 ) ) ;
#19315 = VERTEX_POINT ( 'NONE', #16224 ) ;
#19316 = CARTESIAN_POINT ( 'NONE',  ( 123.8012348109119642, 0.2603800115204892296, -16.42320221600525088 ) ) ;
#19317 = CARTESIAN_POINT ( 'NONE',  ( 73.07463722459043254, -60.14594483832745198, -36.36666953930154023 ) ) ;
#19318 = CARTESIAN_POINT ( 'NONE',  ( 123.9584548109119737, 2.250047331442289966, -9.733932798157443500 ) ) ;
#19319 = CARTESIAN_POINT ( 'NONE',  ( 115.0190408578216932, 0.04929351793716424401, -12.14321520033833934 ) ) ;
#19320 = CARTESIAN_POINT ( 'NONE',  ( 118.5823814775786360, -7.643976991954077427, -18.09477374809248928 ) ) ;
#19321 = CARTESIAN_POINT ( 'NONE',  ( 67.86702936097370298, -0.4719278425800559895, -16.39321520033831092 ) ) ;
#19322 = CARTESIAN_POINT ( 'NONE',  ( 94.20708369096698220, -26.72956082974378944, -12.96372607128127363 ) ) ;
#19323 = CARTESIAN_POINT ( 'NONE',  ( 124.3117748109119844, 0.1319031606808879209, -14.10382304977623669 ) ) ;
#19324 = CARTESIAN_POINT ( 'NONE',  ( 109.7439176093651980, 0.5600166689815611054, -14.64321520033831447 ) ) ;
#19325 = DIRECTION ( 'NONE',  ( 1.000000000000000000, 0.000000000000000000, -0.000000000000000000 ) ) ;
#19326 = CIRCLE ( 'NONE', #5481, 0.5000000000000004441 ) ;
#19327 = FACE_OUTER_BOUND ( 'NONE', #35620, .T. ) ;
#19328 = CARTESIAN_POINT ( 'NONE',  ( 123.8443641859119992, -1.409680983675146049, -17.55938974467885672 ) ) ;
#19329 = CARTESIAN_POINT ( 'NONE',  ( 116.4267681442453153, -6.222761293078241884, -8.102969835052219238 ) ) ;
#19330 = CARTESIAN_POINT ( 'NONE',  ( 123.2906948109119867, -1.833838273342659697, -17.42832698103878286 ) ) ;
#19331 = VERTEX_POINT ( 'NONE', #39935 ) ;
#19332 = CARTESIAN_POINT ( 'NONE',  ( 122.0994348109119443, 0.9020085738987339008, -11.91225656197089222 ) ) ;
#19333 = CARTESIAN_POINT ( 'NONE',  ( 114.6115148109119986, -3.383040157471821630, -19.15922257007629170 ) ) ;
#19334 = CARTESIAN_POINT ( 'NONE',  ( 115.7610046295247912, -4.863998795839590272, -18.39754474579285315 ) ) ;
#19335 = CARTESIAN_POINT ( 'NONE',  ( 112.2289948109119848, -7.643976991954077427, -18.09477374809248928 ) ) ;
#19336 = VECTOR ( 'NONE', #24277, 1000.000000000000000 ) ;
#19337 = CARTESIAN_POINT ( 'NONE',  ( 122.3830681442452857, -1.833838273342659697, -17.42832698103878286 ) ) ;
#19338 = CARTESIAN_POINT ( 'NONE',  ( 123.7445081442452874, -1.561330072975668948, -17.79121239304076951 ) ) ;
#19339 = CARTESIAN_POINT ( 'NONE',  ( 113.6079577545248043, -7.250697342233347165, -7.631215200338321125 ) ) ;
#19340 = CARTESIAN_POINT ( 'NONE',  ( 108.5378796295247810, -4.863998795839590272, -8.388885654883775800 ) ) ;
#19341 = CARTESIAN_POINT ( 'NONE',  ( 76.63408154409412987, 1.697290617957241565, -19.39321520033831447 ) ) ;
#19342 = CARTESIAN_POINT ( 'NONE',  ( 112.5126281442453120, 0.1319031606808879209, -14.10382304977623669 ) ) ;
#19343 = DIRECTION ( 'NONE',  ( 0.000000000000000000, 0.000000000000000000, -1.000000000000000000 ) ) ;
#19344 = CARTESIAN_POINT ( 'NONE',  ( 114.9275671295247889, 0.1403307496149613920, -13.39321520033831447 ) ) ;
#19345 = ORIENTED_EDGE ( 'NONE', *, *, #25993, .T. ) ;
#19346 = CARTESIAN_POINT ( 'NONE',  ( 124.4819548109119722, -2.084020599724406786, -8.691656652584148546 ) ) ;
#19347 = CARTESIAN_POINT ( 'NONE',  ( 119.3267360609119692, -3.387241619883791355, -18.17469012370385073 ) ) ;
#19348 = CARTESIAN_POINT ( 'NONE',  ( 120.3685329359119862, -4.283928203966213211, -7.183505701512925334 ) ) ;
#19349 = ORIENTED_EDGE ( 'NONE', *, *, #38190, .F. ) ;
#19350 = CARTESIAN_POINT ( 'NONE',  ( 70.19189222814998175, -67.83330054016514055, -40.33609291459782753 ) ) ;
#19351 = CARTESIAN_POINT ( 'NONE',  ( 107.9128015045248219, -6.936859964151250502, -18.39754474579286025 ) ) ;
#19352 = VERTEX_POINT ( 'NONE', #19188 ) ;
#19353 = CARTESIAN_POINT ( 'NONE',  ( 117.5045748109119756, 0.5811942927096110934, -14.16772938898807510 ) ) ;
#19354 = CARTESIAN_POINT ( 'NONE',  ( 123.0070614775786169, -10.15424416112533912, -14.75197769757731336 ) ) ;
#19355 = ADVANCED_FACE ( 'NONE', ( #33066 ), #43583, .T. ) ;
#19356 = CARTESIAN_POINT ( 'NONE',  ( 115.4624148109119943, -4.153390946401321671, -8.397313243818183892 ) ) ;
#19357 = CARTESIAN_POINT ( 'NONE',  ( 70.19189222814998175, -59.11650476797663600, -36.84940499091918298 ) ) ;
#19358 = B_SPLINE_CURVE_WITH_KNOTS ( 'NONE', 3,
 ( #36985, #43402, #5986, #19674, #26975, #13077, #19452, #43625, #33562, #33796 ),
 .UNSPECIFIED., .F., .F.,
 ( 4, 3, 3, 4 ),
 ( 5.553824967135429714E-18, 0.0002476486541971044722, 0.0004952973025691070419, 0.0009610892161188180861 ),
 .UNSPECIFIED. ) ;
#19359 = CARTESIAN_POINT ( 'NONE',  ( 114.6490365460471992, -2.191907684172563986, -18.20049396185734025 ) ) ;
#19360 = CARTESIAN_POINT ( 'NONE',  ( 115.1787814775786387, -9.988377603198976828, -10.36322818467138340 ) ) ;
#19361 = CARTESIAN_POINT ( 'NONE',  ( 111.6632702545248605, 0.1403307496149616695, -11.32035403202665336 ) ) ;
#19362 = CARTESIAN_POINT ( 'NONE',  ( 123.1772414775786189, -4.089484607189486809, -7.948022111789456723 ) ) ;
#19363 = VERTEX_POINT ( 'NONE', #13030 ) ;
#19364 = CARTESIAN_POINT ( 'NONE',  ( 114.1577014775786552, -6.344957434206662583, -7.627207830600332805 ) ) ;
#19365 = CARTESIAN_POINT ( 'NONE',  ( 113.9875214775786532, -8.899110576539710493, -16.42337572283490132 ) ) ;
#19366 = CARTESIAN_POINT ( 'NONE',  ( 143.3676850761856940, -68.13214146720427777, -20.74076566292611545 ) ) ;
#19367 = CARTESIAN_POINT ( 'NONE',  ( 126.0703014775786102, -0.1624402480850797581, -16.17319339645315424 ) ) ;
#19368 = ORIENTED_EDGE ( 'NONE', *, *, #35297, .T. ) ;
#19369 = CARTESIAN_POINT ( 'NONE',  ( 120.0572748109119772, -3.383040157471821630, -19.15922257007629170 ) ) ;
#19370 = DIRECTION ( 'NONE',  ( 0.000000000000000000, 2.168404344971010101E-16, -1.000000000000000000 ) ) ;
#19371 = CARTESIAN_POINT ( 'NONE',  ( 70.19189222814998175, -52.61716011954800365, -34.24968978710501943 ) ) ;
#19372 = CARTESIAN_POINT ( 'NONE',  ( 93.24708369096698846, -25.99489077589524300, -13.39321520033831447 ) ) ;
#19373 = CARTESIAN_POINT ( 'NONE',  ( 151.2860562277021472, -3.484218720211406772, -13.98160872758045947 ) ) ;
#19374 = CARTESIAN_POINT ( 'NONE',  ( 115.5758681442453053, -7.894159318335828068, -9.358103419637847864 ) ) ;
#19375 = CARTESIAN_POINT ( 'NONE',  ( 70.19189222814998175, -54.47411573338475677, -34.99246555962335492 ) ) ;
#19376 = CARTESIAN_POINT ( 'NONE',  ( 125.3521822035780815, -2.963544489311753516, -20.18754802458934705 ) ) ;
#19377 = AXIS2_PLACEMENT_3D ( 'NONE', #20151, #6229, #26980 ) ;
#19378 = CARTESIAN_POINT ( 'NONE',  ( 112.8529881442453160, -7.894159318335828068, -9.358103419637847864 ) ) ;
#19379 = CARTESIAN_POINT ( 'NONE',  ( 126.5241148109119393, -9.565557343593413364, -10.61323700422348004 ) ) ;
#19380 = CARTESIAN_POINT ( 'NONE',  ( 123.7022829359119811, -5.367793381288652910, -18.78638297431638904 ) ) ;
#19381 = CARTESIAN_POINT ( 'NONE',  ( 125.5597614775786326, -7.894159318335828068, -9.358103419637847864 ) ) ;
#19382 = CARTESIAN_POINT ( 'NONE',  ( 116.9373081442452929, -1.833838273342659253, -17.42832698103878286 ) ) ;
#19383 = CARTESIAN_POINT ( 'NONE',  ( 123.8012348109119642, 0.2603800115204892296, -16.42320221600525088 ) ) ;
#19384 = CARTESIAN_POINT ( 'NONE',  ( 121.1350814775786233, 0.5811942927096110934, -14.16772938898807510 ) ) ;
#19385 = ORIENTED_EDGE ( 'NONE', *, *, #25570, .T. ) ;
#19386 = CARTESIAN_POINT ( 'NONE',  ( 117.6695424678160862, -1.149058757900091265, -17.09122335155388939 ) ) ;
#19387 = CARTESIAN_POINT ( 'NONE',  ( 111.5938171295247940, -10.62599879583958540, -13.39321520033831447 ) ) ;
#19388 = CARTESIAN_POINT ( 'NONE',  ( 110.9687390045248350, -9.868328341294098749, -11.32035403202665869 ) ) ;
#19389 = CARTESIAN_POINT ( 'NONE',  ( 108.1906140045248463, 0.1403307496149616695, -15.46607636864997204 ) ) ;
#19390 = DIRECTION ( 'NONE',  ( 0.000000000000000000, 0.9284778069183720062, 0.3713878862591650232 ) ) ;
#19391 = CARTESIAN_POINT ( 'NONE',  ( 119.6601881442453106, -8.166667518702819706, -8.995218007635861213 ) ) ;
#19392 = ORIENTED_EDGE ( 'NONE', *, *, #32712, .T. ) ;
#19393 = CARTESIAN_POINT ( 'NONE',  ( 124.1593615891115547, -9.675291321254654520, -19.78473021908635943 ) ) ;
#19394 = CARTESIAN_POINT ( 'NONE',  ( 61.69189222814998175, -50.16718729050181480, 3.106784799661685526 ) ) ;
#19395 = CARTESIAN_POINT ( 'NONE',  ( 70.19189222814998175, -57.25954915413987578, -36.10662921840084749 ) ) ;
#19396 = CARTESIAN_POINT ( 'NONE',  ( 114.2144281442453178, -1.833838273342658809, -17.42832698103878286 ) ) ;
#19397 =( GEOMETRIC_REPRESENTATION_CONTEXT ( 3 ) GLOBAL_UNCERTAINTY_ASSIGNED_CONTEXT ( ( #22380 ) ) GLOBAL_UNIT_ASSIGNED_CONTEXT ( ( #29392, #32127, #22104 ) ) REPRESENTATION_CONTEXT ( 'NONE', 'WORKASPACE' ) );
#19398 = AXIS2_PLACEMENT_3D ( 'NONE', #1203, #43379, #32868 ) ;
#19399 = CARTESIAN_POINT ( 'NONE',  ( 118.0151148109119816, -10.63000616557722466, -14.87417383870573495 ) ) ;
#19400 = CARTESIAN_POINT ( 'NONE',  ( 108.3295202545248657, -10.62599879583958717, -15.77991374673208469 ) ) ;
#19401 = CARTESIAN_POINT ( 'NONE',  ( 69.69189222814998175, -41.76310523276723785, -24.39321520033831447 ) ) ;
#19402 = ORIENTED_EDGE ( 'NONE', *, *, #23992, .T. ) ;
#19403 = CARTESIAN_POINT ( 'NONE',  ( 120.9081748109119872, -4.153390946401307460, -8.397313243818183892 ) ) ;
#19404 = CARTESIAN_POINT ( 'NONE',  ( 122.0427081442452817, -9.859900752359378018, -12.68260735090039759 ) ) ;
#19405 = CARTESIAN_POINT ( 'NONE',  ( 118.8092881442453290, -9.988377603198976828, -10.36322818467138340 ) ) ;
#19406 = CARTESIAN_POINT ( 'NONE',  ( 114.3846081442453197, 0.4262465694468514643, -12.03445270309931736 ) ) ;
#19407 = CARTESIAN_POINT ( 'NONE',  ( 114.4413348109119823, -9.261995988541697145, -16.69588392320189030 ) ) ;
#19408 = CARTESIAN_POINT ( 'NONE',  ( 118.6391081442452986, -5.574606645277192740, -18.38911715685844328 ) ) ;
#19409 = CARTESIAN_POINT ( 'NONE',  ( 124.2550481442452792, -0.1624402480850797581, -16.17319339645315424 ) ) ;
#19410 = CARTESIAN_POINT ( 'NONE',  ( 120.4543614775786295, -5.574606645277164318, -18.38911715685844683 ) ) ;
#19411 = EDGE_LOOP ( 'NONE', ( #34647, #5699, #17512, #6573 ) ) ;
#19412 = CARTESIAN_POINT ( 'NONE',  ( 122.3826735609119680, 0.6414057260225851653, -11.69287257290600657 ) ) ;
#19413 = CIRCLE ( 'NONE', #12888, 2.000000000000000444 ) ;
#19414 = CARTESIAN_POINT ( 'NONE',  ( 114.4980614775786592, -7.893985811506177619, -18.51759400769804742 ) ) ;
#19415 = CARTESIAN_POINT ( 'NONE',  ( 120.3976348109119812, -7.643976991954077427, -18.09477374809248928 ) ) ;
#19416 = ORIENTED_EDGE ( 'NONE', *, *, #11637, .T. ) ;
#19417 = CARTESIAN_POINT ( 'NONE',  ( 119.8129079359119942, -5.444069387712269226, -19.60292469916370450 ) ) ;
#19418 = CARTESIAN_POINT ( 'NONE',  ( 120.0572748109119772, -3.383040157471821630, -19.15922257007629170 ) ) ;
#19419 = CARTESIAN_POINT ( 'NONE',  ( 113.3301452545248083, 0.8980012041604421569, -11.00651665394454071 ) ) ;
#19420 = CARTESIAN_POINT ( 'NONE',  ( 116.9373081442452929, -1.833838273342659253, -17.42832698103878286 ) ) ;
#19421 = CIRCLE ( 'NONE', #36171, 1.610000000000000986 ) ;
#19422 = ORIENTED_EDGE ( 'NONE', *, *, #44066, .F. ) ;
#19423 = ORIENTED_EDGE ( 'NONE', *, *, #20879, .F. ) ;
#19424 = CARTESIAN_POINT ( 'NONE',  ( 123.8579614775786126, -9.859900752359378018, -12.68260735090039759 ) ) ;
#19425 = CARTESIAN_POINT ( 'NONE',  ( 119.4900081442453086, -7.643976991954077427, -18.09477374809248928 ) ) ;
#19426 = CARTESIAN_POINT ( 'NONE',  ( 94.20708369096698220, -25.89439488952623591, -12.28775498424876211 ) ) ;
#19427 = AXIS2_PLACEMENT_3D ( 'NONE', #33029, #39451, #22344 ) ;
#19428 = FACE_OUTER_BOUND ( 'NONE', #10083, .T. ) ;
#19429 = CARTESIAN_POINT ( 'NONE',  ( 116.6536748109119941, 0.9020085738987339008, -11.91225656197089222 ) ) ;
#19430 = CARTESIAN_POINT ( 'NONE',  ( 90.48265143217095385, -26.32847964148556485, -12.58579976615069818 ) ) ;
#19431 = CARTESIAN_POINT ( 'NONE',  ( 117.5613014775786525, 0.9020085738987339008, -11.91225656197089222 ) ) ;
#19432 = EDGE_CURVE ( 'NONE', #44761, #23032, #30125, .T. ) ;
#19434 = CARTESIAN_POINT ( 'NONE',  ( 117.7882081442453170, -3.505236298600246325, -18.68346056562440793 ) ) ;
#19433 = CARTESIAN_POINT ( 'NONE',  ( 113.7038881442453402, -3.383040157471821630, -19.15922257007629170 ) ) ;
#19435 = CARTESIAN_POINT ( 'NONE',  ( 121.9859814775786333, -9.565557343593413364, -10.61323700422348004 ) ) ;
#19436 = CARTESIAN_POINT ( 'NONE',  ( 113.6471614775786492, -5.638512984488999180, -18.83840828888717311 ) ) ;
#19437 = EDGE_CURVE ( 'NONE', #11292, #34097, #29443, .T. ) ;
#19438 = EDGE_CURVE ( 'NONE', #2933, #8919, #34645, .T. ) ;
#19439 = ORIENTED_EDGE ( 'NONE', *, *, #10852, .F. ) ;
#19440 = CARTESIAN_POINT ( 'NONE',  ( 123.0637881442452937, -8.899110576539710493, -16.42337572283490132 ) ) ;
#19441 = CARTESIAN_POINT ( 'NONE',  ( 113.9762393335884383, -2.334846009198400019, -18.01015021110789149 ) ) ;
#19442 = CARTESIAN_POINT ( 'NONE',  ( 112.0799890045248475, 0.8980012041604421569, -15.77991374673208469 ) ) ;
#19443 = CARTESIAN_POINT ( 'NONE',  ( 114.8581140045248361, 0.1403307496149616695, -15.46607636864997204 ) ) ;
#19444 = CARTESIAN_POINT ( 'NONE',  ( 113.1912390045248031, 0.8980012041604421569, -15.77991374673208469 ) ) ;
#19445 = CARTESIAN_POINT ( 'NONE',  ( 118.2987481442453088, -1.561330072975668504, -17.79121239304076951 ) ) ;
#19446 = ORIENTED_EDGE ( 'NONE', *, *, #28153, .T. ) ;
#19447 = CARTESIAN_POINT ( 'NONE',  ( 120.3976348109119812, -1.834011780172310813, -8.268836392978581529 ) ) ;
#19448 = CARTESIAN_POINT ( 'NONE',  ( 63.69189222814998175, -37.86175736943883408, -4.893215200338314474 ) ) ;
#19449 = CARTESIAN_POINT ( 'NONE',  ( 109.0935046295247872, -4.863998795839590272, -7.631215200338315796 ) ) ;
#19450 = CARTESIAN_POINT ( 'NONE',  ( 121.2485348109119769, -0.4660016031367893996, -10.09054647747474043 ) ) ;
#19451 = CARTESIAN_POINT ( 'NONE',  ( 120.5678148109119832, -8.166667518702819706, -8.995218007635861213 ) ) ;
#19452 = CARTESIAN_POINT ( 'NONE',  ( 123.3883748871816266, -6.188980713775695364, -18.62212668298318619 ) ) ;
#19453 = CARTESIAN_POINT ( 'NONE',  ( 116.6292570341474288, -11.85868526616381047, -6.404461157504905522 ) ) ;
#19454 = AXIS2_PLACEMENT_3D ( 'NONE', #36854, #27069, #37076 ) ;
#19455 = EDGE_LOOP ( 'NONE', ( #31130, #39502, #37840, #5549 ) ) ;
#19456 = CARTESIAN_POINT ( 'NONE',  ( -2.417516882670096123, -7.009994832972470391, -7.554101583258010955 ) ) ;
#19457 = CARTESIAN_POINT ( 'NONE',  ( 109.2294548792482516, -10.43681072401148135, -13.08540494253950470 ) ) ;
#19458 = CARTESIAN_POINT ( 'NONE',  ( 123.2906948109119867, -1.833838273342659697, -17.42832698103878286 ) ) ;
#19459 = CARTESIAN_POINT ( 'NONE',  ( 114.0246765045248196, -2.791137627527939813, -8.388885654883777576 ) ) ;
#19460 = CARTESIAN_POINT ( 'NONE',  ( 112.8439733795247832, -1.325403438956436419, -9.854619843455211026 ) ) ;
#19461 = CARTESIAN_POINT ( 'NONE',  ( 119.7169148109119874, -0.1624402480850797581, -16.17319339645315424 ) ) ;
#19462 = CARTESIAN_POINT ( 'NONE',  ( 117.2294421295247844, 1.035107641088057973, -4.893215200338314474 ) ) ;
#19463 = CARTESIAN_POINT ( 'NONE',  ( 70.09983049117633414, -25.86019782604198980, -5.724353937072335086 ) ) ;
#19464 = CARTESIAN_POINT ( 'NONE',  ( 114.3278814775786429, 0.1319031606808879209, -14.10382304977623669 ) ) ;
#19465 = CARTESIAN_POINT ( 'NONE',  ( 123.6310548109119765, -5.638512984488999180, -18.83840828888717311 ) ) ;
#19466 = ORIENTED_EDGE ( 'NONE', *, *, #5958, .T. ) ;
#19467=STYLED_ITEM('',(#45190),#6206);
#19468 = EDGE_CURVE ( 'NONE', #4906, #22775, #16292, .T. ) ;
#19469 = CARTESIAN_POINT ( 'NONE',  ( 121.5321681442453183, -0.1624402480850797581, -16.17319339645315424 ) ) ;
#19470 = CARTESIAN_POINT ( 'NONE',  ( 115.8027748109119841, -0.4660016031367893996, -10.09054647747474043 ) ) ;
#19471 = CARTESIAN_POINT ( 'NONE',  ( 120.3409081442453044, -0.4660016031367893996, -10.09054647747474043 ) ) ;
#19472 = CARTESIAN_POINT ( 'NONE',  ( 124.1983214775786166, -1.833838273342659697, -17.42832698103878286 ) ) ;
#19473 = EDGE_LOOP ( 'NONE', ( #964, #27553, #43561, #14093, #12741, #20082 ) ) ;
#19474 = DIRECTION ( 'NONE',  ( -3.317300593186674996E-33, 1.195183497228115774E-16, -1.000000000000000000 ) ) ;
#19475 = EDGE_CURVE ( 'NONE', #34692, #14979, #2435, .T. ) ;
#19476 = EDGE_CURVE ( 'NONE', #4486, #31639, #8276, .T. ) ;
#19477 = CARTESIAN_POINT ( 'NONE',  ( 124.0281414775786146, -1.834011780172310813, -8.268836392978581529 ) ) ;
#19478 = CARTESIAN_POINT ( 'NONE',  ( 124.9801526047680227, -8.159936295607842283, -6.546456203805208318 ) ) ;
#19479 = AXIS2_PLACEMENT_3D ( 'NONE', #12390, #22636, #1874 ) ;
#19480 = CARTESIAN_POINT ( 'NONE',  ( 111.6050014775786536, 0.1319031606808879209, -14.10382304977623669 ) ) ;
#19481 = CARTESIAN_POINT ( 'NONE',  ( 108.1906140045248463, -10.62599879583958717, -11.00651665394454604 ) ) ;
#19482 = LINE ( 'NONE', #15611, #13346 ) ;
#19483 = CARTESIAN_POINT ( 'NONE',  ( 137.0982916334691026, -1.054555534231447878, -17.21706852322335379 ) ) ;
#19484 = CARTESIAN_POINT ( 'NONE',  ( 108.3989733795247759, -1.325403438956436419, -9.854619843455211026 ) ) ;
#19485 = DIRECTION ( 'NONE',  ( 0.000000000000000000, -0.9242245927363027524, -0.3818493186865928868 ) ) ;
#19486 = EDGE_CURVE ( 'NONE', #8919, #14657, #31018, .T. ) ;
#19487 = CARTESIAN_POINT ( 'NONE',  ( 71.31713442278434911, 2.423123680056909368, -16.18610841915176479 ) ) ;
#19488 = CARTESIAN_POINT ( 'NONE',  ( 118.1852948109119836, -4.153390946401325223, -8.397313243818185668 ) ) ;
#19489 = CARTESIAN_POINT ( 'NONE',  ( 126.1270281442452870, -10.30919188438810075, -12.61870101168855918 ) ) ;
#19490 = CARTESIAN_POINT ( 'NONE',  ( 126.6164971830670822, -6.329513783485987588, -18.38149871819503645 ) ) ;
#19491 = EDGE_CURVE ( 'NONE', #41326, #19352, #41963, .T. ) ;
#19492 = EDGE_CURVE ( 'NONE', #19939, #22843, #10070, .T. ) ;
#19493 = ORIENTED_EDGE ( 'NONE', *, *, #8377, .T. ) ;
#19494 = CARTESIAN_POINT ( 'NONE',  ( 116.8722546295247895, -4.863998795839590272, -18.39754474579285315 ) ) ;
#19495 = VECTOR ( 'NONE', #16085, 1000.000000000000000 ) ;
#19496 = CARTESIAN_POINT ( 'NONE',  ( 115.6893214775786447, -9.859900752359374465, -12.68260735090039404 ) ) ;
#19497 = CARTESIAN_POINT ( 'NONE',  ( 116.5944421295247793, -4.863998795839590272, -18.39321520033831803 ) ) ;
#19498 = CARTESIAN_POINT ( 'NONE',  ( 67.79187456311957760, -0.4014585417718678495, -10.39321520033831447 ) ) ;
#19499 = CARTESIAN_POINT ( 'NONE',  ( 119.7434548109119703, -13.11073630560948722, -15.94021774473354114 ) ) ;
#19501 = CARTESIAN_POINT ( 'NONE',  ( 121.1350814775786233, 0.5811942927096110934, -14.16772938898807510 ) ) ;
#19500 = CARTESIAN_POINT ( 'NONE',  ( 114.3216384760652744, 0.6362173239733635022, -12.14321520033831625 ) ) ;
#19502 = CARTESIAN_POINT ( 'NONE',  ( 123.3474214775786209, -0.1624402480850797581, -16.17319339645315424 ) ) ;
#19503 = ORIENTED_EDGE ( 'NONE', *, *, #8947, .F. ) ;
#19504 = CARTESIAN_POINT ( 'NONE',  ( 109.8889130180080826, 0.7607806665037644134, -14.64321520033833579 ) ) ;
#19505 = CARTESIAN_POINT ( 'NONE',  ( 125.4463081442452932, -5.638512984488999180, -18.83840828888717311 ) ) ;
#19506 = CARTESIAN_POINT ( 'NONE',  ( 112.2188952545247531, -9.868328341294098749, -15.46607636864997204 ) ) ;
#19507 = B_SPLINE_CURVE_WITH_KNOTS ( 'NONE', 3,
 ( #44339, #30193, #37707, #16519, #27229, #12651, #16291, #13325, #33586, #41147 ),
 .UNSPECIFIED., .F., .F.,
 ( 4, 3, 3, 4 ),
 ( 0.000000000000000000, 0.0001671877548681284921, 0.0003343755096277714980, 0.0006463528481650629171 ),
 .UNSPECIFIED. ) ;
#19508 = CARTESIAN_POINT ( 'NONE',  ( 122.2128881442453263, -7.643976991954077427, -18.09477374809248928 ) ) ;
#19509 = CARTESIAN_POINT ( 'NONE',  ( 120.5678148109119832, -1.833838273342659253, -17.42832698103878286 ) ) ;
#19510 = CARTESIAN_POINT ( 'NONE',  ( 125.0532895624267837, 1.228647770399326156, -17.81034849661567065 ) ) ;
#19511 = CARTESIAN_POINT ( 'NONE',  ( 113.6774108795247997, -1.325403438956436419, -16.93181055722141792 ) ) ;
#19512 = CARTESIAN_POINT ( 'NONE',  ( 78.69189222814998175, -48.76310523276723785, -24.89321520033831447 ) ) ;
#19513 = CARTESIAN_POINT ( 'NONE',  ( 89.12784890491134604, -25.99489077589524300, -13.39321520033831625 ) ) ;
#19514 = CARTESIAN_POINT ( 'NONE',  ( 112.4675314748722599, -0.1020945015694913471, -15.74893487844866691 ) ) ;
#19515 = CIRCLE ( 'NONE', #2022, 5.999999999999997335 ) ;
#19516 = CARTESIAN_POINT ( 'NONE',  ( 111.8021765045248372, -7.250697342233347165, -19.15521520033831138 ) ) ;
#19517 = CARTESIAN_POINT ( 'NONE',  ( 116.2175407567830518, 2.316852922634951017, -20.12813529906391352 ) ) ;
#19518 = CARTESIAN_POINT ( 'NONE',  ( 114.5803015045248117, -2.477300249445798297, -7.631215200338321125 ) ) ;
#19519 = CARTESIAN_POINT ( 'NONE',  ( 120.0005481442453146, -5.638512984488999180, -18.83840828888717311 ) ) ;
#19520 = CARTESIAN_POINT ( 'NONE',  ( 121.4187148109119789, -6.344957434206665248, -7.627207830600338134 ) ) ;
#19521 = CARTESIAN_POINT ( 'NONE',  ( 106.8015515045248378, -2.477300249445798297, -7.631215200338321125 ) ) ;
#19522 = CARTESIAN_POINT ( 'NONE',  ( 115.2355081442453155, -10.30919188438810075, -12.61870101168855918 ) ) ;
#19523 = DIRECTION ( 'NONE',  ( -1.000000000000000000, 0.000000000000000000, 0.000000000000000000 ) ) ;
#19524 = VERTEX_POINT ( 'NONE', #7075 ) ;
#19525 = CARTESIAN_POINT ( 'NONE',  ( 109.2914656780534841, 0.1539732345883643161, -12.14321520033831625 ) ) ;
#19526 = CARTESIAN_POINT ( 'NONE',  ( 111.9453614775786434, -7.894159318335828068, -9.358103419637847864 ) ) ;
#19527 = CARTESIAN_POINT ( 'NONE',  ( 121.0216281442452981, -1.561330072975668948, -17.79121239304076951 ) ) ;
#19528 = CARTESIAN_POINT ( 'NONE',  ( 124.1415948109119540, -3.505236298600246325, -18.68346056562440793 ) ) ;
#19529 = ITEM_DEFINED_TRANSFORMATION ( 'NONE', 'NONE', #25703,  #12375 ) ;
#19530 = CARTESIAN_POINT ( 'NONE',  ( 113.7606148109119886, -7.894159318335828068, -9.358103419637847864 ) ) ;
#19531 = VERTEX_POINT ( 'NONE', #23971 ) ;
#19532 = CARTESIAN_POINT ( 'NONE',  ( 115.8595014775786609, -7.643976991954077427, -18.09477374809248928 ) ) ;
#19533 = CARTESIAN_POINT ( 'NONE',  ( 124.7088614775786226, 0.2603800115204892296, -16.42320221600525088 ) ) ;
#19534 = CARTESIAN_POINT ( 'NONE',  ( 108.8851452545248151, 0.8980012041604421569, -11.00651665394454071 ) ) ;
#19535 = CARTESIAN_POINT ( 'NONE',  ( 121.1918081442452859, -10.15424416112533912, -14.75197769757731336 ) ) ;
#19536 = CARTESIAN_POINT ( 'NONE',  ( 110.6909265045248247, -7.250697342233347165, -19.15521520033832203 ) ) ;
#19537 = DIRECTION ( 'NONE',  ( 1.000000000000000000, 0.000000000000000000, -0.000000000000000000 ) ) ;
#19538 = ORIENTED_EDGE ( 'NONE', *, *, #42605, .F. ) ;
#19539 = ADVANCED_FACE ( 'NONE', ( #6633 ), #6016, .F. ) ;
#19540 = CARTESIAN_POINT ( 'NONE',  ( 122.8688454359119646, 0.5291689781388270175, -13.89700978578772705 ) ) ;
#19541 = CARTESIAN_POINT ( 'NONE',  ( 121.1918081442452859, 0.9020085738987339008, -11.91225656197089222 ) ) ;
#19542 = DIRECTION ( 'NONE',  ( -0.000000000000000000, -0.9242245927363028635, -0.3818493186865929423 ) ) ;
#19543 = AXIS2_PLACEMENT_3D ( 'NONE', #44663, #10225, #30740 ) ;
#19544 = CARTESIAN_POINT ( 'NONE',  ( 67.52555172610438206, -0.2286232172799360363, -16.39321520033831803 ) ) ;
#19545 = CARTESIAN_POINT ( 'NONE',  ( 92.26512299712632625, -23.76310523276723785, -6.893215200338315363 ) ) ;
#19546 = CARTESIAN_POINT ( 'NONE',  ( 123.2339681442453241, -3.505236298600246325, -18.68346056562440793 ) ) ;
#19547 = CARTESIAN_POINT ( 'NONE',  ( 61.76986277844709861, -39.32091226840162079, -4.893215200338314474 ) ) ;
#19548 = CARTESIAN_POINT ( 'NONE',  ( 123.4608748109119745, 0.4262465694468514643, -12.03445270309931736 ) ) ;
#19549 = CARTESIAN_POINT ( 'NONE',  ( 125.3570663707213839, -11.61100471653260513, -15.41365316013039255 ) ) ;
#19550 = CARTESIAN_POINT ( 'NONE',  ( 126.0135748109119902, -8.166667518702819706, -8.995218007635861213 ) ) ;
#19551 = CARTESIAN_POINT ( 'NONE',  ( 117.1074881442453233, 0.4262465694468514643, -12.03445270309931736 ) ) ;
#19552 = CARTESIAN_POINT ( 'NONE',  ( 119.7434548109119845, -1.456678546396870333, -17.70209537461181526 ) ) ;
#19553 = ORIENTED_EDGE ( 'NONE', *, *, #3091, .T. ) ;
#19554 = CARTESIAN_POINT ( 'NONE',  ( 123.0637881442452937, -0.4660016031367893996, -10.09054647747474043 ) ) ;
#19555 = ADVANCED_FACE ( 'NONE', ( #27160 ), #44724, .T. ) ;
#19556 = CARTESIAN_POINT ( 'NONE',  ( 114.2144281442453178, -8.166667518702817929, -8.995218007635859436 ) ) ;
#19557 = CARTESIAN_POINT ( 'NONE',  ( 114.3024890045248156, -9.868328341294098749, -11.32035403202665869 ) ) ;
#19558 = CARTESIAN_POINT ( 'NONE',  ( 3.060777270043529619, -5.064559853354640317, -17.89321520033831447 ) ) ;
#19559 = CARTESIAN_POINT ( 'NONE',  ( 122.5532481442453019, 0.4262465694468514643, -12.03445270309931736 ) ) ;
#19560 = CARTESIAN_POINT ( 'NONE',  ( 123.4608748109119745, -10.63000616557722466, -14.87417383870573495 ) ) ;
#19561 = CARTESIAN_POINT ( 'NONE',  ( 113.7468640045248236, -10.62599879583958717, -11.00651665394454604 ) ) ;
#19562 = CARTESIAN_POINT ( 'NONE',  ( 108.1906140045248463, 0.1403307496149616695, -15.46607636864997204 ) ) ;
#19563 = CARTESIAN_POINT ( 'NONE',  ( 82.83387690911449397, -31.80118368680629715, -23.16660311822836960 ) ) ;
#19564 = CARTESIAN_POINT ( 'NONE',  ( 113.0231681442453180, -10.15424416112533912, -14.75197769757731336 ) ) ;
#19565 = CARTESIAN_POINT ( 'NONE',  ( 117.9016614775786280, -0.1624402480850797581, -16.17319339645315424 ) ) ;
#19566 = DIRECTION ( 'NONE',  ( -0.8636456077245086016, 0.5040994586965593660, 0.000000000000000000 ) ) ;
#19567 = CARTESIAN_POINT ( 'NONE',  ( 113.2606921295247702, -9.868328341294093420, -13.39321520033831447 ) ) ;
#19568 = EDGE_LOOP ( 'NONE', ( #31183, #43520, #44568, #17580 ) ) ;
#19569 = CARTESIAN_POINT ( 'NONE',  ( 125.0492214775786266, -3.505236298600246325, -18.68346056562440793 ) ) ;
#19570 = CARTESIAN_POINT ( 'NONE',  ( 123.8411891859119862, -8.844754642576884152, -8.592115655440050404 ) ) ;
#19571 = CARTESIAN_POINT ( 'NONE',  ( 120.7852516859119731, -9.665098340737509730, -17.37397104707595474 ) ) ;
#19572 = EDGE_LOOP ( 'NONE', ( #1269, #37182, #28960, #13771 ) ) ;
#19573 = CYLINDRICAL_SURFACE ( 'NONE', #27564, 3.000000000000001776 ) ;
#19574 = CARTESIAN_POINT ( 'NONE',  ( 116.4165695033805292, -11.97005334918662101, -21.03157055382677854 ) ) ;
#19575 = VERTEX_POINT ( 'NONE', #27831 ) ;
#19576 = CARTESIAN_POINT ( 'NONE',  ( 118.8092881442453290, -9.988377603198976828, -10.36322818467138340 ) ) ;
#19577 = CARTESIAN_POINT ( 'NONE',  ( 124.1983214775786166, -1.833838273342659697, -17.42832698103878286 ) ) ;
#19578 = CARTESIAN_POINT ( 'NONE',  ( 115.5758681442453053, -7.894159318335828068, -9.358103419637847864 ) ) ;
#19579 = SURFACE_SIDE_STYLE ('',( #23921 ) ) ;
#19580 = DIRECTION ( 'NONE',  ( -0.9609149988134837450, 0.1028163501681639419, -0.2570431154366518145 ) ) ;
#19581 = CARTESIAN_POINT ( 'NONE',  ( 71.90980237029992850, -25.93883227901748967, -4.893215200338314474 ) ) ;
#19582 = CARTESIAN_POINT ( 'NONE',  ( 113.4769814775786330, -10.63000616557722466, -14.87417383870573495 ) ) ;
#19583 = CARTESIAN_POINT ( 'NONE',  ( 113.6079577545248043, -2.791137627527939813, -18.39754474579286025 ) ) ;
#19584 = CARTESIAN_POINT ( 'NONE',  ( 123.8012348109119642, 0.2603800115204892296, -16.42320221600525088 ) ) ;
#19585 = CYLINDRICAL_SURFACE ( 'NONE', #15543, 1.999999999999998890 ) ;
#19586 = ORIENTED_EDGE ( 'NONE', *, *, #42601, .T. ) ;
#19587 = CARTESIAN_POINT ( 'NONE',  ( 115.5191414775786569, -3.383040157471821630, -19.15922257007629170 ) ) ;
#19588 = B_SPLINE_CURVE_WITH_KNOTS ( 'NONE', 3,
 ( #38395, #30677, #7167, #21078, #14467, #15142, #7851, #29048, #38848, #7388 ),
 .UNSPECIFIED., .F., .F.,
 ( 4, 3, 3, 4 ),
 ( 0.000000000000000000, 0.0001671877560958105107, 0.0003343755126086559717, 0.0006438490228507209303 ),
 .UNSPECIFIED. ) ;
#19589 = CARTESIAN_POINT ( 'NONE',  ( 114.7816948109119863, -9.859900752359374465, -12.68260735090039404 ) ) ;
#19590 = CARTESIAN_POINT ( 'NONE',  ( 126.8137406967727827, -4.694980012604976771, -18.68855277172357177 ) ) ;
#19591 = CARTESIAN_POINT ( 'NONE',  ( 126.6942948109119840, -8.899110576539710493, -16.42337572283490132 ) ) ;
#19592 = ORIENTED_EDGE ( 'NONE', *, *, #11107, .F. ) ;
#19593 = CARTESIAN_POINT ( 'NONE',  ( 121.4187148109119789, -6.344957434206665248, -7.627207830600338134 ) ) ;
#19594 = DIRECTION ( 'NONE',  ( 0.000000000000000000, -0.4669533266896289114, -0.8842819633428518067 ) ) ;
#19595 = DIRECTION ( 'NONE',  ( -1.000000000000000000, 0.000000000000000000, 0.000000000000000000 ) ) ;
#19596 = CARTESIAN_POINT ( 'NONE',  ( 124.7061593007352371, -1.353583375765361696, -20.37564943805809747 ) ) ;
#19597 = CARTESIAN_POINT ( 'NONE',  ( 136.8340972670082181, -2.869431185927890038, -8.189930540114788826 ) ) ;
#19598 = CARTESIAN_POINT ( 'NONE',  ( 112.4559014775786778, -0.1624402480850797581, -16.17319339645315424 ) ) ;
#19599 = CARTESIAN_POINT ( 'NONE',  ( 70.36267391504958368, -5.685877709920885259, -4.893215200338314474 ) ) ;
#19600 = ADVANCED_FACE ( 'NONE', ( #10 ), #6759, .T. ) ;
#19601 = CARTESIAN_POINT ( 'NONE',  ( 124.2773744744968951, -3.869742919590428265, -21.30530514842164536 ) ) ;
#19602 = CARTESIAN_POINT ( 'NONE',  ( 116.8238548109119819, -5.574606645277164318, -18.38911715685844683 ) ) ;
#19603 = CARTESIAN_POINT ( 'NONE',  ( 113.3635281442453504, -9.988377603198976828, -10.36322818467138340 ) ) ;
#19604 = CARTESIAN_POINT ( 'NONE',  ( 121.5492360609119800, -3.387241619883791355, -18.17469012370385073 ) ) ;
#19605 = CARTESIAN_POINT ( 'NONE',  ( 113.7606148109119886, -1.561330072975668060, -17.79121239304076596 ) ) ;
#19606 = CARTESIAN_POINT ( 'NONE',  ( 117.2209414775786485, -2.084020599724406786, -8.691656652584148546 ) ) ;
#19607 = CARTESIAN_POINT ( 'NONE',  ( 124.8223148109119762, 0.9020085738987339008, -11.91225656197089222 ) ) ;
#19608 = CARTESIAN_POINT ( 'NONE',  ( 122.3830681442452857, -8.166667518702819706, -8.995218007635861213 ) ) ;
#19609 = EDGE_LOOP ( 'NONE', ( #235, #31951, #40012, #28671 ) ) ;
#19610 = CARTESIAN_POINT ( 'NONE',  ( 111.7751814775786556, -7.893985811506177619, -18.51759400769804742 ) ) ;
#19611 = CARTESIAN_POINT ( 'NONE',  ( 111.0381921295247878, 0.8980012041604618078, -13.39321520033831447 ) ) ;
#19612 = CARTESIAN_POINT ( 'NONE',  ( 109.6491296295247793, -4.863998795839590272, -8.388885654883775800 ) ) ;
#19613 = CARTESIAN_POINT ( 'NONE',  ( 110.1353015045248469, -6.936859964151250502, -18.39754474579286025 ) ) ;
#19614 = CARTESIAN_POINT ( 'NONE',  ( 64.29809874639587974, -36.27217697897505388, -5.693345502272438630 ) ) ;
#19615 = CARTESIAN_POINT ( 'NONE',  ( 119.4332814775786318, -0.4660016031367893996, -10.09054647747474043 ) ) ;
#19616 = VERTEX_POINT ( 'NONE', #17349 ) ;
#19617 = CARTESIAN_POINT ( 'NONE',  ( 125.4213865762419999, -9.147205927423879501, -18.78468083046782056 ) ) ;
#19618 = DIRECTION ( 'NONE',  ( -0.9908103287288503314, 0.1352586133457956419, 0.000000000000000000 ) ) ;
#19619 = CARTESIAN_POINT ( 'NONE',  ( 117.2294421295247417, -10.73794132348372266, -21.89321520033831092 ) ) ;
#19620 = CARTESIAN_POINT ( 'NONE',  ( 115.8027748109119841, -8.899110576539710493, -16.42337572283490132 ) ) ;
#19621 = CARTESIAN_POINT ( 'NONE',  ( 106.6626452545248611, -9.868328341294098749, -15.46607636864997204 ) ) ;
#19622 = CARTESIAN_POINT ( 'NONE',  ( 118.5256548109119876, -0.4660016031367893996, -10.09054647747474043 ) ) ;
#19623 = CARTESIAN_POINT ( 'NONE',  ( 115.1359265045248605, -2.791137627527939813, -8.388885654883777576 ) ) ;
#19624 = DIRECTION ( 'NONE',  ( -0.000000000000000000, -0.9284778069183720062, -0.3713878862591650232 ) ) ;
#19625 = EDGE_LOOP ( 'NONE', ( #26834, #3242, #24528, #23051 ) ) ;
#19626 = DIRECTION ( 'NONE',  ( 0.000000000000000000, 0.4669533266896288559, 0.8842819633428518067 ) ) ;
#19627 = CARTESIAN_POINT ( 'NONE',  ( 122.7801548109119665, -6.222761293078241884, -8.102969835052219238 ) ) ;
#19628 = CARTESIAN_POINT ( 'NONE',  ( 118.9794681442453026, -9.261995988541697145, -16.69588392320189030 ) ) ;
#19629 = EDGE_CURVE ( 'NONE', #5448, #14958, #29653, .T. ) ;
#19630 = CARTESIAN_POINT ( 'NONE',  ( 115.0653281442453277, -3.505236298600246325, -18.68346056562440793 ) ) ;
#19631 = CARTESIAN_POINT ( 'NONE',  ( 116.6536748109119941, 0.9020085738987339008, -11.91225656197089222 ) ) ;
#19632 = CARTESIAN_POINT ( 'NONE',  ( 118.0831236215688307, -1.135392229370316919, -17.10942237759952533 ) ) ;
#19633 = CARTESIAN_POINT ( 'NONE',  ( 122.6667014775786413, -2.084020599724406786, -8.691656652584148546 ) ) ;
#19634 = CARTESIAN_POINT ( 'NONE',  ( 119.9438214775786378, -2.084020599724406786, -8.691656652584148546 ) ) ;
#19635 = EDGE_LOOP ( 'NONE', ( #33747, #8966, #26140, #11191, #37633, #5385, #27514, #43292, #18386, #7372, #43262, #25615, #41759, #9769 ) ) ;
#19636 = CARTESIAN_POINT ( 'NONE',  ( 119.2737891406318766, 0.3208234527006367798, -15.99825685930877839 ) ) ;
#19637 = CARTESIAN_POINT ( 'NONE',  ( 113.0798948109119948, -0.4660016031367893996, -10.09054647747474043 ) ) ;
#19638 = CARTESIAN_POINT ( 'NONE',  ( 122.7801548109119665, -6.222761293078241884, -8.102969835052219238 ) ) ;
#19639 = ORIENTED_EDGE ( 'NONE', *, *, #9904, .F. ) ;
#19640 = CARTESIAN_POINT ( 'NONE',  ( 120.0212673109119805, 0.2312338769422704887, -16.08380026872395874 ) ) ;
#19641 = CARTESIAN_POINT ( 'NONE',  ( 120.3409081442453044, -0.4660016031367893996, -10.09054647747474043 ) ) ;
#19642 = CARTESIAN_POINT ( 'NONE',  ( 113.6774108795247997, -8.938348069036489818, -9.318865927141430916 ) ) ;
#19643 = CARTESIAN_POINT ( 'NONE',  ( 115.4624148109119943, -4.153390946401321671, -8.397313243818183892 ) ) ;
#19644 = EDGE_LOOP ( 'NONE', ( #37679, #42244, #38657, #26043 ) ) ;
#19645 = ORIENTED_EDGE ( 'NONE', *, *, #24530, .F. ) ;
#19646 = VECTOR ( 'NONE', #21669, 1000.000000000000000 ) ;
#19647 = CARTESIAN_POINT ( 'NONE',  ( 125.1059481442452750, -1.833838273342660141, -17.42832698103878286 ) ) ;
#19648 = CARTESIAN_POINT ( 'NONE',  ( 121.1350814775786233, -9.859900752359378018, -12.68260735090039759 ) ) ;
#19649 = AXIS2_PLACEMENT_3D ( 'NONE', #35849, #18544, #1645 ) ;
#19650 = DIRECTION ( 'NONE',  ( 0.8636456077245092677, -0.5040994586965584778, 0.000000000000000000 ) ) ;
#19651 = ORIENTED_EDGE ( 'NONE', *, *, #33363, .T. ) ;
#19652 = CARTESIAN_POINT ( 'NONE',  ( 119.8303681442453126, -10.63000616557722466, -14.87417383870573495 ) ) ;
#19653 = FACE_OUTER_BOUND ( 'NONE', #5167, .T. ) ;
#19654 = CARTESIAN_POINT ( 'NONE',  ( 117.7314814775786260, -4.089484607189486809, -7.948022111789456723 ) ) ;
#19656 = CARTESIAN_POINT ( 'NONE',  ( 114.7249681442453237, -9.565557343593413364, -10.61323700422348004 ) ) ;
#19655 = CARTESIAN_POINT ( 'NONE',  ( 115.8027748109119841, -0.4660016031367893996, -10.09054647747474043 ) ) ;
#19657 = CARTESIAN_POINT ( 'NONE',  ( 124.8223148109119762, -10.15424416112533912, -14.75197769757731336 ) ) ;
#19658 = CARTESIAN_POINT ( 'NONE',  ( 111.7184548109119788, -9.261995988541697145, -16.69588392320189030 ) ) ;
#19659 = ORIENTED_EDGE ( 'NONE', *, *, #42306, .F. ) ;
#19660 = CARTESIAN_POINT ( 'NONE',  ( 122.4397948109119767, -0.1624402480850797581, -16.17319339645315424 ) ) ;
#19661 = CARTESIAN_POINT ( 'NONE',  ( 123.4041481442452834, -10.30919188438809364, -12.61870101168852187 ) ) ;
#19662 = DIRECTION ( 'NONE',  ( -0.000000000000000000, -0.9284778069183721172, -0.3713878862591650232 ) ) ;
#19663 = CARTESIAN_POINT ( 'NONE',  ( 113.8857702545248003, -10.62599879583958717, -15.77991374673208469 ) ) ;
#19664 = CARTESIAN_POINT ( 'NONE',  ( 112.0105358795247810, -8.402594152722688392, -9.854619843455216355 ) ) ;
#19665 = CARTESIAN_POINT ( 'NONE',  ( 111.8021765045248372, -7.250697342233347165, -19.15521520033831138 ) ) ;
#19666 = AXIS2_PLACEMENT_3D ( 'NONE', #28487, #10488, #28038 ) ;
#19667 = CARTESIAN_POINT ( 'NONE',  ( 121.6456214775786293, -10.63000616557722466, -14.87417383870573495 ) ) ;
#19668 = ORIENTED_EDGE ( 'NONE', *, *, #17337, .T. ) ;
#19669 = CARTESIAN_POINT ( 'NONE',  ( 121.1350814775786233, 0.5811942927096110934, -14.16772938898807510 ) ) ;
#19670 = CARTESIAN_POINT ( 'NONE',  ( 113.1933481442453058, -5.574606645277164318, -18.38911715685844683 ) ) ;
#19671 = DIRECTION ( 'NONE',  ( 0.000000000000000000, -0.4669533266896289114, -0.8842819633428518067 ) ) ;
#19672 = CARTESIAN_POINT ( 'NONE',  ( 119.0361948109119652, -7.893985811506177619, -18.51759400769804742 ) ) ;
#19673 = CARTESIAN_POINT ( 'NONE',  ( 120.9649014775786355, -3.383040157471821630, -19.15922257007629170 ) ) ;
#19674 = CARTESIAN_POINT ( 'NONE',  ( 123.5330849628857237, -6.095137211460710525, -18.44441274085890115 ) ) ;
#19675 = CARTESIAN_POINT ( 'NONE',  ( 122.4965214775786251, 0.1319031606808879209, -14.10382304977623669 ) ) ;
#19676 = CARTESIAN_POINT ( 'NONE',  ( 115.5950730757767531, -0.9924539043446216624, -17.29976612834909133 ) ) ;
#19677 = CARTESIAN_POINT ( 'NONE',  ( 123.4939235609119663, 0.6414057260225851653, -11.69287257290600657 ) ) ;
#19678 = ORIENTED_EDGE ( 'NONE', *, *, #12758, .F. ) ;
#19679 = CARTESIAN_POINT ( 'NONE',  ( -2.848861189601162192, -7.139067047498250496, -7.411210244931162094 ) ) ;
#19680 = AXIS2_PLACEMENT_3D ( 'NONE', #41682, #44657, #10443 ) ;
#19681 = DIRECTION ( 'NONE',  ( -0.000000000000000000, -0.9284778069183718952, -0.3713878862591649677 ) ) ;
#19682 = CARTESIAN_POINT ( 'NONE',  ( 124.1983214775786166, -1.833838273342659697, -17.42832698103878286 ) ) ;
#19683 = CARTESIAN_POINT ( 'NONE',  ( 116.1082702545247827, -10.62599879583958717, -15.77991374673208469 ) ) ;
#19684 = CARTESIAN_POINT ( 'NONE',  ( 112.0105358795248804, -8.402594152722688392, -9.854619843455216355 ) ) ;
#19685 = CIRCLE ( 'NONE', #27, 2.999999999999999556 ) ;
#19686 = CARTESIAN_POINT ( 'NONE',  ( 117.6180281442453150, -8.899110576539710493, -16.42337572283490132 ) ) ;
#19687 = CARTESIAN_POINT ( 'NONE',  ( 80.19189222814998175, -75.31442247550837976, -37.94335727672635272 ) ) ;
#19688 = CARTESIAN_POINT ( 'NONE',  ( 68.96255064148981262, -26.01231434226903616, -5.893215200338315363 ) ) ;
#19689 = CARTESIAN_POINT ( 'NONE',  ( 111.9453614775786434, -7.894159318335828068, -9.358103419637847864 ) ) ;
#19690 = CARTESIAN_POINT ( 'NONE',  ( 125.3328548109119964, -9.261995988541697145, -16.69588392320189030 ) ) ;
#19691 = ORIENTED_EDGE ( 'NONE', *, *, #15010, .F. ) ;
#19692 = CARTESIAN_POINT ( 'NONE',  ( 122.7801548109119665, -6.222761293078241884, -8.102969835052219238 ) ) ;
#19693 = CARTESIAN_POINT ( 'NONE',  ( 115.4056881442453459, -7.893985811506177619, -18.51759400769804742 ) ) ;
#19694 = CARTESIAN_POINT ( 'NONE',  ( 125.2761281442453054, -10.63000616557722466, -14.87417383870573495 ) ) ;
#19695 = CARTESIAN_POINT ( 'NONE',  ( 123.6877814775786533, -6.222761293078241884, -8.102969835052219238 ) ) ;
#19696 = ORIENTED_EDGE ( 'NONE', *, *, #18895, .T. ) ;
#19697 = CARTESIAN_POINT ( 'NONE',  ( 120.3925890224331710, -4.681800857092175860, -18.57451437749315559 ) ) ;
#19698 = EDGE_CURVE ( 'NONE', #20261, #8479, #39522, .T. ) ;
#19699 = CARTESIAN_POINT ( 'NONE',  ( 122.5532481442453019, -10.63000616557722466, -14.87417383870573495 ) ) ;
#19700 = VECTOR ( 'NONE', #41013, 1000.000000000000114 ) ;
#19701 = CARTESIAN_POINT ( 'NONE',  ( 114.7816948109119863, -9.859900752359374465, -12.68260735090039404 ) ) ;
#19702 = CARTESIAN_POINT ( 'NONE',  ( 125.0492214775786266, -6.344957434206665248, -7.627207830600338134 ) ) ;
#19703 = CARTESIAN_POINT ( 'NONE',  ( 106.1764733795248219, -8.938348069036489818, -17.46756447353520159 ) ) ;
#19704 = DIRECTION ( 'NONE',  ( 0.000000000000000000, -0.3818493186865936084, 0.9242245927363024194 ) ) ;
#19705 = ORIENTED_EDGE ( 'NONE', *, *, #19251, .T. ) ;
#19706 = CARTESIAN_POINT ( 'NONE',  ( 137.6297597661404950, -1.384417142403913559, -16.77780847371255035 ) ) ;
#19707 = CARTESIAN_POINT ( 'NONE',  ( 110.3436608795247764, -1.325403438956436419, -16.93181055722141792 ) ) ;
#19708 = VECTOR ( 'NONE', #32014, 1000.000000000000114 ) ;
#19709 = DIRECTION ( 'NONE',  ( -0.6383198453882299450, -0.7697712484781087383, 0.000000000000000000 ) ) ;
#19710 = CIRCLE ( 'NONE', #18252, 2.999999999999999556 ) ;
#19711 = CARTESIAN_POINT ( 'NONE',  ( 118.2420214775786320, -6.222761293078241884, -8.102969835052219238 ) ) ;
#19712 = CARTESIAN_POINT ( 'NONE',  ( 115.5758681442453053, -7.894159318335828068, -9.358103419637847864 ) ) ;
#19713 = CARTESIAN_POINT ( 'NONE',  ( 126.4750299824170554, -0.4299843489097670002, -10.81661262080413977 ) ) ;
#19714 = VERTEX_POINT ( 'NONE', #34858 ) ;
#19715 = CARTESIAN_POINT ( 'NONE',  ( 112.1240771095751114, -8.918610395140916580, -16.31999322929525675 ) ) ;
#19716 = CARTESIAN_POINT ( 'NONE',  ( 115.2922348109119781, 0.4262465694468514643, -12.03445270309931736 ) ) ;
#19717 = CARTESIAN_POINT ( 'NONE',  ( 112.5693548109119888, 0.4262465694468514643, -12.03445270309931736 ) ) ;
#19718 = ADVANCED_FACE ( 'NONE', ( #13484 ), #9679, .T. ) ;
#19719 = CARTESIAN_POINT ( 'NONE',  ( 65.98944182936091352, -0.1558845086392504908, -10.39321520033831447 ) ) ;
#19720 = DIRECTION ( 'NONE',  ( 0.000000000000000000, 0.000000000000000000, -1.000000000000000000 ) ) ;
#19722 = CARTESIAN_POINT ( 'NONE',  ( 122.3830681442452857, -8.166667518702819706, -8.995218007635861213 ) ) ;
#19721 = DIRECTION ( 'NONE',  ( 0.000000000000000000, 0.6004852223388321697, -0.7996358532186279566 ) ) ;
#19723 = CARTESIAN_POINT ( 'NONE',  ( 121.5321681442453183, -0.1624402480850797581, -16.17319339645315424 ) ) ;
#19724 = ORIENTED_EDGE ( 'NONE', *, *, #30077, .T. ) ;
#19725 = DIRECTION ( 'NONE',  ( 1.000000000000000000, 0.000000000000000000, 0.000000000000000000 ) ) ;
#19726 = DIRECTION ( 'NONE',  ( 1.000000000000000000, 0.000000000000000000, 0.000000000000000000 ) ) ;
#19727 = CARTESIAN_POINT ( 'NONE',  ( 109.7880358795247986, -8.402594152722688392, -9.854619843455216355 ) ) ;
#19728 = ADVANCED_FACE ( 'NONE', ( #3645 ), #31458, .F. ) ;
#19729 = CARTESIAN_POINT ( 'NONE',  ( 124.2550481442452792, -0.1624402480850797581, -16.17319339645315424 ) ) ;
#19730 = CARTESIAN_POINT ( 'NONE',  ( 120.3976348109119812, -7.643976991954077427, -18.09477374809248928 ) ) ;
#19731 = ADVANCED_FACE ( 'NONE', ( #37408 ), #3102, .T. ) ;
#19732 = CARTESIAN_POINT ( 'NONE',  ( 119.4847958011494171, -1.149058757900107697, -17.09122335155391781 ) ) ;
#19733 = CARTESIAN_POINT ( 'NONE',  ( 105.6903015045248253, -2.477300249445798297, -7.631215200338321125 ) ) ;
#19734 = CARTESIAN_POINT ( 'NONE',  ( 116.8805814775786587, -6.344957434206656366, -7.627207830600330141 ) ) ;
#19735 = CARTESIAN_POINT ( 'NONE',  ( 112.2289948109119848, -7.643976991954077427, -18.09477374809248218 ) ) ;
#19736 = CIRCLE ( 'NONE', #26278, 1.499999999999999334 ) ;
#19737 = CARTESIAN_POINT ( 'NONE',  ( 113.0231681442453180, -10.15424416112534622, -14.75197769757730448 ) ) ;
#19738 = CARTESIAN_POINT ( 'NONE',  ( 109.4407702545248355, -10.62599879583958717, -15.77991374673208469 ) ) ;
#19739 = CARTESIAN_POINT ( 'NONE',  ( 116.0286950891469786, 2.331313199634366118, -19.89321520033831447 ) ) ;
#19740 = CARTESIAN_POINT ( 'NONE',  ( 113.6079577545248043, -7.250697342233347165, -7.631215200338321125 ) ) ;
#19741 = CARTESIAN_POINT ( 'NONE',  ( 120.6245414775786458, -9.988377603198976828, -10.36322818467138340 ) ) ;
#19742 = CARTESIAN_POINT ( 'NONE',  ( 121.9859814775786333, 0.2603800115204892296, -16.42320221600525088 ) ) ;
#19743 = CARTESIAN_POINT ( 'NONE',  ( 114.4620221536727485, 0.3967854368540359999, -10.50530088663808925 ) ) ;
#19744 = CARTESIAN_POINT ( 'NONE',  ( 117.3343948109119737, -3.383040157471821630, -19.15922257007629170 ) ) ;
#19745 = CARTESIAN_POINT ( 'NONE',  ( 112.8529881442453302, -1.561330072975668060, -17.79121239304076596 ) ) ;
#19746 = ORIENTED_EDGE ( 'NONE', *, *, #587, .F. ) ;
#19747 = CARTESIAN_POINT ( 'NONE',  ( 114.9518748109119883, -7.643976991954077427, -18.09477374809248928 ) ) ;
#19748 = EDGE_CURVE ( 'NONE', #30875, #15493, #36932, .T. ) ;
#19749 = CARTESIAN_POINT ( 'NONE',  ( 113.0231681442453180, -10.15424416112533912, -14.75197769757731336 ) ) ;
#19750 = AXIS2_PLACEMENT_3D ( 'NONE', #38509, #7286, #24405 ) ;
#19751 = CARTESIAN_POINT ( 'NONE',  ( 120.9649014775786355, -3.383040157471821630, -19.15922257007629170 ) ) ;
#19752 = CARTESIAN_POINT ( 'NONE',  ( 125.3895814775786448, -2.084020599724406786, -8.691656652584148546 ) ) ;
#19753 = CARTESIAN_POINT ( 'NONE',  ( 112.3991748109119868, -1.833838273342658809, -17.42832698103878286 ) ) ;
#19754 = ORIENTED_EDGE ( 'NONE', *, *, #19789, .T. ) ;
#19755 = AXIS2_PLACEMENT_3D ( 'NONE', #21892, #685, #31697 ) ;
#19756 = EDGE_CURVE ( 'NONE', #22801, #24842, #18685, .T. ) ;
#19757 = CARTESIAN_POINT ( 'NONE',  ( 117.1642148109119859, -0.8288870151387760510, -10.36305467784173118 ) ) ;
#19758 = CARTESIAN_POINT ( 'NONE',  ( 125.7299414775786346, 0.9020085738987339008, -11.91225656197089222 ) ) ;
#19759 = EDGE_CURVE ( 'NONE', #17628, #41162, #17684, .T. ) ;
#19760 = ADVANCED_FACE ( 'NONE', ( #15258 ), #28505, .T. ) ;
#19761 = CARTESIAN_POINT ( 'NONE',  ( 107.7738952545248310, 0.8980012041604421569, -11.00651665394454071 ) ) ;
#19762 = CARTESIAN_POINT ( 'NONE',  ( 118.6958348109119754, -3.505236298600246325, -18.68346056562440793 ) ) ;
#19763 = CARTESIAN_POINT ( 'NONE',  ( 123.9832704359119759, 0.5245030254254422486, -13.89657392289357141 ) ) ;
#19764 = DIRECTION ( 'NONE',  ( -0.000000000000000000, -0.9284778069183721172, -0.3713878862591650232 ) ) ;
#19765 = VERTEX_POINT ( 'NONE', #39434 ) ;
#19766 = CARTESIAN_POINT ( 'NONE',  ( 122.6604860609119640, -3.387241619883791355, -18.17469012370385073 ) ) ;
#19767 = CARTESIAN_POINT ( 'NONE',  ( 123.2339681442453241, -6.344957434206665248, -7.627207830600338134 ) ) ;
#19768 = DIRECTION ( 'NONE',  ( 0.000000000000000000, 0.4669533266896289669, 0.8842819633428518067 ) ) ;
#19769 = AXIS2_PLACEMENT_3D ( 'NONE', #27011, #30656, #23832 ) ;
#19770 = CARTESIAN_POINT ( 'NONE',  ( 122.7993923109119692, -9.959231468620748373, -10.70263013195265955 ) ) ;
#19771 = CARTESIAN_POINT ( 'NONE',  ( 75.95778847736514194, -3.256761025687008537, -16.39321520033831447 ) ) ;
#19772 =( BOUNDED_CURVE ( )  B_SPLINE_CURVE ( 2, ( #30397, #22647, #1663, #40895, #12170 ),
 .UNSPECIFIED., .F., .T. ) 
 B_SPLINE_CURVE_WITH_KNOTS ( ( 3, 2, 3 ),
 ( 0.000000000000000000, 0.1250000000000000000, 0.2257267493207365250 ),
 .UNSPECIFIED. ) 
 CURVE ( )  GEOMETRIC_REPRESENTATION_ITEM ( )  RATIONAL_B_SPLINE_CURVE ( ( 1.000000000000000000, 0.9238795325112869605, 1.000000000000000000, 0.9386610620246970127, 0.9761776733140110629 ) ) 
 REPRESENTATION_ITEM ( '' )  );
#19773 = CARTESIAN_POINT ( 'NONE',  ( 108.9545983795247821, -8.402594152722688392, -16.93181055722141792 ) ) ;
#19774 = DIRECTION ( 'NONE',  ( -0.1736481776669309696, -0.9848077530122079093, 0.000000000000000000 ) ) ;
#19775 = CARTESIAN_POINT ( 'NONE',  ( 122.6604860609119640, -3.387241619883791355, -18.17469012370385073 ) ) ;
#19776 = CIRCLE ( 'NONE', #33587, 4.500000000000003553 ) ;
#19777 = CARTESIAN_POINT ( 'NONE',  ( 125.0969017241875321, -2.474500861266701435, -17.82417889551932788 ) ) ;
#19778 = CARTESIAN_POINT ( 'NONE',  ( 123.9138173109119663, -0.4425889791248522331, -15.72798183378621140 ) ) ;
#19779 = CARTESIAN_POINT ( 'NONE',  ( 117.6180281442453150, -8.899110576539710493, -16.42337572283490132 ) ) ;
#19780 = CARTESIAN_POINT ( 'NONE',  ( 119.7434548109119845, -1.978546973019726263, -18.09349220968092098 ) ) ;
#19781 = ORIENTED_EDGE ( 'NONE', *, *, #4309, .T. ) ;
#19782 = CARTESIAN_POINT ( 'NONE',  ( 122.5532481442453019, -10.63000616557722466, -14.87417383870573495 ) ) ;
#19783 = CARTESIAN_POINT ( 'NONE',  ( 115.0086014775786509, -4.089484607189486809, -7.948022111789456723 ) ) ;
#19784 = CARTESIAN_POINT ( 'NONE',  ( 116.1082702545247827, 0.1403307496149616695, -11.32035403202665336 ) ) ;
#19785 = CARTESIAN_POINT ( 'NONE',  ( 112.3424481442453384, -3.505236298600246325, -18.68346056562440793 ) ) ;
#19786 = CARTESIAN_POINT ( 'NONE',  ( 123.8012348109119642, -9.565557343593413364, -10.61323700422348004 ) ) ;
#19787 = CARTESIAN_POINT ( 'NONE',  ( 122.3830681442452857, -8.166667518702819706, -8.995218007635861213 ) ) ;
#19788 = CARTESIAN_POINT ( 'NONE',  ( 114.6497546295247929, -4.863998795839590272, -7.631215200338315796 ) ) ;
#19789 = EDGE_CURVE ( 'NONE', #19947, #873, #27164, .T. ) ;
#19790 = CARTESIAN_POINT ( 'NONE',  ( 108.7462390045248242, -9.868328341294098749, -11.32035403202665869 ) ) ;
#19791 = CARTESIAN_POINT ( 'NONE',  ( 124.6127514966337060, -12.64971312686726712, -14.42062521576453626 ) ) ;
#19792 = CARTESIAN_POINT ( 'NONE',  ( 118.4689281442453392, -10.15424416112533912, -14.75197769757731336 ) ) ;
#19793 = CARTESIAN_POINT ( 'NONE',  ( 115.6325948109119821, -9.565557343593413364, -10.61323700422348004 ) ) ;
#19794 = FACE_OUTER_BOUND ( 'NONE', #6697, .T. ) ;
#19795 = CARTESIAN_POINT ( 'NONE',  ( 115.6220983795247861, -8.402594152722688392, -16.93181055722141792 ) ) ;
#19796 = ORIENTED_EDGE ( 'NONE', *, *, #25029, .T. ) ;
#19797 = FACE_OUTER_BOUND ( 'NONE', #13285, .T. ) ;
#19798 = CARTESIAN_POINT ( 'NONE',  ( 111.7184548109119788, -9.261995988541697145, -16.69588392320189030 ) ) ;
#19799 = CARTESIAN_POINT ( 'NONE',  ( 120.7852516859119731, -0.6942167230862511529, -9.935906262978006609 ) ) ;
#19800 = CARTESIAN_POINT ( 'NONE',  ( 119.3961891859119930, -1.406689858478933353, -17.56299727309130887 ) ) ;
#19801 = ORIENTED_EDGE ( 'NONE', *, *, #25156, .T. ) ;
#19802 = CARTESIAN_POINT ( 'NONE',  ( 123.5967000642937421, -3.159363131617086484, -14.41422705066527854 ) ) ;
#19803 = DIRECTION ( 'NONE',  ( 1.000000000000000000, 0.000000000000000000, -0.000000000000000000 ) ) ;
#19804 = ORIENTED_EDGE ( 'NONE', *, *, #9439, .F. ) ;
#19805 = CARTESIAN_POINT ( 'NONE',  ( 119.4332814775786318, -0.4660016031367893996, -10.09054647747474043 ) ) ;
#19806 = CIRCLE ( 'NONE', #15438, 2.000000000000000444 ) ;
#19807 = CARTESIAN_POINT ( 'NONE',  ( 123.2339681442453241, -3.505236298600246325, -18.68346056562440793 ) ) ;
#19808 = CARTESIAN_POINT ( 'NONE',  ( 112.9664414775786412, -9.859900752359374465, -12.68260735090039404 ) ) ;
#19809 = FACE_OUTER_BOUND ( 'NONE', #20616, .T. ) ;
#19810 = CARTESIAN_POINT ( 'NONE',  ( 123.5176014775786228, -9.261995988541697145, -16.69588392320189030 ) ) ;
#19811 = CARTESIAN_POINT ( 'NONE',  ( 114.7816948109119863, 0.5811942927096154232, -14.16772938898807155 ) ) ;
#19812 = EDGE_CURVE ( 'NONE', #41036, #20548, #897, .T. ) ;
#19813 = CARTESIAN_POINT ( 'NONE',  ( 110.0658483795247804, -8.402594152722688392, -16.93181055722141792 ) ) ;
#19814 = AXIS2_PLACEMENT_3D ( 'NONE', #21189, #31223, #31544 ) ;
#19815 = CARTESIAN_POINT ( 'NONE',  ( 125.4463081442452932, -5.638512984488999180, -18.83840828888717311 ) ) ;
#19816 = CARTESIAN_POINT ( 'NONE',  ( 151.2860562277021472, -1.889072916127989776, -18.60376373290417362 ) ) ;
#19817 = VERTEX_POINT ( 'NONE', #10947 ) ;
#19818 = ADVANCED_FACE ( 'NONE', ( #14587 ), #35199, .T. ) ;
#19819 = CARTESIAN_POINT ( 'NONE',  ( 113.8740681442453138, 0.5811942927096154232, -14.16772938898807155 ) ) ;
#19820 = CARTESIAN_POINT ( 'NONE',  ( 113.4202548109119846, 0.1319031606808879209, -14.10382304977623669 ) ) ;
#19821 = CARTESIAN_POINT ( 'NONE',  ( 75.95778847736481509, -3.256761025687722189, -7.993215200338315007 ) ) ;
#19822 = CARTESIAN_POINT ( 'NONE',  ( 112.7395348109119766, -5.638512984488999180, -18.83840828888717311 ) ) ;
#19823 = VERTEX_POINT ( 'NONE', #16393 ) ;
#19824 = CARTESIAN_POINT ( 'NONE',  ( 121.1350814775786233, 0.5811942927096110934, -14.16772938898807510 ) ) ;
#19825 = FACE_OUTER_BOUND ( 'NONE', #33298, .T. ) ;
#19826 = CARTESIAN_POINT ( 'NONE',  ( 119.7434548109119703, -2.613043214085062793, -8.928554074455437473 ) ) ;
#19827 = FACE_OUTER_BOUND ( 'NONE', #34707, .T. ) ;
#19828 = CARTESIAN_POINT ( 'NONE',  ( 114.4413348109119823, -0.8288870151387760510, -10.36305467784173118 ) ) ;
#19829 = CARTESIAN_POINT ( 'NONE',  ( 123.4772435044479124, -4.053804398456810176, -15.72110060669333187 ) ) ;
#19830 = AXIS2_PLACEMENT_3D ( 'NONE', #33912, #13196, #30736 ) ;
#19831 = CARTESIAN_POINT ( 'NONE',  ( 115.3489614775786407, -0.8288870151387760510, -10.36305467784173118 ) ) ;
#19832 = CARTESIAN_POINT ( 'NONE',  ( 68.56885555382550024, -20.41671115022304406, -19.39321520033831447 ) ) ;
#19833 = CONICAL_SURFACE ( 'NONE', #3104, 2.445500000000004448, 0.9599310885968757034 ) ;
#19834 = CARTESIAN_POINT ( 'NONE',  ( 125.1986466278897154, -1.893713009889057552, -20.10971988540413236 ) ) ;
#19835 = CARTESIAN_POINT ( 'NONE',  ( 114.2711548109119803, -0.1624402480850797581, -16.17319339645315424 ) ) ;
#19836 = CARTESIAN_POINT ( 'NONE',  ( 117.2209414775786485, -7.893985811506177619, -18.51759400769804742 ) ) ;
#19837 = CARTESIAN_POINT ( 'NONE',  ( 124.6746266859119743, -9.033780868592240054, -16.85052413769862056 ) ) ;
#19838 = CARTESIAN_POINT ( 'NONE',  ( 112.3991748109119868, -8.166667518702817929, -8.995218007635859436 ) ) ;
#19839 = CARTESIAN_POINT ( 'NONE',  ( 115.6325948109119821, -9.565557343593413364, -10.61323700422348004 ) ) ;
#19840 = CARTESIAN_POINT ( 'NONE',  ( 124.3117748109119844, -10.30919188438810075, -12.61870101168855918 ) ) ;
#19841 = CARTESIAN_POINT ( 'NONE',  ( 122.4965214775786251, -10.30919188438810075, -12.61870101168855918 ) ) ;
#19842 = VERTEX_POINT ( 'NONE', #36444 ) ;
#19843 = CARTESIAN_POINT ( 'NONE',  ( 111.8886348109120092, -3.383040157471821630, -19.15922257007629170 ) ) ;
#19844 = CARTESIAN_POINT ( 'NONE',  ( 113.1217858795247935, -0.7896495226426338832, -17.46756447353520159 ) ) ;
#19845 = CARTESIAN_POINT ( 'NONE',  ( 89.40092984481313465, -25.99489077589524300, -13.39321520033831625 ) ) ;
#19846 = VECTOR ( 'NONE', #16404, 1000.000000000000114 ) ;
#19847 = CARTESIAN_POINT ( 'NONE',  ( 122.6009548109119720, -2.421111938423274879, -5.775321541204940345 ) ) ;
#19848 = DIRECTION ( 'NONE',  ( 1.000000000000000000, 0.000000000000000000, -0.000000000000000000 ) ) ;
#19849 = CARTESIAN_POINT ( 'NONE',  ( 118.9794681442453026, -9.261995988541697145, -16.69588392320189030 ) ) ;
#19850 = VERTEX_POINT ( 'NONE', #29393 ) ;
#19851 = CARTESIAN_POINT ( 'NONE',  ( 125.6164881442453094, 0.2603800115204892296, -16.42320221600525088 ) ) ;
#19852 = CARTESIAN_POINT ( 'NONE',  ( 87.44708369096657918, -21.99489077589588604, -18.39321520033831803 ) ) ;
#19853 = CARTESIAN_POINT ( 'NONE',  ( 114.2711548109119803, -0.1624402480850797581, -16.17319339645315424 ) ) ;
#19854 = CARTESIAN_POINT ( 'NONE',  ( 104.9263171295248327, 0.1403307496149613920, -13.39321520033831447 ) ) ;
#19855 = EDGE_CURVE ( 'NONE', #12781, #9608, #29337, .T. ) ;
#19856 = CARTESIAN_POINT ( 'NONE',  ( 119.7169148109119874, -9.988377603198976828, -10.36322818467138340 ) ) ;
#19857 = CARTESIAN_POINT ( 'NONE',  ( 114.6497546295247929, -4.863998795839590272, -18.39754474579285315 ) ) ;
#19858 = CARTESIAN_POINT ( 'NONE',  ( 119.4219993335884311, -2.334846009198419559, -18.01015021110789505 ) ) ;
#19859 = ORIENTED_EDGE ( 'NONE', *, *, #30017, .T. ) ;
#19860 = DIRECTION ( 'NONE',  ( 0.000000000000000000, 0.000000000000000000, 1.000000000000000000 ) ) ;
#19861 = CARTESIAN_POINT ( 'NONE',  ( 122.7234281442452755, -4.153390946401325223, -8.397313243818185668 ) ) ;
#19862 = CARTESIAN_POINT ( 'NONE',  ( 119.6034614775786196, -6.344957434206665248, -7.627207830600338134 ) ) ;
#19863 = CARTESIAN_POINT ( 'NONE',  ( 112.2289948109119848, -7.643976991954077427, -18.09477374809248928 ) ) ;
#19864 =( BOUNDED_CURVE ( )  B_SPLINE_CURVE ( 2, ( #22821, #15989, #33510, #33061, #5483, #9146, #19403, #5039, #33290, #2065, #18953, #32844, #16219, #1612, #29893, #15533, #12576 ),
 .UNSPECIFIED., .F., .F. ) 
 B_SPLINE_CURVE_WITH_KNOTS ( ( 3, 2, 2, 2, 2, 2, 2, 2, 3 ),
 ( 0.6421282416568590001, 0.6484375000000000000, 0.6562500000000000000, 0.6640625000000000000, 0.6718750000000000000, 0.6796875000000000000, 0.6875000000000000000, 0.6953125000000000000, 0.7016217583431409999 ),
 .UNSPECIFIED. ) 
 CURVE ( )  GEOMETRIC_REPRESENTATION_ITEM ( )  RATIONAL_B_SPLINE_CURVE ( ( 0.9763430640195950305, 0.9385262470928690259, 1.000000000000000000, 0.9238795325112869605, 1.000000000000000000, 0.9238795325112869605, 1.000000000000000000, 0.9238795325112869605, 1.000000000000000000, 0.9238795325112869605, 1.000000000000000000, 0.9238795325112869605, 1.000000000000000000, 0.9238795325112869605, 1.000000000000000000, 0.9385262470928680267, 0.9763430640195970289 ) ) 
 REPRESENTATION_ITEM ( '' )  );
#19865 = CARTESIAN_POINT ( 'NONE',  ( 114.3278814775786429, -10.30919188438810075, -12.61870101168855918 ) ) ;
#19866 = LINE ( 'NONE', #22601, #23486 ) ;
#19867 = CARTESIAN_POINT ( 'NONE',  ( 126.2184548109105435, -0.8658195297460520301, -10.39078908864422246 ) ) ;
#19868 = CARTESIAN_POINT ( 'NONE',  ( 119.0929214775786278, -4.153390946401325223, -8.397313243818185668 ) ) ;
#19869 = ORIENTED_EDGE ( 'NONE', *, *, #13069, .F. ) ;
#19870 = CARTESIAN_POINT ( 'NONE',  ( 122.7993923109119692, -9.959231468620755479, -10.70263013195267199 ) ) ;
#19871 = ADVANCED_FACE ( 'NONE', ( #23232 ), #8646, .T. ) ;
#19872 = CARTESIAN_POINT ( 'NONE',  ( 113.7038881442453402, -3.383040157471821630, -19.15922257007629170 ) ) ;
#19873 = CARTESIAN_POINT ( 'NONE',  ( 121.4754414775786131, -1.833838273342659697, -17.42832698103878286 ) ) ;
#19874 = ORIENTED_EDGE ( 'NONE', *, *, #11421, .T. ) ;
#19875 = CARTESIAN_POINT ( 'NONE',  ( 124.6051735609119646, -9.645473719204776586, -14.86997237629376656 ) ) ;
#19876 = CARTESIAN_POINT ( 'NONE',  ( 118.7525614775786380, -8.166667518702819706, -8.995218007635861213 ) ) ;
#19877 = STYLED_ITEM ( 'NONE', ( #2924 ), #41161 ) ;
#19878 = CARTESIAN_POINT ( 'NONE',  ( 114.3024890045248156, 0.8980012041604421569, -15.77991374673208469 ) ) ;
#19879 = CARTESIAN_POINT ( 'NONE',  ( 117.4478481442453131, -9.565557343593413364, -10.61323700422348004 ) ) ;
#19880 = ORIENTED_EDGE ( 'NONE', *, *, #17775, .F. ) ;
#19881 = VECTOR ( 'NONE', #2367, 1000.000000000000000 ) ;
#19882 = ORIENTED_EDGE ( 'NONE', *, *, #40713, .T. ) ;
#19883 = CARTESIAN_POINT ( 'NONE',  ( 112.0020881442453344, 0.2603800115204892296, -16.42320221600525088 ) ) ;
#19884 = CARTESIAN_POINT ( 'NONE',  ( 120.3409081442453044, -8.899110576539710493, -16.42337572283490132 ) ) ;
#19885 = SURFACE_SIDE_STYLE ('',( #36739 ) ) ;
#19886 = ORIENTED_EDGE ( 'NONE', *, *, #30026, .F. ) ;
#19887 = CARTESIAN_POINT ( 'NONE',  ( 117.3343948109119737, -3.383040157471821630, -19.15922257007629170 ) ) ;
#19888 = CARTESIAN_POINT ( 'NONE',  ( 108.6767858795247861, -0.7896495226426338832, -17.46756447353520159 ) ) ;
#19889 = CARTESIAN_POINT ( 'NONE',  ( 121.4754414775786131, -8.166667518702819706, -8.995218007635861213 ) ) ;
#19891 = CARTESIAN_POINT ( 'NONE',  ( 118.1285681442453068, -2.084020599724406786, -8.691656652584148546 ) ) ;
#19890 = CARTESIAN_POINT ( 'NONE',  ( 113.5337081442453240, -9.261995988541697145, -16.69588392320189030 ) ) ;
#19892 = CARTESIAN_POINT ( 'NONE',  ( 124.1983214775786166, -1.833838273342659697, -17.42832698103878286 ) ) ;
#19893 = DIRECTION ( 'NONE',  ( 0.9609149988134837450, -0.1028163501681639419, 0.2570431154366518145 ) ) ;
#19894 = VERTEX_POINT ( 'NONE', #8421 ) ;
#19895 = CARTESIAN_POINT ( 'NONE',  ( 124.5386814775786206, -4.153390946401325223, -8.397313243818185668 ) ) ;
#19896 = CARTESIAN_POINT ( 'NONE',  ( 123.6770938145250227, -3.807985514183269693, -19.09877912889401230 ) ) ;
#19897 = CIRCLE ( 'NONE', #3868, 6.500000000000000888 ) ;
#19898 = DIRECTION ( 'NONE',  ( -0.9908103287288504424, 0.1352586133457950590, 0.000000000000000000 ) ) ;
#19899 = CARTESIAN_POINT ( 'NONE',  ( 108.1211608795247798, -8.938348069036489818, -9.318865927141430916 ) ) ;
#19900 = AXIS2_PLACEMENT_3D ( 'NONE', #3798, #6569, #34366 ) ;
#19901 = CARTESIAN_POINT ( 'NONE',  ( 111.2465515045248168, -6.936859964151250502, -18.39754474579286025 ) ) ;
#19902 = CARTESIAN_POINT ( 'NONE',  ( 112.7050671295247923, -10.62599879583958540, -13.39321520033831447 ) ) ;
#19903 = CARTESIAN_POINT ( 'NONE',  ( 122.7234281442452755, -5.638512984488999180, -18.83840828888717311 ) ) ;
#19904 = CARTESIAN_POINT ( 'NONE',  ( 124.7655881442452852, -9.859900752359378018, -12.68260735090039759 ) ) ;
#19905 = ORIENTED_EDGE ( 'NONE', *, *, #29473, .F. ) ;
#19906 = CARTESIAN_POINT ( 'NONE',  ( 124.9357681442453014, -1.834011780172310813, -8.268836392978581529 ) ) ;
#19907 = CARTESIAN_POINT ( 'NONE',  ( 113.8173414775786512, -9.565557343593413364, -10.61323700422348004 ) ) ;
#19908 = CARTESIAN_POINT ( 'NONE',  ( 121.4964260444391755, -1.267766418764731728, -16.93314635290706605 ) ) ;
#19909 = CARTESIAN_POINT ( 'NONE',  ( 120.3976348109119812, -1.834011780172310813, -8.268836392978581529 ) ) ;
#19910 = CARTESIAN_POINT ( 'NONE',  ( 119.9438214775786378, -7.893985811506177619, -18.51759400769804742 ) ) ;
#19911 = FACE_OUTER_BOUND ( 'NONE', #7806, .T. ) ;
#19912 = CARTESIAN_POINT ( 'NONE',  ( 124.9924948109119924, -5.574606645277164318, -18.38911715685844683 ) ) ;
#19913 = CARTESIAN_POINT ( 'NONE',  ( 68.07789357685331311, -68.58957386525776201, -38.44539312525988350 ) ) ;
#19914 = LINE ( 'NONE', #3250, #10984 ) ;
#19915 = EDGE_LOOP ( 'NONE', ( #41446, #27429, #7142, #24044, #20667, #19021, #40552, #24229, #14004, #31057, #28000 ) ) ;
#19916 = CARTESIAN_POINT ( 'NONE',  ( -2.700297285702341732, -7.094665554431733412, -7.444873403169903092 ) ) ;
#19917 = CARTESIAN_POINT ( 'NONE',  ( 112.2857214775786474, -5.574606645277164318, -18.38911715685844683 ) ) ;
#19918 = CARTESIAN_POINT ( 'NONE',  ( 122.7234281442452755, -4.153390946401325223, -8.397313243818185668 ) ) ;
#19919 = CARTESIAN_POINT ( 'NONE',  ( 108.6767858795247861, -8.402594152722688392, -9.854619843455216355 ) ) ;
#19920 = CARTESIAN_POINT ( 'NONE',  ( 110.6214733795247867, -1.325403438956436419, -9.854619843455211026 ) ) ;
#19921 = CARTESIAN_POINT ( 'NONE',  ( 116.4834948109119779, -7.894159318335828068, -9.358103419637847864 ) ) ;
#19922 = CARTESIAN_POINT ( 'NONE',  ( 70.64808409340794526, -25.00190304748438663, -5.469311635450234910 ) ) ;
#19923 = CARTESIAN_POINT ( 'NONE',  ( 117.3911214775786505, -7.894159318335828068, -9.358103419637847864 ) ) ;
#19924 = CARTESIAN_POINT ( 'NONE',  ( 123.0637881442452937, -0.4660016031367893996, -10.09054647747474043 ) ) ;
#19925 = ORIENTED_EDGE ( 'NONE', *, *, #796, .F. ) ;
#19926 = CARTESIAN_POINT ( 'NONE',  ( 123.5743281442453139, -2.084020599724406786, -8.691656652584148546 ) ) ;
#19927 = CARTESIAN_POINT ( 'NONE',  ( 117.5045748109119756, 0.5811942927096110934, -14.16772938898807510 ) ) ;
#19928 = CARTESIAN_POINT ( 'NONE',  ( 124.0281414775786146, -1.834011780172310813, -8.268836392978581529 ) ) ;
#19929 = ADVANCED_FACE ( 'NONE', ( #2018 ), #33461, .F. ) ;
#19930 = CARTESIAN_POINT ( 'NONE',  ( 124.7655881442452852, -9.859900752359378018, -12.68260735090039759 ) ) ;
#19931 = ORIENTED_EDGE ( 'NONE', *, *, #34052, .T. ) ;
#19932 = DIRECTION ( 'NONE',  ( 0.000000000000000000, 0.9284778069183720062, 0.3713878862591650232 ) ) ;
#19933 = CONICAL_SURFACE ( 'NONE', #10464, 0.4999999999999999445, 0.7853981633974476129 ) ;
#19934 = CARTESIAN_POINT ( 'NONE',  ( 122.7801548109119665, -3.383040157471821630, -19.15922257007629170 ) ) ;
#19935 = CARTESIAN_POINT ( 'NONE',  ( 114.8951481442453115, -8.899110576539710493, -16.42337572283490132 ) ) ;
#19936 = CARTESIAN_POINT ( 'NONE',  ( 111.8319081442453182, -4.153390946401321671, -8.397313243818183892 ) ) ;
#19937 = CARTESIAN_POINT ( 'NONE',  ( 108.4684265045247997, -7.250697342233347165, -19.15521520033831138 ) ) ;
#19938 = CARTESIAN_POINT ( 'NONE',  ( 121.6186891859119896, -1.406689858478933353, -17.56299727309130887 ) ) ;
#19939 = VERTEX_POINT ( 'NONE', #4989 ) ;
#19940 = DIRECTION ( 'NONE',  ( -0.9609149988134837450, 0.1028163501681639419, -0.2570431154366518145 ) ) ;
#19941 = CARTESIAN_POINT ( 'NONE',  ( 110.1353015045248469, -6.936859964151250502, -18.39754474579286025 ) ) ;
#19942 = CIRCLE ( 'NONE', #25766, 4.500000000000003553 ) ;
#19943 = CARTESIAN_POINT ( 'NONE',  ( 115.4137390045248566, -9.868328341294150263, -11.32035403202669777 ) ) ;
#19944 = CARTESIAN_POINT ( 'NONE',  ( 117.7314814775786260, -5.574606645277164318, -18.38911715685844683 ) ) ;
#19945 = CARTESIAN_POINT ( 'NONE',  ( 115.2355081442453155, 0.1319031606808879209, -14.10382304977623669 ) ) ;
#19946 = CARTESIAN_POINT ( 'NONE',  ( 126.7358418800189384, -6.436512518564030394, -18.41132298396161460 ) ) ;
#19947 = VERTEX_POINT ( 'NONE', #29843 ) ;
#19948 = DIRECTION ( 'NONE',  ( 0.000000000000000000, 0.000000000000000000, -1.000000000000000000 ) ) ;
#19949 = CARTESIAN_POINT ( 'NONE',  ( 118.2420214775786320, -6.222761293078241884, -8.102969835052219238 ) ) ;
#19950 = CARTESIAN_POINT ( 'NONE',  ( 113.5337081442453240, -0.8288870151387760510, -10.36305467784173118 ) ) ;
#19951 = CARTESIAN_POINT ( 'NONE',  ( 67.05591816083881440, -0.08547223048874456885, -10.39321520033831447 ) ) ;
#19952 = CARTESIAN_POINT ( 'NONE',  ( 111.4453614775786434, -1.861572684145083256, -17.39139446643145348 ) ) ;
#19954 = CARTESIAN_POINT ( 'NONE',  ( 122.4965214775786251, -10.30919188438810075, -12.61870101168855918 ) ) ;
#19953 = CARTESIAN_POINT ( 'NONE',  ( 114.0027383310706881, 0.1843591316377651834, -12.14321520033831625 ) ) ;
#19955 = CARTESIAN_POINT ( 'NONE',  ( 126.4673881442452910, -7.894159318335828068, -9.358103419637847864 ) ) ;
#19956 = ORIENTED_EDGE ( 'NONE', *, *, #33402, .T. ) ;
#19957 = CARTESIAN_POINT ( 'NONE',  ( 151.2860562277021472, -4.863998795839242995, -13.39321520033831447 ) ) ;
#19958 = FACE_OUTER_BOUND ( 'NONE', #24521, .T. ) ;
#19959 = CARTESIAN_POINT ( 'NONE',  ( 116.2471765045247594, -7.250697342233347165, -19.15521520033831138 ) ) ;
#19960 = CARTESIAN_POINT ( 'NONE',  ( 124.1983214775786166, -1.833838273342659697, -17.42832698103878286 ) ) ;
#19962 = CIRCLE ( 'NONE', #11240, 2.999999999999999556 ) ;
#19961 = CARTESIAN_POINT ( 'NONE',  ( 118.6391081442452986, -5.574606645277164318, -18.38911715685844683 ) ) ;
#19963 = DIRECTION ( 'NONE',  ( 0.000000000000000000, -0.4669533266896281343, -0.8842819633428521398 ) ) ;
#19964 = CARTESIAN_POINT ( 'NONE',  ( 115.4137390045248566, -9.868328341294098749, -11.32035403202665869 ) ) ;
#19965 = LINE ( 'NONE', #23163, #1145 ) ;
#19966 = LINE ( 'NONE', #41180, #33998 ) ;
#19967 = CARTESIAN_POINT ( 'NONE',  ( 114.7816948109119863, -9.859900752359374465, -12.68260735090039404 ) ) ;
#19968 = CARTESIAN_POINT ( 'NONE',  ( 110.3436608795247764, -8.938348069036489818, -9.318865927141430916 ) ) ;
#19969 = LINE ( 'NONE', #13807, #25543 ) ;
#19970 = CARTESIAN_POINT ( 'NONE',  ( 112.2883483795247770, -0.7896495226426338832, -9.318865927141430916 ) ) ;
#19971 = DIRECTION ( 'NONE',  ( 0.000000000000000000, 0.000000000000000000, -1.000000000000000000 ) ) ;
#19972 = CARTESIAN_POINT ( 'NONE',  ( 122.1561614775786353, -0.4660016031367893996, -10.09054647747474043 ) ) ;
#19973 = CARTESIAN_POINT ( 'NONE',  ( 116.2659068881580708, -12.01880880694303855, -4.893215200338314474 ) ) ;
#19974 = CARTESIAN_POINT ( 'NONE',  ( 120.7379948109119709, -10.63000616557722466, -14.87417383870573495 ) ) ;
#19975 = CARTESIAN_POINT ( 'NONE',  ( 112.9664414775786412, 0.5811942927096154232, -14.16772938898807155 ) ) ;
#19976 = ORIENTED_EDGE ( 'NONE', *, *, #29317, .F. ) ;
#19977 = CARTESIAN_POINT ( 'NONE',  ( 112.6260814775786514, -0.8288870151387760510, -10.36305467784173118 ) ) ;
#19978 = CARTESIAN_POINT ( 'NONE',  ( 112.7395348109119766, -4.153390946401321671, -8.397313243818183892 ) ) ;
#19979 = CARTESIAN_POINT ( 'NONE',  ( 122.7801548109119665, -3.383040157471821630, -19.15922257007629170 ) ) ;
#19980 = CARTESIAN_POINT ( 'NONE',  ( 115.2922348109119781, -10.63000616557722466, -14.87417383870573495 ) ) ;
#19981 = CARTESIAN_POINT ( 'NONE',  ( 113.0231681442453180, -10.15424416112533912, -14.75197769757731336 ) ) ;
#19982 = ORIENTED_EDGE ( 'NONE', *, *, #26825, .T. ) ;
#19983 = CARTESIAN_POINT ( 'NONE',  ( 118.4122014775786340, -9.859900752359374465, -12.68260735090039404 ) ) ;
#19984 = CARTESIAN_POINT ( 'NONE',  ( 115.8027748109119841, -8.899110576539710493, -16.42337572283490132 ) ) ;
#19985 = ADVANCED_FACE ( 'NONE', ( #19809 ), #191, .T. ) ;
#19986 = CARTESIAN_POINT ( 'NONE',  ( 107.9822546295247889, -4.863998795839590272, -7.631215200338315796 ) ) ;
#19987 = PRESENTATION_LAYER_ASSIGNMENT (  '', '', ( #13452 ) ) ;
#19988 = CARTESIAN_POINT ( 'NONE',  ( 112.2188952545247531, -9.868328341294098749, -15.46607636864997204 ) ) ;
#19989 = CARTESIAN_POINT ( 'NONE',  ( 122.5532481442453019, 0.4262465694468514643, -12.03445270309931736 ) ) ;
#19990 = CARTESIAN_POINT ( 'NONE',  ( 70.19189222814998175, -60.21979223295905825, -40.52181113153821457 ) ) ;
#19991 = CARTESIAN_POINT ( 'NONE',  ( 124.2166073908105801, -2.443475742715335741, -17.86549347949429389 ) ) ;
#19992 = VERTEX_POINT ( 'NONE', #22999 ) ;
#19993 = B_SPLINE_CURVE_WITH_KNOTS ( 'NONE', 3,
 ( #8048, #21279, #31536, #38587, #14894, #979, #28134, #13996, #28805, #18087, #24482, #4395, #24699, #42714, #744, #31980, #21506, #14666, #27913, #42490, #7365, #28582, #3719, #31310, #35394, #24927, #3941, #34932, #11251, #35164, #11481, #17639, #3502, #14442, #34718, #41824 ),
 .UNSPECIFIED., .F., .F.,
 ( 4, 2, 2, 2, 2, 1, 2, 2, 2, 2, 2, 2, 2, 1, 2, 2, 2, 2, 4 ),
 ( 0.000000000000000000, 0.06249999999998848144, 0.1249999999999769629, 0.1874999999999654443, 0.2187499999999629463, 0.2343749999999588385, 0.2421874999999513445, 0.2499999999999438505, 0.3749999999999300004, 0.4999999999999161782, 0.6249999999999023004, 0.6874999999998954170, 0.7187499999998919753, 0.7343749999998853140, 0.7421874999998818723, 0.7499999999998784306, 0.8124999999999107381, 0.8749999999999430456, 1.000000000000000000 ),
 .UNSPECIFIED. ) ;
#19994 = AXIS2_PLACEMENT_3D ( 'NONE', #34827, #44915, #10034 ) ;
#19995 = CARTESIAN_POINT ( 'NONE',  ( 123.6328298109119714, -7.200787124940443817, -17.81845355600750835 ) ) ;
#19996 = ADVANCED_FACE ( 'NONE', ( #36891 ), #40333, .T. ) ;
#19997 = CARTESIAN_POINT ( 'NONE',  ( 125.1626748109119802, -9.988377603198980381, -10.36322818467138518 ) ) ;
#19998 = CARTESIAN_POINT ( 'NONE',  ( 70.19189222814998175, -58.54852247098141049, -36.62221405200617141 ) ) ;
#19999 = CARTESIAN_POINT ( 'NONE',  ( 112.4559014775786494, -9.988377603198976828, -10.36322818467138340 ) ) ;
#20000 = CARTESIAN_POINT ( 'NONE',  ( 123.0385396737536752, -8.611453504372539314, -17.77011218421760574 ) ) ;
#20001 = CARTESIAN_POINT ( 'NONE',  ( 114.1889176093651912, 0.5600166689815611054, -14.64321520033831447 ) ) ;
#20002 = CARTESIAN_POINT ( 'NONE',  ( 106.1070202545248407, 0.1403307496149616695, -11.32035403202665336 ) ) ;
#20003 = DIRECTION ( 'NONE',  ( 0.9609149988134843001, -0.1028163501681632064, 0.2570431154366505933 ) ) ;
#20004 = CARTESIAN_POINT ( 'NONE',  ( 137.5146286042878785, -5.394418022101637789, -18.36369670353648687 ) ) ;
#20005 = DIRECTION ( 'NONE',  ( 1.000000000000000000, 0.000000000000000000, 0.000000000000000000 ) ) ;
#20006 = CARTESIAN_POINT ( 'NONE',  ( 125.7299414775786346, 0.9020085738987339008, -11.91225656197089222 ) ) ;
#20007 = CARTESIAN_POINT ( 'NONE',  ( 120.0005481442453146, -4.153390946401325223, -8.397313243818185668 ) ) ;
#20008 = CARTESIAN_POINT ( 'NONE',  ( 138.2184548109119930, 0.8652765085452543969, -12.77968882490997338 ) ) ;
#20009 = EDGE_CURVE ( 'NONE', #27061, #14735, #32792, .T. ) ;
#20010 = ORIENTED_EDGE ( 'NONE', *, *, #33178, .F. ) ;
#20011 = CARTESIAN_POINT ( 'NONE',  ( 122.7801548109119665, -3.383040157471821630, -19.15922257007629170 ) ) ;
#20012 = CARTESIAN_POINT ( 'NONE',  ( 120.7947214775786193, -9.261995988541697145, -16.69588392320189030 ) ) ;
#20013 = CARTESIAN_POINT ( 'NONE',  ( 125.6732148109119862, 0.5811942927096110934, -14.16772938898807510 ) ) ;
#20014 = CARTESIAN_POINT ( 'NONE',  ( 113.3635281442453504, -0.1624402480850797581, -16.17319339645315424 ) ) ;
#20015 = EDGE_CURVE ( 'NONE', #2361, #42481, #9098, .T. ) ;
#20016 = EDGE_CURVE ( 'NONE', #26194, #24134, #39659, .T. ) ;
#20017 = CARTESIAN_POINT ( 'NONE',  ( 114.1577014775786552, -6.344957434206662583, -7.627207830600332805 ) ) ;
#20018 = CARTESIAN_POINT ( 'NONE',  ( 124.3117748109119844, -10.30919188438810075, -12.61870101168855918 ) ) ;
#20019 = CARTESIAN_POINT ( 'NONE',  ( 110.6214733795247867, -8.938348069036489818, -17.46756447353520159 ) ) ;
#20020 = CARTESIAN_POINT ( 'NONE',  ( 106.8710046295248759, -4.863998795839590272, -18.39754474579285315 ) ) ;
#20021 = CARTESIAN_POINT ( 'NONE',  ( 82.73277184789131411, -31.78424552905355327, -23.09918304670232558 ) ) ;
#20022 = AXIS2_PLACEMENT_3D ( 'NONE', #20564, #10087, #40869 ) ;
#20023 = CARTESIAN_POINT ( 'NONE',  ( 116.9940348109119839, -0.1624402480850797581, -16.17319339645315424 ) ) ;
#20024 = CARTESIAN_POINT ( 'NONE',  ( 118.1852948109119836, -4.153390946401325223, -8.397313243818185668 ) ) ;
#20025 = CARTESIAN_POINT ( 'NONE',  ( 112.7965408578216824, 0.04929351793716424401, -12.14321520033834467 ) ) ;
#20026 = CARTESIAN_POINT ( 'NONE',  ( 114.3024890045248156, -9.868328341294098749, -11.32035403202665869 ) ) ;
#20027 = EDGE_LOOP ( 'NONE', ( #36927, #319, #7616, #10978 ) ) ;
#20028 = CARTESIAN_POINT ( 'NONE',  ( 109.2293626546097158, -0.7401772152451036035, -16.31465090027937137 ) ) ;
#20029 = CARTESIAN_POINT ( 'NONE',  ( 115.0086014775786509, -4.089484607189486809, -7.948022111789456723 ) ) ;
#20030 = CARTESIAN_POINT ( 'NONE',  ( 123.0133800025837019, -2.311015703046761072, -18.04188382666269774 ) ) ;
#20031 = CARTESIAN_POINT ( 'NONE',  ( 124.1190016859119680, -9.665098340737509730, -17.37397104707595474 ) ) ;
#20032 = CARTESIAN_POINT ( 'NONE',  ( 121.4103298109119748, -7.200787124940443817, -17.81845355600750835 ) ) ;
#20033 = ORIENTED_EDGE ( 'NONE', *, *, #19437, .T. ) ;
#20034 = CARTESIAN_POINT ( 'NONE',  ( 123.2184548109119788, -2.211393927326563702, -15.67656524173425758 ) ) ;
#20035 = CIRCLE ( 'NONE', #20741, 1.610000000000000986 ) ;
#20036 = CARTESIAN_POINT ( 'NONE',  ( 116.6056978591944642, -11.87337149029565175, -21.21309283736433571 ) ) ;
#20037 = ORIENTED_EDGE ( 'NONE', *, *, #41247, .T. ) ;
#20038 = CARTESIAN_POINT ( 'NONE',  ( 117.2776681442452968, -5.638512984488999180, -18.83840828888717311 ) ) ;
#20039 = CARTESIAN_POINT ( 'NONE',  ( 126.1270281442452870, 0.1319031606808879209, -14.10382304977623669 ) ) ;
#20040 = CARTESIAN_POINT ( 'NONE',  ( 117.8449348109119938, -1.833838273342659253, -17.42832698103878286 ) ) ;
#20041 = FILL_AREA_STYLE ('',( #37350 ) ) ;
#20042 = DIRECTION ( 'NONE',  ( 0.9908103287288505534, -0.1352586133457944206, 0.000000000000000000 ) ) ;
#20043 = CARTESIAN_POINT ( 'NONE',  ( 120.7947214775786193, -9.261995988541697145, -16.69588392320189030 ) ) ;
#20044 = CARTESIAN_POINT ( 'NONE',  ( 113.1933481442453058, -4.089484607189486809, -7.948022111789456723 ) ) ;
#20045 = EDGE_CURVE ( 'NONE', #22059, #16290, #32214, .T. ) ;
#20046 = CARTESIAN_POINT ( 'NONE',  ( 113.8857702545248003, 0.1403307496149616695, -11.32035403202665336 ) ) ;
#20047 = CARTESIAN_POINT ( 'NONE',  ( 126.0703014775786102, -9.988377603198980381, -10.36322818467138518 ) ) ;
#20048 = ORIENTED_EDGE ( 'NONE', *, *, #5411, .F. ) ;
#20049 =( BOUNDED_SURFACE ( )  B_SPLINE_SURFACE ( 1, 2, ( 
 ( #7194, #34981, #3112, #3767, #10856, #24751, #7412, #21332, #24099, #3991, #582, #6537, #20455, #44855, #37992, #6768, #11076, #8550, #7876, #24978, #36122, #32478, #1694, #4220, #15614, #38873, #18136, #7643, #39336, #39780, #42980, #1253, #1468, #25879, #25435, #18808, #11529, #22451, #28854, #14944, #21784, #29296, #29069, #8328, #19031, #11750, #15164, #29521, #4891, #11977, #18369, #21556, #1027, #36343, #35445, #801, #4666, #42767, #32032, #25658, #14719, #8104, #28631, #39563, #15393, #43209, #22004, #5114, #32699, #42539, #35900, #18588, #32918, #11300, #22227, #25209, #39107, #35674, #4449, #32258, #19265, #15846, #29741, #26329, #16067, #37246, #13106, #27009, #12201, #33595, #40929, #12428, #9681, #12659, #33367, #23598, #26556, #33144, #19707, #26786, #26099, #19941, #37019, #16301, #5789, #20178, #2829, #40236, #5564, #5348, #23140, #2370, #40695, #44347, #6257, #33830, #36571, #43652, #30202, #1916, #9003, #37484, #22902, #36795, #44121, #9449, #19484, #40470, #12887, #23363, #9230, #34062, #2137, #16757, #16529, #6018, #43437, #29973, #43889, #2599, #30428, #40004, #8769, #22675, #3281, #38159, #27241, #41825, #10585, #20840, #24483, #24047, #307, #24270, #85, #35165, #3720, #38372, #14220, #38588, #20402 ),
 ( #7145, #24700, #3942, #21056, #13337, #30654, #28136, #44572, #34933, #41387, #37717, #41156, #3503, #37940, #9917, #16986, #7366, #6715, #23830, #6487, #3059, #10363, #17640, #31537, #6934, #21280, #42043, #34719, #10141, #10804, #13997, #17420, #20626, #34286, #41604, #30878, #13779, #44798, #13556, #27466, #31095, #17203, #34502, #45021, #27690, #31311, #27914, #39284, #38824, #8050, #11482, #21954, #18763, #42491, #7593, #39512, #14667, #31762, #35845, #533, #745, #1420, #32653, #21508, #42715, #22402, #8500, #980, #39057, #4619, #29248, #4170, #28807, #31981, #43157, #1205, #15339, #25824, #28583, #11252, #18540, #15119, #25161, #14895, #32431, #29026, #25388, #11924, #18089, #36297, #36074, #42937, #17865, #4396, #35395, #11698, #18313, #22178, #39731, #35624, #32207, #25609, #14443, #8275, #4844, #28351, #42263, #7828, #11028, #24928, #21735, #9625, #23306, #12832, #19888, #13052, #39955, #23547, #5296, #23082, #26731, #36523, #44065, #44297, #5065, #40640, #32870, #18980, #2545, #1639, #16247, #15791, #12150, #15562, #36962, #12379, #29466, #19212, #26951, #43604, #43382, #26052, #22624, #29922, #30150, #9395, #12605, #40872, #37189, #43837, #29692, #5963, #33539, #5734, #26277, #33775, #16016, #16472, #33315, #30375, #8719 ) ),
 .UNSPECIFIED., .F., .F., .F. ) 
 B_SPLINE_SURFACE_WITH_KNOTS ( ( 2, 2 ),
 ( 3, 2, 2, 2, 2, 2, 2, 2, 2, 2, 2, 2, 2, 2, 2, 2, 2, 2, 2, 2, 2, 2, 2, 2, 2, 2, 2, 2, 2, 2, 2, 2, 2, 2, 2, 2, 2, 2, 2, 2, 2, 2, 2, 2, 2, 2, 2, 2, 2, 2, 2, 2, 2, 2, 2, 2, 2, 2, 2, 2, 2, 2, 2, 2, 2, 2, 2, 2, 2, 2, 2, 2, 2, 2, 2, 2, 2, 2, 2, 2, 3 ),
 ( 0.000000000000000000, 1.000000000000000000 ),
 ( 0.000000000000000000, 0.01250000000000000069, 0.02500000000000000139, 0.03749999999999999861, 0.05000000000000000278, 0.06250000000000000000, 0.07499999999999999722, 0.08749999999999999445, 0.1000000000000000056, 0.1125000000000000028, 0.1250000000000000000, 0.1375000000000000111, 0.1499999999999999944, 0.1625000000000000056, 0.1749999999999999889, 0.1875000000000000000, 0.2000000000000000111, 0.2124999999999999944, 0.2250000000000000056, 0.2374999999999999889, 0.2500000000000000000, 0.2625000000000000111, 0.2750000000000000222, 0.2874999999999999778, 0.2999999999999999889, 0.3125000000000000000, 0.3250000000000000111, 0.3375000000000000222, 0.3499999999999999778, 0.3624999999999999889, 0.3750000000000000000, 0.3875000000000000111, 0.4000000000000000222, 0.4124999999999999778, 0.4249999999999999889, 0.4375000000000000000, 0.4500000000000000111, 0.4625000000000000222, 0.4749999999999999778, 0.4874999999999999889, 0.5000000000000000000, 0.5124999999999999556, 0.5250000000000000222, 0.5374999999999999778, 0.5500000000000000444, 0.5625000000000000000, 0.5749999999999999556, 0.5875000000000000222, 0.5999999999999999778, 0.6125000000000000444, 0.6250000000000000000, 0.6374999999999999556, 0.6500000000000000222, 0.6624999999999999778, 0.6750000000000000444, 0.6875000000000000000, 0.6999999999999999556, 0.7125000000000000222, 0.7249999999999999778, 0.7375000000000000444, 0.7500000000000000000, 0.7624999999999999556, 0.7750000000000000222, 0.7874999999999999778, 0.8000000000000000444, 0.8125000000000000000, 0.8249999999999999556, 0.8375000000000000222, 0.8499999999999999778, 0.8625000000000000444, 0.8750000000000000000, 0.8874999999999999556, 0.9000000000000000222, 0.9124999999999999778, 0.9250000000000000444, 0.9375000000000000000, 0.9499999999999999556, 0.9625000000000000222, 0.9749999999999999778, 0.9875000000000000444, 1.000000000000000000 ),
 .UNSPECIFIED. ) 
 GEOMETRIC_REPRESENTATION_ITEM ( )  RATIONAL_B_SPLINE_SURFACE ( (
 ( 1.000000000000000000, 0.9238795325112869605, 1.000000000000000000, 0.9238795325112869605, 1.000000000000000000, 0.9238795325112869605, 1.000000000000000000, 0.9238795325112869605, 1.000000000000000000, 0.9238795325112869605, 1.000000000000000000, 0.9238795325112869605, 1.000000000000000000, 0.9238795325112869605, 1.000000000000000000, 0.9238795325112869605, 1.000000000000000000, 0.9238795325112869605, 1.000000000000000000, 0.9238795325112869605, 1.000000000000000000, 0.9238795325112869605, 1.000000000000000000, 0.9238795325112869605, 1.000000000000000000, 0.9238795325112869605, 1.000000000000000000, 0.9238795325112869605, 1.000000000000000000, 0.9238795325112869605, 1.000000000000000000, 0.9238795325112869605, 1.000000000000000000, 0.9238795325112869605, 1.000000000000000000, 0.9238795325112869605, 1.000000000000000000, 0.9238795325112869605, 1.000000000000000000, 0.9238795325112869605, 1.000000000000000000, 0.9238795325112869605, 1.000000000000000000, 0.9238795325112869605, 1.000000000000000000, 0.9238795325112869605, 1.000000000000000000, 0.9238795325112869605, 1.000000000000000000, 0.9238795325112869605, 1.000000000000000000, 0.9238795325112869605, 1.000000000000000000, 0.9238795325112869605, 1.000000000000000000, 0.9238795325112869605, 1.000000000000000000, 0.9238795325112869605, 1.000000000000000000, 0.9238795325112869605, 1.000000000000000000, 0.9238795325112869605, 1.000000000000000000, 0.9238795325112869605, 1.000000000000000000, 0.9238795325112869605, 1.000000000000000000, 0.9238795325112869605, 1.000000000000000000, 0.9238795325112869605, 1.000000000000000000, 0.9238795325112869605, 1.000000000000000000, 0.9238795325112869605, 1.000000000000000000, 0.9238795325112869605, 1.000000000000000000, 0.9238795325112869605, 1.000000000000000000, 0.9238795325112869605, 1.000000000000000000, 0.9238795325112869605, 1.000000000000000000, 0.9238795325112869605, 1.000000000000000000, 0.9238795325112869605, 1.000000000000000000, 0.9238795325112869605, 1.000000000000000000, 0.9238795325112869605, 1.000000000000000000, 0.9238795325112869605, 1.000000000000000000, 0.9238795325112869605, 1.000000000000000000, 0.9238795325112869605, 1.000000000000000000, 0.9238795325112869605, 1.000000000000000000, 0.9238795325112869605, 1.000000000000000000, 0.9238795325112869605, 1.000000000000000000, 0.9238795325112869605, 1.000000000000000000, 0.9238795325112869605, 1.000000000000000000, 0.9238795325112869605, 1.000000000000000000, 0.9238795325112869605, 1.000000000000000000, 0.9238795325112869605, 1.000000000000000000, 0.9238795325112869605, 1.000000000000000000, 0.9238795325112869605, 1.000000000000000000, 0.9238795325112869605, 1.000000000000000000, 0.9238795325112869605, 1.000000000000000000, 0.9238795325112869605, 1.000000000000000000, 0.9238795325112869605, 1.000000000000000000, 0.9238795325112869605, 1.000000000000000000, 0.9238795325112869605, 1.000000000000000000, 0.9238795325112869605, 1.000000000000000000, 0.9238795325112869605, 1.000000000000000000, 0.9238795325112869605, 1.000000000000000000, 0.9238795325112869605, 1.000000000000000000, 0.9238795325112869605, 1.000000000000000000, 0.9238795325112869605, 1.000000000000000000, 0.9238795325112869605, 1.000000000000000000, 0.9238795325112869605, 1.000000000000000000, 0.9238795325112869605, 1.000000000000000000, 0.9238795325112869605, 1.000000000000000000, 0.9238795325112869605, 1.000000000000000000, 0.9238795325112869605, 1.000000000000000000, 0.9238795325112869605, 1.000000000000000000, 0.9238795325112869605, 1.000000000000000000, 0.9238795325112869605, 1.000000000000000000, 0.9238795325112869605, 1.000000000000000000),
 ( 1.000000000000000000, 0.9238795325112869605, 1.000000000000000000, 0.9238795325112869605, 1.000000000000000000, 0.9238795325112869605, 1.000000000000000000, 0.9238795325112869605, 1.000000000000000000, 0.9238795325112869605, 1.000000000000000000, 0.9238795325112869605, 1.000000000000000000, 0.9238795325112869605, 1.000000000000000000, 0.9238795325112869605, 1.000000000000000000, 0.9238795325112869605, 1.000000000000000000, 0.9238795325112869605, 1.000000000000000000, 0.9238795325112869605, 1.000000000000000000, 0.9238795325112869605, 1.000000000000000000, 0.9238795325112869605, 1.000000000000000000, 0.9238795325112869605, 1.000000000000000000, 0.9238795325112869605, 1.000000000000000000, 0.9238795325112869605, 1.000000000000000000, 0.9238795325112869605, 1.000000000000000000, 0.9238795325112869605, 1.000000000000000000, 0.9238795325112869605, 1.000000000000000000, 0.9238795325112869605, 1.000000000000000000, 0.9238795325112869605, 1.000000000000000000, 0.9238795325112869605, 1.000000000000000000, 0.9238795325112869605, 1.000000000000000000, 0.9238795325112869605, 1.000000000000000000, 0.9238795325112869605, 1.000000000000000000, 0.9238795325112869605, 1.000000000000000000, 0.9238795325112869605, 1.000000000000000000, 0.9238795325112869605, 1.000000000000000000, 0.9238795325112869605, 1.000000000000000000, 0.9238795325112869605, 1.000000000000000000, 0.9238795325112869605, 1.000000000000000000, 0.9238795325112869605, 1.000000000000000000, 0.9238795325112869605, 1.000000000000000000, 0.9238795325112869605, 1.000000000000000000, 0.9238795325112869605, 1.000000000000000000, 0.9238795325112869605, 1.000000000000000000, 0.9238795325112869605, 1.000000000000000000, 0.9238795325112869605, 1.000000000000000000, 0.9238795325112869605, 1.000000000000000000, 0.9238795325112869605, 1.000000000000000000, 0.9238795325112869605, 1.000000000000000000, 0.9238795325112869605, 1.000000000000000000, 0.9238795325112869605, 1.000000000000000000, 0.9238795325112869605, 1.000000000000000000, 0.9238795325112869605, 1.000000000000000000, 0.9238795325112869605, 1.000000000000000000, 0.9238795325112869605, 1.000000000000000000, 0.9238795325112869605, 1.000000000000000000, 0.9238795325112869605, 1.000000000000000000, 0.9238795325112869605, 1.000000000000000000, 0.9238795325112869605, 1.000000000000000000, 0.9238795325112869605, 1.000000000000000000, 0.9238795325112869605, 1.000000000000000000, 0.9238795325112869605, 1.000000000000000000, 0.9238795325112869605, 1.000000000000000000, 0.9238795325112869605, 1.000000000000000000, 0.9238795325112869605, 1.000000000000000000, 0.9238795325112869605, 1.000000000000000000, 0.9238795325112869605, 1.000000000000000000, 0.9238795325112869605, 1.000000000000000000, 0.9238795325112869605, 1.000000000000000000, 0.9238795325112869605, 1.000000000000000000, 0.9238795325112869605, 1.000000000000000000, 0.9238795325112869605, 1.000000000000000000, 0.9238795325112869605, 1.000000000000000000, 0.9238795325112869605, 1.000000000000000000, 0.9238795325112869605, 1.000000000000000000, 0.9238795325112869605, 1.000000000000000000, 0.9238795325112869605, 1.000000000000000000, 0.9238795325112869605, 1.000000000000000000, 0.9238795325112869605, 1.000000000000000000, 0.9238795325112869605, 1.000000000000000000, 0.9238795325112869605, 1.000000000000000000, 0.9238795325112869605, 1.000000000000000000, 0.9238795325112869605, 1.000000000000000000, 0.9238795325112869605, 1.000000000000000000, 0.9238795325112869605, 1.000000000000000000, 0.9238795325112869605, 1.000000000000000000, 0.9238795325112869605, 1.000000000000000000, 0.9238795325112869605, 1.000000000000000000) ) ) 
 REPRESENTATION_ITEM ( '' )  SURFACE ( )  );
#20050 = CARTESIAN_POINT ( 'NONE',  ( 116.4834948109119779, -1.561330072975668504, -17.79121239304076951 ) ) ;
#20051 = ADVANCED_FACE ( 'NONE', ( #8868 ), #11116, .T. ) ;
#20052 = CARTESIAN_POINT ( 'NONE',  ( 114.9518748109119883, -7.643976991954077427, -18.09477374809248928 ) ) ;
#20053 = CARTESIAN_POINT ( 'NONE',  ( 126.3444272079631503, -5.154307014690458821, -18.44796746967900702 ) ) ;
#20054 = EDGE_CURVE ( 'NONE', #35629, #10759, #1649, .T. ) ;
#20055 = CARTESIAN_POINT ( 'NONE',  ( 113.2500748109119968, -6.344957434206662583, -7.627207830600332805 ) ) ;
#20056 = AXIS2_PLACEMENT_3D ( 'NONE', #20344, #2999, #16924 ) ;
#20057 = ORIENTED_EDGE ( 'NONE', *, *, #44280, .T. ) ;
#20058 = CARTESIAN_POINT ( 'NONE',  ( 121.7590748109119687, -7.893985811506177619, -18.51759400769804742 ) ) ;
#20059 = LINE ( 'NONE', #6824, #18691 ) ;
#20060 = CARTESIAN_POINT ( 'NONE',  ( 113.3068014775786594, -1.833838273342658809, -17.42832698103878286 ) ) ;
#20061 = DIRECTION ( 'NONE',  ( -0.000000000000000000, -0.9284778069183721172, -0.3713878862591650232 ) ) ;
#20062 = CARTESIAN_POINT ( 'NONE',  ( 66.58723489636778936, -20.14619392353143112, -10.89321520033831447 ) ) ;
#20063 = CARTESIAN_POINT ( 'NONE',  ( 117.2209414775786485, -2.084020599724406786, -8.691656652584148546 ) ) ;
#20064 = CARTESIAN_POINT ( 'NONE',  ( 112.8337832127138682, -2.191907684172563986, -18.20049396185734025 ) ) ;
#20065 = CARTESIAN_POINT ( 'NONE',  ( 116.8805814775786445, -3.505236298600246325, -18.68346056562440793 ) ) ;
#20066 = CARTESIAN_POINT ( 'NONE',  ( 87.02785693856107230, -24.14644159042263993, -12.62951656296512937 ) ) ;
#20067 = CARTESIAN_POINT ( 'NONE',  ( 116.5402214775786405, -9.565557343593413364, -10.61323700422348004 ) ) ;
#20068 = CARTESIAN_POINT ( 'NONE',  ( 116.8238548109119819, -4.089484607189486809, -7.948022111789456723 ) ) ;
#20069 = CARTESIAN_POINT ( 'NONE',  ( 122.3826735609119680, -9.645473719204776586, -14.86997237629376656 ) ) ;
#20070 = CARTESIAN_POINT ( 'NONE',  ( 125.4463081442452932, -4.153390946401325223, -8.397313243818185668 ) ) ;
#20071 = CARTESIAN_POINT ( 'NONE',  ( 116.1998614775786507, 0.4262465694468514643, -12.03445270309931736 ) ) ;
#20072 = CARTESIAN_POINT ( 'NONE',  ( 122.5532481442453019, -10.63000616557722466, -14.87417383870573495 ) ) ;
#20073 = EDGE_CURVE ( 'NONE', #36947, #18524, #32252, .T. ) ;
#20074 = CARTESIAN_POINT ( 'NONE',  ( 116.8238548109119819, -5.574606645277164318, -18.38911715685844683 ) ) ;
#20075 = ORIENTED_EDGE ( 'NONE', *, *, #12095, .T. ) ;
#20076 = CARTESIAN_POINT ( 'NONE',  ( 113.6471614775786492, -5.638512984488999180, -18.83840828888717311 ) ) ;
#20077 = CARTESIAN_POINT ( 'NONE',  ( 111.1770983795247787, -0.7896495226426338832, -9.318865927141430916 ) ) ;
#20078 = CARTESIAN_POINT ( 'NONE',  ( 105.6903015045248253, -6.936859964151250502, -18.39754474579286025 ) ) ;
#20079 = CARTESIAN_POINT ( 'NONE',  ( 105.8986608795248401, -1.325403438956436419, -16.93181055722141792 ) ) ;
#20080 = LINE ( 'NONE', #9360, #13850 ) ;
#20081 = CARTESIAN_POINT ( 'NONE',  ( 117.5613014775786525, 0.9020085738987339008, -11.91225656197089222 ) ) ;
#20082 = ORIENTED_EDGE ( 'NONE', *, *, #12252, .F. ) ;
#20083 = DIRECTION ( 'NONE',  ( 0.000000000000000000, 0.000000000000000000, -1.000000000000000000 ) ) ;
#20084 = CARTESIAN_POINT ( 'NONE',  ( 117.2294421295247844, -10.72535413672978599, -21.89321520033831447 ) ) ;
#20085 = EDGE_CURVE ( 'NONE', #35601, #1558, #22067, .T. ) ;
#20086 = CARTESIAN_POINT ( 'NONE',  ( 113.7038881442453402, -6.222761293078241884, -8.102969835052219238 ) ) ;
#20087 = CARTESIAN_POINT ( 'NONE',  ( 89.67401078471493747, -24.14644159042263993, -12.62951656296512937 ) ) ;
#20088 = CARTESIAN_POINT ( 'NONE',  ( 123.4608748109119745, -10.63000616557722466, -14.87417383870573495 ) ) ;
#20089 = CARTESIAN_POINT ( 'NONE',  ( 114.4413952545248350, -9.868328341294098749, -15.46607636864997204 ) ) ;
#20090 = CARTESIAN_POINT ( 'NONE',  ( 89.28374162313775741, -9.926294987500817513, -13.51696516463038833 ) ) ;
#20091 = AXIS2_PLACEMENT_3D ( 'NONE', #1087, #27795, #3825 ) ;
#20092 = ORIENTED_EDGE ( 'NONE', *, *, #11363, .F. ) ;
#20093 = CARTESIAN_POINT ( 'NONE',  ( 112.1722681442453222, -0.4660016031367893996, -10.09054647747474043 ) ) ;
#20094 = CARTESIAN_POINT ( 'NONE',  ( 123.7445081442452874, -7.894159318335828068, -9.358103419637847864 ) ) ;
#20095 = CARTESIAN_POINT ( 'NONE',  ( 119.5467348109119712, -4.089484607189486809, -7.948022111789456723 ) ) ;
#20096 = CARTESIAN_POINT ( 'NONE',  ( 113.6471614775786492, -4.153390946401321671, -8.397313243818183892 ) ) ;
#20097 = CARTESIAN_POINT ( 'NONE',  ( 116.4834948109119779, -1.561330072975668504, -17.79121239304076951 ) ) ;
#20098 = CARTESIAN_POINT ( 'NONE',  ( 69.69189222815028018, -41.76310523276638520, -7.393215200338315363 ) ) ;
#20099 = CARTESIAN_POINT ( 'NONE',  ( 126.5125895482200917, -1.167437683881369814, -9.811629287901746821 ) ) ;
#20100 = CARTESIAN_POINT ( 'NONE',  ( 119.6034614775786196, -3.505236298600246325, -18.68346056562440793 ) ) ;
#20101 = ORIENTED_EDGE ( 'NONE', *, *, #6114, .F. ) ;
#20102 = AXIS2_PLACEMENT_3D ( 'NONE', #3056, #16984, #30876 ) ;
#20103 = CARTESIAN_POINT ( 'NONE',  ( 119.4900081442453086, -1.834011780172310591, -8.268836392978581529 ) ) ;
#20104 = CARTESIAN_POINT ( 'NONE',  ( 111.9453614775786434, -1.561330072975668060, -17.79121239304076596 ) ) ;
#20105 = CARTESIAN_POINT ( 'NONE',  ( 121.5888948109119809, 0.1319031606808879209, -14.10382304977623669 ) ) ;
#20106 = EDGE_LOOP ( 'NONE', ( #18208, #38860, #18896, #44708 ) ) ;
#20107 = CARTESIAN_POINT ( 'NONE',  ( 122.8688454359119646, 0.5291689781388270175, -13.89700978578772705 ) ) ;
#20108 = CARTESIAN_POINT ( 'NONE',  ( 137.3527759848259961, -0.3567832970757958688, -10.86681561206427027 ) ) ;
#20109 = CARTESIAN_POINT ( 'NONE',  ( 118.2420214775786320, -3.383040157471821630, -19.15922257007629170 ) ) ;
#20110 = CARTESIAN_POINT ( 'NONE',  ( 113.4690515045247992, -2.477300249445798297, -7.631215200338321125 ) ) ;
#20111 = CARTESIAN_POINT ( 'NONE',  ( 114.6115148109119986, -6.222761293078241884, -8.102969835052219238 ) ) ;
#20112 = VERTEX_POINT ( 'NONE', #40565 ) ;
#20113 = VERTEX_POINT ( 'NONE', #37115 ) ;
#20114 = CARTESIAN_POINT ( 'NONE',  ( 126.2404814775786264, -0.8288870151387760510, -10.36305467784173118 ) ) ;
#20115 = CIRCLE ( 'NONE', #32457, 2.000000000000000444 ) ;
#20116 = CARTESIAN_POINT ( 'NONE',  ( 122.4397948109119767, -0.1624402480850797581, -16.17319339645315424 ) ) ;
#20117 = DIRECTION ( 'NONE',  ( 0.7962509850245451659, 0.6049664196031392382, 0.000000000000000000 ) ) ;
#20118 = ADVANCED_FACE ( 'NONE', ( #41473 ), #33707, .T. ) ;
#20119 = VERTEX_POINT ( 'NONE', #24139 ) ;
#20120 = CARTESIAN_POINT ( 'NONE',  ( 121.0783548109119749, 0.2603800115204892296, -16.42320221600525088 ) ) ;
#20121 = AXIS2_PLACEMENT_3D ( 'NONE', #10971, #36020, #21898 ) ;
#20122 = CARTESIAN_POINT ( 'NONE',  ( 112.1722681442453222, -8.899110576539710493, -16.42337572283490132 ) ) ;
#20123 = CARTESIAN_POINT ( 'NONE',  ( 120.4543614775786295, -4.089484607189486809, -7.948022111789456723 ) ) ;
#20125 = CARTESIAN_POINT ( 'NONE',  ( 119.6034614775786196, -3.505236298600246325, -18.68346056562440793 ) ) ;
#20124 = CARTESIAN_POINT ( 'NONE',  ( 119.1496481442453046, -3.383040157471821630, -19.15922257007629170 ) ) ;
#20126 = CARTESIAN_POINT ( 'NONE',  ( 124.1415948109119540, -3.505236298600246325, -18.68346056562440793 ) ) ;
#20127 = CARTESIAN_POINT ( 'NONE',  ( 112.4559014775786494, -9.988377603198976828, -10.36322818467138340 ) ) ;
#20128 = ORIENTED_EDGE ( 'NONE', *, *, #1616, .F. ) ;
#20129 = VECTOR ( 'NONE', #38512, 1000.000000000000000 ) ;
#20130 = CARTESIAN_POINT ( 'NONE',  ( 124.2550481442452792, -0.1624402480850797581, -16.17319339645315424 ) ) ;
#20131 = DIRECTION ( 'NONE',  ( 1.000000000000000000, 0.000000000000000000, 0.000000000000000000 ) ) ;
#20132 = DIRECTION ( 'NONE',  ( 0.6725995567522981000, 0.7400066460894877407, -0.000000000000000000 ) ) ;
#20133 = CARTESIAN_POINT ( 'NONE',  ( 110.0658483795247804, -0.7896495226426338832, -9.318865927141430916 ) ) ;
#20134 = CARTESIAN_POINT ( 'NONE',  ( 112.5661608795247872, -1.325403438956436419, -16.93181055722141792 ) ) ;
#20135 = CARTESIAN_POINT ( 'NONE',  ( 109.0240515045248202, -2.477300249445798297, -7.631215200338321125 ) ) ;
#20136 = B_SPLINE_CURVE_WITH_KNOTS ( 'NONE', 3,
 ( #9777, #20263, #9544, #6349, #41023, #44213, #37108, #13201, #23692, #16164 ),
 .UNSPECIFIED., .F., .F.,
 ( 4, 3, 3, 4 ),
 ( 0.000000000000000000, 1.701546542442319959E-05, 3.403093084891929823E-05, 6.554879158867139171E-05 ),
 .UNSPECIFIED. ) ;
#20137 = CARTESIAN_POINT ( 'NONE',  ( 120.9081748109119872, -5.638512984488999180, -18.83840828888717311 ) ) ;
#20138 = CARTESIAN_POINT ( 'NONE',  ( 121.3052614775786111, -7.643976991954077427, -18.09477374809248928 ) ) ;
#20139 =( BOUNDED_CURVE ( )  B_SPLINE_CURVE ( 2, ( #24072, #3305, #30679, #45043, #44823, #2853, #37276, #37740, #44148 ),
 .UNSPECIFIED., .F., .T. ) 
 B_SPLINE_CURVE_WITH_KNOTS ( ( 3, 2, 2, 2, 3 ),
 ( 0.1250000000000000000, 0.1562500000000000000, 0.1875000000000000000, 0.2187500000000000000, 0.2397292404589490000 ),
 .UNSPECIFIED. ) 
 CURVE ( )  GEOMETRIC_REPRESENTATION_ITEM ( )  RATIONAL_B_SPLINE_CURVE ( ( 1.000000000000000000, 0.9238795325112869605, 1.000000000000000000, 0.9238795325112869605, 1.000000000000000000, 0.9238795325112869605, 1.000000000000000000, 0.9488976130786129781, 0.9664089390052280626 ) ) 
 REPRESENTATION_ITEM ( '' )  );
#20140 = EDGE_LOOP ( 'NONE', ( #30925, #32470, #13192, #18760, #33088 ) ) ;
#20141 = CARTESIAN_POINT ( 'NONE',  ( 124.0848681442452772, -4.089484607189486809, -7.948022111789456723 ) ) ;
#20142 = CARTESIAN_POINT ( 'NONE',  ( 114.0442481442453300, -7.643976991954077427, -18.09477374809248928 ) ) ;
#20143 = CARTESIAN_POINT ( 'NONE',  ( 60.06931813437628875, -14.72076136720887085, -18.18301750815651374 ) ) ;
#20144 = EDGE_CURVE ( 'NONE', #25485, #33632, #14067, .T. ) ;
#20145 = CARTESIAN_POINT ( 'NONE',  ( 118.8092881442453290, -9.988377603198976828, -10.36322818467138340 ) ) ;
#20146 = CARTESIAN_POINT ( 'NONE',  ( 123.0070614775786169, 0.9020085738987339008, -11.91225656197089222 ) ) ;
#20147 = FACE_OUTER_BOUND ( 'NONE', #15077, .T. ) ;
#20148 = CARTESIAN_POINT ( 'NONE',  ( 114.2144281442453178, -8.166667518702817929, -8.995218007635859436 ) ) ;
#20149 = DIRECTION ( 'NONE',  ( -0.9908103287288504424, 0.1352586133457950590, 0.000000000000000000 ) ) ;
#20150 = ORIENTED_EDGE ( 'NONE', *, *, #5262, .T. ) ;
#20151 = CARTESIAN_POINT ( 'NONE',  ( 89.67401078471493747, -25.99489077589524300, -13.39321520033831447 ) ) ;
#20152 = CARTESIAN_POINT ( 'NONE',  ( 112.6828081442453282, -2.084020599724406786, -8.691656652584148546 ) ) ;
#20153 = CARTESIAN_POINT ( 'NONE',  ( 125.1059481442452750, -1.833838273342660141, -17.42832698103878286 ) ) ;
#20154 = CONICAL_SURFACE ( 'NONE', #1890, 0.8509999999999994236, 0.06981317007976593769 ) ;
#20155 = CARTESIAN_POINT ( 'NONE',  ( 107.7738952545248310, -9.868328341294098749, -15.46607636864997204 ) ) ;
#20156 = CARTESIAN_POINT ( 'NONE',  ( 110.0658483795247804, -8.402594152722688392, -16.93181055722141792 ) ) ;
#20157 = CARTESIAN_POINT ( 'NONE',  ( 119.0929214775786278, -4.153390946401325223, -8.397313243818185668 ) ) ;
#20158 = DIRECTION ( 'NONE',  ( 0.000000000000000000, 0.000000000000000000, -1.000000000000000000 ) ) ;
#20159 = CARTESIAN_POINT ( 'NONE',  ( 117.9583881442453048, 0.1319031606808879209, -14.10382304977623669 ) ) ;
#20160 = CARTESIAN_POINT ( 'NONE',  ( 124.3685014775786328, -10.63000616557722466, -14.87417383870573495 ) ) ;
#20161 = ORIENTED_EDGE ( 'NONE', *, *, #24744, .F. ) ;
#20162 = VECTOR ( 'NONE', #33427, 1000.000000000000227 ) ;
#20163 = CARTESIAN_POINT ( 'NONE',  ( 120.6245414775786458, -0.1624402480850797581, -16.17319339645315424 ) ) ;
#20164 = CARTESIAN_POINT ( 'NONE',  ( 119.9438214775786378, -7.893985811506177619, -18.51759400769804742 ) ) ;
#20165 = CARTESIAN_POINT ( 'NONE',  ( 123.5176014775786228, -9.261995988541697145, -16.69588392320189030 ) ) ;
#20166 = CARTESIAN_POINT ( 'NONE',  ( 125.1059481442452750, -1.833838273342660141, -17.42832698103878286 ) ) ;
#20167 = ORIENTED_EDGE ( 'NONE', *, *, #30914, .F. ) ;
#20168 = CARTESIAN_POINT ( 'NONE',  ( 121.3655035264548872, -8.247323210606168686, -17.08054893949881148 ) ) ;
#20169 = VECTOR ( 'NONE', #23935, 1000.000000000000000 ) ;
#20170 = CARTESIAN_POINT ( 'NONE',  ( 123.9714148109119805, -0.4660016031367893996, -10.09054647747474043 ) ) ;
#20171 = CARTESIAN_POINT ( 'NONE',  ( 116.4267681442453153, -6.222761293078241884, -8.102969835052219238 ) ) ;
#20172 = CARTESIAN_POINT ( 'NONE',  ( 124.5954081442453116, -3.383040157471821630, -19.15922257007629170 ) ) ;
#20173 = DIRECTION ( 'NONE',  ( 0.000000000000000000, 0.6004852223388321697, -0.7996358532186279566 ) ) ;
#20174 = CARTESIAN_POINT ( 'NONE',  ( 124.5357204359119550, -10.25716656981731489, -12.88942061488890545 ) ) ;
#20175 = ORIENTED_EDGE ( 'NONE', *, *, #25053, .T. ) ;
#20176 = PLANE ( 'NONE',  #43389 ) ;
#20177 = CARTESIAN_POINT ( 'NONE',  ( 125.1589444732338308, 2.423665151342216273, -12.11196455044497000 ) ) ;
#20178 = CARTESIAN_POINT ( 'NONE',  ( 109.8574890045247940, -9.868328341294098749, -11.32035403202665869 ) ) ;
#20179 = CARTESIAN_POINT ( 'NONE',  ( 118.0203271540078589, -2.348512537728064675, -17.99195118506216318 ) ) ;
#20180 = CARTESIAN_POINT ( 'NONE',  ( 123.2339681442453241, -3.505236298600246325, -18.68346056562440793 ) ) ;
#20181 = CARTESIAN_POINT ( 'NONE',  ( 113.4769814775786330, 0.4262465694468514643, -12.03445270309931736 ) ) ;
#20182 = CARTESIAN_POINT ( 'NONE',  ( 126.7706290066808492, -6.465199847775628506, -18.42047446121263121 ) ) ;
#20183 = ORIENTED_EDGE ( 'NONE', *, *, #15264, .T. ) ;
#20184 = DIRECTION ( 'NONE',  ( 0.000000000000000000, -0.9242245927363029745, -0.3818493186865927203 ) ) ;
#20185 = CARTESIAN_POINT ( 'NONE',  ( 118.4689281442453392, -10.15424416112533912, -14.75197769757731336 ) ) ;
#20186 = CARTESIAN_POINT ( 'NONE',  ( 114.1009748109119784, -5.574606645277164318, -18.38911715685844683 ) ) ;
#20187 = CARTESIAN_POINT ( 'NONE',  ( 122.3620835773848654, -2.467220198592778413, -17.83387418641524391 ) ) ;
#20188 = DIRECTION ( 'NONE',  ( -0.000000000000000000, -0.9284778069183718952, -0.3713878862591649677 ) ) ;
#20190 = DIRECTION ( 'NONE',  ( 0.000000000000000000, 0.3818493186865929423, -0.9242245927363028635 ) ) ;
#20189 = CARTESIAN_POINT ( 'NONE',  ( 114.0502378519202864, 0.2518737723193609224, -12.14321520033831625 ) ) ;
#20191 = ADVANCED_FACE ( 'NONE', ( #23465 ), #3379, .T. ) ;
#20192 = CARTESIAN_POINT ( 'NONE',  ( 126.6942948109119840, -8.899110576539710493, -16.42337572283490132 ) ) ;
#20193 = VERTEX_POINT ( 'NONE', #9783 ) ;
#20194 = CARTESIAN_POINT ( 'NONE',  ( 112.3424481442453384, -6.344957434206662583, -7.627207830600332805 ) ) ;
#20195 = DIRECTION ( 'NONE',  ( -1.000000000000000000, 0.000000000000000000, 0.000000000000000000 ) ) ;
#20196 = CARTESIAN_POINT ( 'NONE',  ( 115.1359265045248605, -7.250697342233347165, -19.15521520033831138 ) ) ;
#20197 = CARTESIAN_POINT ( 'NONE',  ( 123.9714148109119805, -8.899110576539710493, -16.42337572283490132 ) ) ;
#20198 = CARTESIAN_POINT ( 'NONE',  ( 119.0361948109119652, -2.084020599724406786, -8.691656652584148546 ) ) ;
#20199 = DIRECTION ( 'NONE',  ( 0.000000000000000000, 0.000000000000000000, -1.000000000000000000 ) ) ;
#20200 = CARTESIAN_POINT ( 'NONE',  ( 114.8581140045248361, 0.1403307496149616695, -15.46607636864997204 ) ) ;
#20201 = CARTESIAN_POINT ( 'NONE',  ( 61.05647571779960003, -46.63990697477660063, -12.39321520033831447 ) ) ;
#20202 = CARTESIAN_POINT ( 'NONE',  ( 109.2295511504564303, -2.582258012937524327, -17.92986911656043247 ) ) ;
#20203 = CARTESIAN_POINT ( 'NONE',  ( 112.2857214775786474, -5.574606645277164318, -18.38911715685844683 ) ) ;
#20204 = CARTESIAN_POINT ( 'NONE',  ( 105.5513952545248060, 0.8980012041604421569, -11.00651665394454071 ) ) ;
#20205 = DIRECTION ( 'NONE',  ( 0.9495615000563050190, -0.3135808629537517600, 0.000000000000000000 ) ) ;
#20206 = CARTESIAN_POINT ( 'NONE',  ( 115.5526452545247622, 0.8980012041604421569, -11.00651665394454071 ) ) ;
#20207 = CARTESIAN_POINT ( 'NONE',  ( 125.6164881442453094, 0.2603800115204892296, -16.42320221600525088 ) ) ;
#20208 = CARTESIAN_POINT ( 'NONE',  ( 123.4608748109119745, -10.63000616557722466, -14.87417383870573495 ) ) ;
#20209 = CARTESIAN_POINT ( 'NONE',  ( 115.2748327545248657, -2.477300249445798297, -19.15521520033830427 ) ) ;
#20210 = CARTESIAN_POINT ( 'NONE',  ( 118.6391081442452986, -4.089484607189486809, -7.948022111789456723 ) ) ;
#20211 = CARTESIAN_POINT ( 'NONE',  ( 112.6828081442453282, -7.893985811506177619, -18.51759400769804742 ) ) ;
#20212 = VERTEX_POINT ( 'NONE', #38031 ) ;
#20213 = CARTESIAN_POINT ( 'NONE',  ( 114.3846081442453197, 0.4262465694468514643, -12.03445270309931736 ) ) ;
#20214 = CARTESIAN_POINT ( 'NONE',  ( 111.8886348109120092, -6.222761293078241884, -8.102969835052219238 ) ) ;
#20215 = CARTESIAN_POINT ( 'NONE',  ( 125.0492214775786266, -6.344957434206665248, -7.627207830600338134 ) ) ;
#20216 = CARTESIAN_POINT ( 'NONE',  ( 115.9162281442453235, -4.089484607189486809, -7.948022111789456723 ) ) ;
#20217 = CARTESIAN_POINT ( 'NONE',  ( 111.3213681442453264, -7.643976991954077427, -18.09477374809248928 ) ) ;
#20218 = ORIENTED_EDGE ( 'NONE', *, *, #7534, .T. ) ;
#20219 = CARTESIAN_POINT ( 'NONE',  ( 116.6536748109119941, -10.15424416112533912, -14.75197769757731336 ) ) ;
#20220 = CARTESIAN_POINT ( 'NONE',  ( 106.3153796295248412, -4.863998795839590272, -19.15521520033831493 ) ) ;
#20221 = CARTESIAN_POINT ( 'NONE',  ( 111.3854577545248645, -2.791137627527939813, -18.39754474579286025 ) ) ;
#20222 = CARTESIAN_POINT ( 'NONE',  ( 124.1415948109119540, -3.505236298600246325, -18.68346056562440793 ) ) ;
#20223 = DIRECTION ( 'NONE',  ( 1.000000000000000000, 0.000000000000000000, -0.000000000000000000 ) ) ;
#20224 = CARTESIAN_POINT ( 'NONE',  ( 112.9828796295247884, -4.863998795839590272, -19.15521520033831493 ) ) ;
#20225 = ORIENTED_EDGE ( 'NONE', *, *, #39803, .F. ) ;
#20226 = CIRCLE ( 'NONE', #30412, 2.999999999999996003 ) ;
#20227 = DIRECTION ( 'NONE',  ( -0.2768435750659241079, -0.3568721902840695792, 0.8921882507333129819 ) ) ;
#20228 = CARTESIAN_POINT ( 'NONE',  ( 63.10250807381770244, -31.76310523276723430, -22.89321520033831803 ) ) ;
#20229 = CARTESIAN_POINT ( 'NONE',  ( 112.7982045411902163, -0.3595008806742185925, -10.82052240173743130 ) ) ;
#20230 = CARTESIAN_POINT ( 'NONE',  ( 112.1155414775786454, 0.9020085738987339008, -11.91225656197089222 ) ) ;
#20231 = CARTESIAN_POINT ( 'NONE',  ( 116.2048035453898223, 2.307602176693129614, -6.673484833205728606 ) ) ;
#20232 = DIRECTION ( 'NONE',  ( 0.000000000000000000, 0.000000000000000000, 1.000000000000000000 ) ) ;
#20233 = CARTESIAN_POINT ( 'NONE',  ( 107.4266296295248821, -4.863998795839590272, -8.388885654883775800 ) ) ;
#20234 = CARTESIAN_POINT ( 'NONE',  ( 122.9294065278262451, -1.036737761566197014, -17.24079555149560861 ) ) ;
#20235 = CARTESIAN_POINT ( 'NONE',  ( 119.5467348109119712, -4.089484607189486809, -7.948022111789456723 ) ) ;
#20236 = DIRECTION ( 'NONE',  ( 0.7871354856660198740, 0.4483307682966886643, 0.4235767337848242442 ) ) ;
#20237 = CARTESIAN_POINT ( 'NONE',  ( 84.49707967414211396, -26.75858941326842810, -11.54476601486570964 ) ) ;
#20239 = CARTESIAN_POINT ( 'NONE',  ( 125.5030348109119558, -3.383040157471821630, -19.15922257007629170 ) ) ;
#20238 = VECTOR ( 'NONE', #27004, 1000.000000000000227 ) ;
#20240 = CARTESIAN_POINT ( 'NONE',  ( 122.9503348109119827, -9.859900752359378018, -12.68260735090039759 ) ) ;
#20241 = CARTESIAN_POINT ( 'NONE',  ( 41.72636039845269096, -11.37347657059392070, -10.39321520033831625 ) ) ;
#20242 = ORIENTED_EDGE ( 'NONE', *, *, #7655, .T. ) ;
#20243 = CARTESIAN_POINT ( 'NONE',  ( 125.2194014775786286, -10.30919188438810075, -12.61870101168855918 ) ) ;
#20244 = CARTESIAN_POINT ( 'NONE',  ( 121.0216281442452981, -1.561330072975668948, -17.79121239304076951 ) ) ;
#20245 = CARTESIAN_POINT ( 'NONE',  ( 86.34560043013698305, -9.320000780048239619, -18.64321520033831803 ) ) ;
#20246 = CARTESIAN_POINT ( 'NONE',  ( 115.9729548109119861, -3.505236298600246325, -18.68346056562440793 ) ) ;
#20247 = CARTESIAN_POINT ( 'NONE',  ( 124.2550481442452792, -9.988377603198980381, -10.36322818467138518 ) ) ;
#20248 = CARTESIAN_POINT ( 'NONE',  ( 112.0799890045248475, 0.8980012041604421569, -15.77991374673208469 ) ) ;
#20249 = LINE ( 'NONE', #37330, #38028 ) ;
#20250 = CARTESIAN_POINT ( 'NONE',  ( 116.5249890045247980, 0.8980012041604421569, -15.77991374673208469 ) ) ;
#20251 = CARTESIAN_POINT ( 'NONE',  ( 116.8238548109119819, -5.574606645277164318, -18.38911715685844683 ) ) ;
#20252 = CARTESIAN_POINT ( 'NONE',  ( 118.5256548109119876, -8.899110576539710493, -16.42337572283490132 ) ) ;
#20253 = DIRECTION ( 'NONE',  ( 0.000000000000000000, -0.3818493186865927203, 0.9242245927363029745 ) ) ;
#20254 = CARTESIAN_POINT ( 'NONE',  ( 112.2188952545247531, -9.868328341294098749, -15.46607636864997204 ) ) ;
#20255 = ORIENTED_EDGE ( 'NONE', *, *, #20644, .F. ) ;
#20256 = CARTESIAN_POINT ( 'NONE',  ( 67.37136766119182596, -70.31694239570130378, -42.20474206142759499 ) ) ;
#20257 = CARTESIAN_POINT ( 'NONE',  ( 114.1009748109119784, -4.089484607189486809, -7.948022111789456723 ) ) ;
#20258 = CARTESIAN_POINT ( 'NONE',  ( 112.9120775202278253, -2.239543233855025850, -18.13706010537467606 ) ) ;
#20259 = CARTESIAN_POINT ( 'NONE',  ( 121.5492360609119800, -3.387241619883791355, -18.17469012370385073 ) ) ;
#20260 = CARTESIAN_POINT ( 'NONE',  ( 120.3685329359119862, -5.367793381288652910, -18.78638297431638904 ) ) ;
#20261 = VERTEX_POINT ( 'NONE', #6808 ) ;
#20262 = CARTESIAN_POINT ( 'NONE',  ( 123.7184548109119788, -3.484218720211407661, -13.98160872758045770 ) ) ;
#20263 = CARTESIAN_POINT ( 'NONE',  ( 111.5085532531557106, -1.270193261574751542, -16.92991464886373976 ) ) ;
#20264 = ORIENTED_EDGE ( 'NONE', *, *, #3550, .F. ) ;
#20265 = CARTESIAN_POINT ( 'NONE',  ( 117.2209414775786485, -7.893985811506177619, -18.51759400769804742 ) ) ;
#20266 = CARTESIAN_POINT ( 'NONE',  ( 126.5808414775786446, -9.859900752359378018, -12.68260735090039759 ) ) ;
#20267 = CARTESIAN_POINT ( 'NONE',  ( 118.7525614775786380, -1.833838273342659253, -17.42832698103878286 ) ) ;
#20268 = SHAPE_REPRESENTATION_RELATIONSHIP ( 'NONE' , 'NONE' ,  #15458, #41161 ) ;
#20269 = DIRECTION ( 'NONE',  ( 0.4649787261689617424, 0.8853218534579895271, 0.000000000000000000 ) ) ;
#20270 = CARTESIAN_POINT ( 'NONE',  ( 123.4041481442452834, -10.30919188438810075, -12.61870101168855918 ) ) ;
#20271 = CARTESIAN_POINT ( 'NONE',  ( 116.7671281442453335, -1.834011780172310813, -8.268836392978581529 ) ) ;
#20272 = CARTESIAN_POINT ( 'NONE',  ( 106.4542858795248179, -8.402594152722688392, -9.854619843455216355 ) ) ;
#20273 = CARTESIAN_POINT ( 'NONE',  ( 112.8529881442453160, -7.894159318335828068, -9.358103419637847864 ) ) ;
#20274 = PLANE ( 'NONE',  #2419 ) ;
#20275 = EDGE_LOOP ( 'NONE', ( #18099, #24573, #41917, #23693 ) ) ;
#20276 = CARTESIAN_POINT ( 'NONE',  ( 117.6747548109119919, -1.834011780172310813, -8.268836392978581529 ) ) ;
#20277 = ADVANCED_FACE ( 'NONE', ( #13867 ), #23556, .T. ) ;
#20278 = CARTESIAN_POINT ( 'NONE',  ( 67.84197459855160162, -51.79774043821656448, -34.65109778699235221 ) ) ;
#20279 = CARTESIAN_POINT ( 'NONE',  ( 114.8384214775786489, 0.9020085738987339008, -11.91225656197089222 ) ) ;
#20280 = ORIENTED_EDGE ( 'NONE', *, *, #44070, .T. ) ;
#20281 = CARTESIAN_POINT ( 'NONE',  ( 120.9081748109119872, -5.638512984488999180, -18.83840828888717311 ) ) ;
#20282 = DIRECTION ( 'NONE',  ( 0.000000000000000000, -0.3818493186865927203, 0.9242245927363029745 ) ) ;
#20283 = CARTESIAN_POINT ( 'NONE',  ( 113.1366214775786432, -7.643976991954077427, -18.09477374809248928 ) ) ;
#20284 = EDGE_CURVE ( 'NONE', #31497, #32564, #3565, .T. ) ;
#20285 = CARTESIAN_POINT ( 'NONE',  ( 78.46442941731035603, -58.56046118940295742, -0.3236597056445599807 ) ) ;
#20286 = CARTESIAN_POINT ( 'NONE',  ( 116.3133148109120043, -2.084020599724406786, -8.691656652584148546 ) ) ;
#20287 = DIRECTION ( 'NONE',  ( -0.9908103287288504424, 0.1352586133457951423, 0.000000000000000000 ) ) ;
#20288 = CARTESIAN_POINT ( 'NONE',  ( 116.4834948109119779, -7.894159318335828068, -9.358103419637847864 ) ) ;
#20289 = CARTESIAN_POINT ( 'NONE',  ( 66.82415148905926117, -40.21211973637273474, -21.89321520033831447 ) ) ;
#20290 = CARTESIAN_POINT ( 'NONE',  ( 117.1074881442453233, 0.4262465694468514643, -12.03445270309931736 ) ) ;
#20291 = CARTESIAN_POINT ( 'NONE',  ( 115.2922348109119781, -10.63000616557722466, -14.87417383870573495 ) ) ;
#20292 = CARTESIAN_POINT ( 'NONE',  ( 119.9518141859119851, -0.8832429491016019485, -18.19431474523657855 ) ) ;
#20293 = CARTESIAN_POINT ( 'NONE',  ( 112.0588148109119828, 0.5811942927096154232, -14.16772938898807155 ) ) ;
#20294 = CARTESIAN_POINT ( 'NONE',  ( 116.8238548109119819, -5.574606645277164318, -18.38911715685844683 ) ) ;
#20295 = CARTESIAN_POINT ( 'NONE',  ( 113.3635281442453504, -0.1624402480850797581, -16.17319339645315424 ) ) ;
#20296 = CARTESIAN_POINT ( 'NONE',  ( 115.1220548109119761, -1.833838273342658809, -17.42832698103878286 ) ) ;
#20297 = ORIENTED_EDGE ( 'NONE', *, *, #5784, .T. ) ;
#20298 = CARTESIAN_POINT ( 'NONE',  ( 113.9875214775786532, -0.4660016031367893996, -10.09054647747474043 ) ) ;
#20299 = CARTESIAN_POINT ( 'NONE',  ( 106.1764733795248219, -8.938348069036489818, -17.46756447353520159 ) ) ;
#20300 = EDGE_CURVE ( 'NONE', #2526, #19765, #13653, .T. ) ;
#20301 = CARTESIAN_POINT ( 'NONE',  ( 107.7738952545248310, -9.868328341294098749, -15.46607636864997204 ) ) ;
#20302 = CARTESIAN_POINT ( 'NONE',  ( 105.6903015045248253, -6.936859964151250502, -18.39754474579286025 ) ) ;
#20303 = CARTESIAN_POINT ( 'NONE',  ( 109.3713171295247832, -10.62599879583958540, -13.39321520033830382 ) ) ;
#20304 = CARTESIAN_POINT ( 'NONE',  ( 117.1642148109119859, -9.261995988541697145, -16.69588392320189030 ) ) ;
#20305 = VERTEX_POINT ( 'NONE', #3157 ) ;
#20306 = CARTESIAN_POINT ( 'NONE',  ( 125.1626748109119802, -9.988377603198980381, -10.36322818467138518 ) ) ;
#20307 = CARTESIAN_POINT ( 'NONE',  ( 117.8449348109119938, -1.833838273342659253, -17.42832698103878286 ) ) ;
#20308 = ADVANCED_FACE ( 'NONE', ( #9549 ), #37351, .T. ) ;
#20309 = FACE_OUTER_BOUND ( 'NONE', #13858, .T. ) ;
#20310 = CARTESIAN_POINT ( 'NONE',  ( 123.6310548109119765, -5.638512984488999180, -18.83840828888717311 ) ) ;
#20311 = EDGE_CURVE ( 'NONE', #40384, #14664, #2695, .T. ) ;
#20312 = CARTESIAN_POINT ( 'NONE',  ( 108.0517077545248696, -7.250697342233347165, -7.631215200338321125 ) ) ;
#20313 = CARTESIAN_POINT ( 'NONE',  ( 89.13434580277143482, -10.42584736732164608, -14.07205986288570010 ) ) ;
#20314 = ORIENTED_EDGE ( 'NONE', *, *, #39875, .T. ) ;
#20315 = CARTESIAN_POINT ( 'NONE',  ( 112.2857214775786474, -4.089484607189486809, -7.948022111789456723 ) ) ;
#20316 = CARTESIAN_POINT ( 'NONE',  ( 123.9146881442452894, -10.15424416112533912, -14.75197769757731336 ) ) ;
#20317 = CARTESIAN_POINT ( 'NONE',  ( 119.1496481442453046, -3.383040157471821630, -19.15922257007629170 ) ) ;
#20318 = CARTESIAN_POINT ( 'NONE',  ( 118.0151148109119816, 0.4262465694468514643, -12.03445270309931736 ) ) ;
#20319 = CARTESIAN_POINT ( 'NONE',  ( 118.0151148109119816, -10.63000616557722466, -14.87417383870573495 ) ) ;
#20320 = CARTESIAN_POINT ( 'NONE',  ( 83.44708369096697709, -25.99489077589524300, -13.39321520033831625 ) ) ;
#20321 =( BOUNDED_SURFACE ( )  B_SPLINE_SURFACE ( 1, 2, ( 
 ( #41784, #24441, #7109, #21019, #34892, #24661, #3681, #266, #14175, #11440, #1823, #40145, #15295, #25786, #29204, #29427, #39469 ),
 ( #25563, #42670, #1600, #25345, #35805, #36485, #5252, #36032, #28764, #15075, #36702, #42894, #22140, #12111, #15752, #15520, #39239 ) ),
 .UNSPECIFIED., .F., .F., .F. ) 
 B_SPLINE_SURFACE_WITH_KNOTS ( ( 2, 2 ),
 ( 3, 2, 2, 2, 2, 2, 2, 2, 3 ),
 ( 0.000000000000000000, 1.000000000000000000 ),
 ( 0.000000000000000000, 0.1250000000000000000, 0.2500000000000000000, 0.3750000000000000000, 0.5000000000000000000, 0.6250000000000000000, 0.7500000000000000000, 0.8750000000000000000, 1.000000000000000000 ),
 .UNSPECIFIED. ) 
 GEOMETRIC_REPRESENTATION_ITEM ( )  RATIONAL_B_SPLINE_SURFACE ( (
 ( 1.000000000000000000, 0.9238795325112869605, 1.000000000000000000, 0.9238795325112869605, 1.000000000000000000, 0.9238795325112869605, 1.000000000000000000, 0.9238795325112869605, 1.000000000000000000, 0.9238795325112869605, 1.000000000000000000, 0.9238795325112869605, 1.000000000000000000, 0.9238795325112869605, 1.000000000000000000, 0.9238795325112869605, 1.000000000000000000),
 ( 1.000000000000000000, 0.9238795325112869605, 1.000000000000000000, 0.9238795325112869605, 1.000000000000000000, 0.9238795325112869605, 1.000000000000000000, 0.9238795325112869605, 1.000000000000000000, 0.9238795325112869605, 1.000000000000000000, 0.9238795325112869605, 1.000000000000000000, 0.9238795325112869605, 1.000000000000000000, 0.9238795325112869605, 1.000000000000000000) ) ) 
 REPRESENTATION_ITEM ( '' )  SURFACE ( )  );
#20322 = CARTESIAN_POINT ( 'NONE',  ( 126.3671785243083150, -1.099405526347972284, -9.990639651589864556 ) ) ;
#20323 = CARTESIAN_POINT ( 'NONE',  ( 121.8725281442453223, -6.222761293078241884, -8.102969835052219238 ) ) ;
#20324 = EDGE_LOOP ( 'NONE', ( #26245, #43972 ) ) ;
#20325 = EDGE_CURVE ( 'NONE', #9951, #31450, #24267, .T. ) ;
#20326 = DIRECTION ( 'NONE',  ( 1.000000000000000000, 0.000000000000000000, 0.000000000000000000 ) ) ;
#20327 = CARTESIAN_POINT ( 'NONE',  ( 118.2987481442453088, -1.561330072975668504, -17.79121239304076951 ) ) ;
#20328 = CARTESIAN_POINT ( 'NONE',  ( 122.5532481442453019, 0.4262465694468514643, -12.03445270309931736 ) ) ;
#20329 = VERTEX_POINT ( 'NONE', #44441 ) ;
#20330 = EDGE_CURVE ( 'NONE', #37005, #42142, #13208, .T. ) ;
#20331 = CARTESIAN_POINT ( 'NONE',  ( 121.3408766859119794, -9.033780868592240054, -16.85052413769862056 ) ) ;
#20332 = CARTESIAN_POINT ( 'NONE',  ( 135.5837700376040118, -1.194507185862332399, -8.657517032471606200 ) ) ;
#20333 = EDGE_CURVE ( 'NONE', #34402, #33083, #37803, .T. ) ;
#20334 = EDGE_CURVE ( 'NONE', #4744, #31560, #19897, .T. ) ;
#20335 = CARTESIAN_POINT ( 'NONE',  ( 118.5823814775786360, -1.834011780172310813, -8.268836392978581529 ) ) ;
#20336 = CARTESIAN_POINT ( 'NONE',  ( 110.3436608795247764, -8.938348069036489818, -9.318865927141430916 ) ) ;
#20337 = CARTESIAN_POINT ( 'NONE',  ( 120.6812681442452941, 0.1319031606808879209, -14.10382304977623669 ) ) ;
#20338 = ORIENTED_EDGE ( 'NONE', *, *, #37271, .F. ) ;
#20339 = ORIENTED_EDGE ( 'NONE', *, *, #14202, .T. ) ;
#20340 = CARTESIAN_POINT ( 'NONE',  ( 112.6260814775786514, -9.261995988541697145, -16.69588392320189030 ) ) ;
#20341 = AXIS2_PLACEMENT_3D ( 'NONE', #7019, #34804, #25473 ) ;
#20342 = CARTESIAN_POINT ( 'NONE',  ( 123.0070614775786169, -10.15424416112533912, -14.75197769757731336 ) ) ;
#20343 = CIRCLE ( 'NONE', #24714, 6.426280380454326924 ) ;
#20344 = CARTESIAN_POINT ( 'NONE',  ( 70.19189222814998175, -54.26662894631272849, -34.90947156805651019 ) ) ;
#20345 = DIRECTION ( 'NONE',  ( 0.9609149988134837450, -0.1028163501681639419, 0.2570431154366518145 ) ) ;
#20346 = CARTESIAN_POINT ( 'NONE',  ( 121.1350814775786233, 0.5811942927096110934, -14.16772938898807510 ) ) ;
#20347 = CARTESIAN_POINT ( 'NONE',  ( 75.95778847736481509, -3.256761025687722189, -8.143215200338314474 ) ) ;
#20348 = CARTESIAN_POINT ( 'NONE',  ( 117.2252848144346729, -2.280480477428486807, -18.08254604495228435 ) ) ;
#20349 = CARTESIAN_POINT ( 'NONE',  ( 120.8514481442452961, -7.893985811506177619, -18.51759400769804742 ) ) ;
#20351 = CARTESIAN_POINT ( 'NONE',  ( 120.5678148109119832, -1.833838273342659253, -17.42832698103878286 ) ) ;
#20350 = CARTESIAN_POINT ( 'NONE',  ( 118.2420214775786320, -3.383040157471821630, -19.15922257007629170 ) ) ;
#20352 = DIRECTION ( 'NONE',  ( 0.9908103287288504424, -0.1352586133457950035, 0.000000000000000000 ) ) ;
#20353 = CARTESIAN_POINT ( 'NONE',  ( 112.7395348109119766, -5.638512984488999180, -18.83840828888717311 ) ) ;
#20354 = ORIENTED_EDGE ( 'NONE', *, *, #30585, .T. ) ;
#20355 = CARTESIAN_POINT ( 'NONE',  ( 121.9292548109119849, -7.894159318335828068, -9.358103419637847864 ) ) ;
#20356 = CARTESIAN_POINT ( 'NONE',  ( 125.6059481442453318, -7.866424907534184996, -9.395035934245763443 ) ) ;
#20357 = CARTESIAN_POINT ( 'NONE',  ( 107.4266296295248821, -4.863998795839590272, -19.15521520033831493 ) ) ;
#20358 = CARTESIAN_POINT ( 'NONE',  ( 115.4137390045248566, -9.868328341294098749, -11.32035403202665869 ) ) ;
#20359 = CARTESIAN_POINT ( 'NONE',  ( 107.6349890045248401, 0.8980012041604421569, -15.77991374673208469 ) ) ;
#20360 = CARTESIAN_POINT ( 'NONE',  ( 124.0848681442452772, -4.089484607189486809, -7.948022111789456723 ) ) ;
#20361 = CARTESIAN_POINT ( 'NONE',  ( 121.7590748109119687, -2.084020599724406786, -8.691656652584148546 ) ) ;
#20362 = ORIENTED_EDGE ( 'NONE', *, *, #20396, .F. ) ;
#20363 = CARTESIAN_POINT ( 'NONE',  ( 125.9001214775786224, -4.089484607189486809, -7.948022111789456723 ) ) ;
#20364 = CARTESIAN_POINT ( 'NONE',  ( 110.2184548109119788, -4.863998795839242995, -13.39321520033831447 ) ) ;
#20365 = LINE ( 'NONE', #27205, #3756 ) ;
#20366 = CARTESIAN_POINT ( 'NONE',  ( 123.1772414775786189, -4.089484607189486809, -7.948022111789456723 ) ) ;
#20367 = CARTESIAN_POINT ( 'NONE',  ( 122.3830681442452857, -8.166667518702819706, -8.995218007635861213 ) ) ;
#20368 = CARTESIAN_POINT ( 'NONE',  ( 119.8791860609119624, -6.339478340643393217, -8.615877017535622073 ) ) ;
#20369 = CARTESIAN_POINT ( 'NONE',  ( 125.8433948109119456, -7.643976991954077427, -18.09477374809248928 ) ) ;
#20370 = CARTESIAN_POINT ( 'NONE',  ( 135.3184548109119874, -0.6896191363000483410, -17.70303589939592825 ) ) ;
#20371 = CARTESIAN_POINT ( 'NONE',  ( 114.2330358795247776, -8.402594152722688392, -9.854619843455216355 ) ) ;
#20372 = ORIENTED_EDGE ( 'NONE', *, *, #7203, .T. ) ;
#20373 = CARTESIAN_POINT ( 'NONE',  ( 125.0849635773846842, -2.467220198597905867, -17.83387418641800437 ) ) ;
#20374 = CARTESIAN_POINT ( 'NONE',  ( 113.1933481442453058, -5.574606645277164318, -18.38911715685844683 ) ) ;
#20375 = CARTESIAN_POINT ( 'NONE',  ( 122.2696148109119889, -5.574606645277164318, -18.38911715685844683 ) ) ;
#20376 = AXIS2_PLACEMENT_3D ( 'NONE', #25415, #14473, #35875 ) ;
#20377 = CARTESIAN_POINT ( 'NONE',  ( 106.3153796295248412, -4.863998795839590272, -8.388885654883775800 ) ) ;
#20378 = CARTESIAN_POINT ( 'NONE',  ( 106.5237390045248418, -9.868328341294098749, -11.32035403202665869 ) ) ;
#20380 = CIRCLE ( 'NONE', #16737, 2.000000000000000444 ) ;
#20379 = CARTESIAN_POINT ( 'NONE',  ( 122.7234281442452755, -4.153390946401325223, -8.397313243818185668 ) ) ;
#20381 = CARTESIAN_POINT ( 'NONE',  ( 115.5191414775786569, -6.222761293078241884, -8.102969835052219238 ) ) ;
#20382 = CARTESIAN_POINT ( 'NONE',  ( 112.2289948109119848, -7.643976991954077427, -18.09477374809248928 ) ) ;
#20383 = ORIENTED_EDGE ( 'NONE', *, *, #15305, .T. ) ;
#20384 = EDGE_CURVE ( 'NONE', #23226, #18085, #44132, .T. ) ;
#20385 = CARTESIAN_POINT ( 'NONE',  ( 123.8012348109119642, -9.565557343593413364, -10.61323700422348004 ) ) ;
#20386 = CARTESIAN_POINT ( 'NONE',  ( 118.5823814775786360, -1.834011780172310813, -8.268836392978581529 ) ) ;
#20387 = CARTESIAN_POINT ( 'NONE',  ( 83.72016463086879412, -26.75858941326842810, -11.54476601486570964 ) ) ;
#20388 = ORIENTED_EDGE ( 'NONE', *, *, #35586, .T. ) ;
#20389 = AXIS2_PLACEMENT_3D ( 'NONE', #19998, #37538, #13393 ) ;
#20390 = CARTESIAN_POINT ( 'NONE',  ( 120.5074391859119913, -1.406689858478935573, -17.56299727309130887 ) ) ;
#20391 = EDGE_CURVE ( 'NONE', #25821, #12113, #18580, .T. ) ;
#20392 = VERTEX_POINT ( 'NONE', #12441 ) ;
#20393 = EDGE_CURVE ( 'NONE', #17270, #34946, #44679, .T. ) ;
#20394 = CARTESIAN_POINT ( 'NONE',  ( 115.1787814775786387, -0.1624402480850797581, -16.17319339645315424 ) ) ;
#20395 = CARTESIAN_POINT ( 'NONE',  ( 114.2711548109119803, -0.1624402480850797581, -16.17319339645315424 ) ) ;
#20396 = EDGE_CURVE ( 'NONE', #35058, #7733, #9721, .T. ) ;
#20397 = CARTESIAN_POINT ( 'NONE',  ( 114.9518748109119883, -1.834011780172303929, -8.268836392978592187 ) ) ;
#20398 = CARTESIAN_POINT ( 'NONE',  ( 119.8129079359119942, -5.444069387712269226, -19.60292469916370450 ) ) ;
#20399 = ORIENTED_EDGE ( 'NONE', *, *, #37934, .F. ) ;
#20400 = CARTESIAN_POINT ( 'NONE',  ( 75.95778847736481509, -3.256761025687722189, -8.143215200338314474 ) ) ;
#20401 = CARTESIAN_POINT ( 'NONE',  ( 124.6565730087419581, 2.130358918975589599, -9.869583666609218042 ) ) ;
#20402 = CARTESIAN_POINT ( 'NONE',  ( 106.0375671295248310, 0.1403307496149613920, -13.39321520033831447 ) ) ;
#20403 = DIRECTION ( 'NONE',  ( 1.000000000000000000, 0.000000000000000000, -0.000000000000000000 ) ) ;
#20404 = CARTESIAN_POINT ( 'NONE',  ( 121.7590748109119687, -2.084020599724406786, -8.691656652584148546 ) ) ;
#20405 = CARTESIAN_POINT ( 'NONE',  ( 114.6115148109119986, -6.222761293078241884, -8.102969835052219238 ) ) ;
#20406 = CARTESIAN_POINT ( 'NONE',  ( 125.2194014775786286, 0.1319031606808887813, -14.10382304977621182 ) ) ;
#20407 = ORIENTED_EDGE ( 'NONE', *, *, #35055, .F. ) ;
#20408 = DIRECTION ( 'NONE',  ( 0.000000000000000000, 0.6004852223388321697, -0.7996358532186279566 ) ) ;
#20409 = CARTESIAN_POINT ( 'NONE',  ( 73.07463722459043254, -51.78964457606210203, -33.02417856296905541 ) ) ;
#20410 = AXIS2_PLACEMENT_3D ( 'NONE', #44911, #20730, #6139 ) ;
#20411 = CARTESIAN_POINT ( 'NONE',  ( 112.5661608795247872, -8.938348069036489818, -9.318865927141430916 ) ) ;
#20412 = CARTESIAN_POINT ( 'NONE',  ( 111.8991748109119868, -7.866424907533402511, -9.395035934245173692 ) ) ;
#20414 = CARTESIAN_POINT ( 'NONE',  ( 125.1059481442452750, -8.166667518702819706, -8.995218007635861213 ) ) ;
#20413 = CARTESIAN_POINT ( 'NONE',  ( 65.68057756587693063, -37.02887214625545909, -5.220056341857074678 ) ) ;
#20415 = CARTESIAN_POINT ( 'NONE',  ( 126.4106614775786284, -6.222761293078241884, -8.102969835052219238 ) ) ;
#20416 = ORIENTED_EDGE ( 'NONE', *, *, #29573, .T. ) ;
#20417 = VECTOR ( 'NONE', #30478, 999.9999999999998863 ) ;
#20418 = CARTESIAN_POINT ( 'NONE',  ( 112.0588148109119828, 0.5811942927096154232, -14.16772938898807155 ) ) ;
#20419 = CARTESIAN_POINT ( 'NONE',  ( 113.6232486830090096, -1.087735405160637603, -17.17288456429614030 ) ) ;
#20420 = CARTESIAN_POINT ( 'NONE',  ( 116.4555358795247884, -0.7896495226426338832, -17.46756447353520159 ) ) ;
#20421 = CARTESIAN_POINT ( 'NONE',  ( 125.5030348109119558, -6.222761293078241884, -8.102969835052219238 ) ) ;
#20422 = CARTESIAN_POINT ( 'NONE',  ( 123.6877814775786533, -6.222761293078241884, -8.102969835052219238 ) ) ;
#20423 = DIRECTION ( 'NONE',  ( 1.000000000000000000, 0.000000000000000000, 0.000000000000000000 ) ) ;
#20424 = CARTESIAN_POINT ( 'NONE',  ( 114.5803015045248117, -6.936859964151250502, -18.39754474579286025 ) ) ;
#20425 = CARTESIAN_POINT ( 'NONE',  ( 120.3924224678160897, -1.149058757900107697, -17.09122335155391781 ) ) ;
#20426 = DIRECTION ( 'NONE',  ( 0.000000000000000000, -0.3818493186865927203, 0.9242245927363029745 ) ) ;
#20427 = CARTESIAN_POINT ( 'NONE',  ( 113.0798948109119948, -8.899110576539717599, -16.42337572283489422 ) ) ;
#20428 = DIRECTION ( 'NONE',  ( 1.000000000000000000, 0.000000000000000000, 0.000000000000000000 ) ) ;
#20429 = CARTESIAN_POINT ( 'NONE',  ( 117.7314814775786260, -4.089484607189483256, -7.948022111789462052 ) ) ;
#20430 = CARTESIAN_POINT ( 'NONE',  ( 112.9828796295247884, -4.863998795839590272, -19.15521520033831493 ) ) ;
#20431 = CARTESIAN_POINT ( 'NONE',  ( 123.0637881442452937, -0.4660016031367893996, -10.09054647747474043 ) ) ;
#20432 = CARTESIAN_POINT ( 'NONE',  ( 125.3328548109119964, -9.261995988541697145, -16.69588392320189030 ) ) ;
#20433 = CARTESIAN_POINT ( 'NONE',  ( 115.0664733795247798, -8.938348069036441856, -17.46756447353520514 ) ) ;
#20434 = CARTESIAN_POINT ( 'NONE',  ( 119.3765548109119834, 0.9020085738987339008, -11.91225656197089222 ) ) ;
#20435 = CARTESIAN_POINT ( 'NONE',  ( 113.3635281442453504, -9.988377603198976828, -10.36322818467138340 ) ) ;
#20437 = EDGE_LOOP ( 'NONE', ( #698, #1376, #12903, #41529 ) ) ;
#20436 = EDGE_CURVE ( 'NONE', #42783, #3386, #31824, .T. ) ;
#20438 = CARTESIAN_POINT ( 'NONE',  ( 112.2289948109119848, -7.643976991954077427, -18.09477374809248928 ) ) ;
#20439 = CARTESIAN_POINT ( 'NONE',  ( 125.4463081442452932, -5.638512984488999180, -18.83840828888717311 ) ) ;
#20440 = CARTESIAN_POINT ( 'NONE',  ( 124.8223148109119762, 0.9020085738987339008, -11.91225656197089222 ) ) ;
#20441 = CONICAL_SURFACE ( 'NONE', #12422, 2.000000000000000444, 0.9599310885968830309 ) ;
#20442 = CARTESIAN_POINT ( 'NONE',  ( 115.3489614775786407, -9.261995988541697145, -16.69588392320189030 ) ) ;
#20443 = CARTESIAN_POINT ( 'NONE',  ( 113.4769814775786330, 0.4262465694468514643, -12.03445270309931736 ) ) ;
#20444 = ORIENTED_EDGE ( 'NONE', *, *, #9982, .T. ) ;
#20445 = CARTESIAN_POINT ( 'NONE',  ( 117.6747548109119919, -7.643976991954077427, -18.09477374809248928 ) ) ;
#20446 = CARTESIAN_POINT ( 'NONE',  ( 112.0588148109119828, 0.5811942927096154232, -14.16772938898807155 ) ) ;
#20447 = EDGE_CURVE ( 'NONE', #17073, #34692, #41038, .T. ) ;
#20448 = CARTESIAN_POINT ( 'NONE',  ( 122.6667014775786413, -2.084020599724406786, -8.691656652584148546 ) ) ;
#20449 = DIRECTION ( 'NONE',  ( 0.000000000000000000, 0.9284778069183718952, 0.3713878862591649677 ) ) ;
#20450 = CARTESIAN_POINT ( 'NONE',  ( 111.5243640045248412, -10.62599879583958717, -11.00651665394454604 ) ) ;
#20451 = ORIENTED_EDGE ( 'NONE', *, *, #30928, .F. ) ;
#20452 = CONICAL_SURFACE ( 'NONE', #35676, 0.4999999999999999445, 0.7853981633974476129 ) ;
#20453 = FACE_OUTER_BOUND ( 'NONE', #34044, .T. ) ;
#20454 = LINE ( 'NONE', #13392, #20810 ) ;
#20455 = CARTESIAN_POINT ( 'NONE',  ( 116.3166296295247832, -4.863998795839590272, -8.388885654883775800 ) ) ;
#20456 = CARTESIAN_POINT ( 'NONE',  ( 76.69189222814998175, -49.76310523276723785, -19.39321520033831447 ) ) ;
#20457 = LINE ( 'NONE', #16353, #6247 ) ;
#20458 = CARTESIAN_POINT ( 'NONE',  ( 112.6260814775786514, -0.8288870151387760510, -10.36305467784173118 ) ) ;
#20459 = CARTESIAN_POINT ( 'NONE',  ( 105.1346765045248475, -2.791137627527939813, -8.388885654883777576 ) ) ;
#20460 = CARTESIAN_POINT ( 'NONE',  ( 86.50830818076254047, -21.65036132658698520, -21.89321520033831447 ) ) ;
#20461 = CARTESIAN_POINT ( 'NONE',  ( 118.9794681442453026, -9.261995988541697145, -16.69588392320189030 ) ) ;
#20462 = CARTESIAN_POINT ( 'NONE',  ( 137.1760413997919557, -6.546412817364553050, -18.44820575760469339 ) ) ;
#20463 = CYLINDRICAL_SURFACE ( 'NONE', #28864, 1.587500000000000355 ) ;
#20464 = ADVANCED_FACE ( 'NONE', ( #33840 ), #30083, .F. ) ;
#20465 = CARTESIAN_POINT ( 'NONE',  ( 70.19189222814998175, -61.69445140165969121, -37.88057465812982372 ) ) ;
#20466 = CARTESIAN_POINT ( 'NONE',  ( 120.2274548109119934, -9.859900752359378018, -12.68260735090039759 ) ) ;
#20467 = ORIENTED_EDGE ( 'NONE', *, *, #23236, .F. ) ;
#20468 = CARTESIAN_POINT ( 'NONE',  ( 135.9373687277912097, -9.538988841393456042, -9.739382474596094852 ) ) ;
#20469 = CARTESIAN_POINT ( 'NONE',  ( 117.6747548109119919, -1.834011780172310813, -8.268836392978581529 ) ) ;
#20470 = FACE_OUTER_BOUND ( 'NONE', #18734, .T. ) ;
#20471 = CARTESIAN_POINT ( 'NONE',  ( 116.9940348109119839, -0.1624402480850797581, -16.17319339645315424 ) ) ;
#20472 = CARTESIAN_POINT ( 'NONE',  ( 111.8319081442453182, -4.153390946401321671, -8.397313243818183892 ) ) ;
#20473 = CARTESIAN_POINT ( 'NONE',  ( 111.5243640045248412, -10.62599879583958717, -11.00651665394454604 ) ) ;
#20474 = DIRECTION ( 'NONE',  ( -0.1736481776669309696, -0.9848077530122079093, 0.000000000000000000 ) ) ;
#20475 = CARTESIAN_POINT ( 'NONE',  ( 115.4831921295247952, 0.8980012041604618078, -13.39321520033831447 ) ) ;
#20476 = CARTESIAN_POINT ( 'NONE',  ( 116.2565881442453133, -0.8288870151387760510, -10.36305467784173118 ) ) ;
#20477 = AXIS2_PLACEMENT_3D ( 'NONE', #36105, #32897, #26309 ) ;
#20478 = CARTESIAN_POINT ( 'NONE',  ( 119.4332814775786318, -8.899110576539710493, -16.42337572283490132 ) ) ;
#20479 = DIRECTION ( 'NONE',  ( 0.1352586133457957807, 0.9908103287288503314, 0.000000000000000000 ) ) ;
#20480 = CARTESIAN_POINT ( 'NONE',  ( 120.7852516859119731, -9.665098340737509730, -17.37397104707595474 ) ) ;
#20481 = CARTESIAN_POINT ( 'NONE',  ( 108.1211608795247798, -1.325403438956436419, -16.93181055722141792 ) ) ;
#20482 = ORIENTED_EDGE ( 'NONE', *, *, #45135, .F. ) ;
#20483 = CIRCLE ( 'NONE', #16070, 10.00000000000000000 ) ;
#20484 = CARTESIAN_POINT ( 'NONE',  ( 87.44708369096657918, -23.44614552640564042, -8.393215200338314474 ) ) ;
#20485 = CARTESIAN_POINT ( 'NONE',  ( 115.3489614775786407, -9.261995988541697145, -16.69588392320189030 ) ) ;
#20486 = CARTESIAN_POINT ( 'NONE',  ( 111.7184548109119788, -9.261995988541697145, -16.69588392320189030 ) ) ;
#20487 = CARTESIAN_POINT ( 'NONE',  ( 121.8965016859119856, -0.6942167230862511529, -9.935906262978006609 ) ) ;
#20488 = CARTESIAN_POINT ( 'NONE',  ( 121.1325173109119788, -9.289237151508434209, -11.05642687123711276 ) ) ;
#20489 = ORIENTED_EDGE ( 'NONE', *, *, #15751, .T. ) ;
#20490 = CARTESIAN_POINT ( 'NONE',  ( 113.7468640045248094, -10.62599879583958540, -11.00651665394455492 ) ) ;
#20491 = ORIENTED_EDGE ( 'NONE', *, *, #1470, .F. ) ;
#20492 = CARTESIAN_POINT ( 'NONE',  ( 123.4041481442452834, -10.30919188438810075, -12.61870101168855918 ) ) ;
#20493 = CARTESIAN_POINT ( 'NONE',  ( 113.5904348109119866, -7.893985811506177619, -18.51759400769804742 ) ) ;
#20494 = CARTESIAN_POINT ( 'NONE',  ( 118.9794681442453026, -0.8288870151387760510, -10.36305467784173118 ) ) ;
#20495 = CARTESIAN_POINT ( 'NONE',  ( 120.2521385739447908, -8.245948579112495125, -17.07794576319270163 ) ) ;
#20496 = CARTESIAN_POINT ( 'NONE',  ( 123.5743281442453139, -7.893985811506177619, -18.51759400769804742 ) ) ;
#20497 = CARTESIAN_POINT ( 'NONE',  ( 118.3554748109119998, 0.2603800115204892296, -16.42320221600525088 ) ) ;
#20498 = CARTESIAN_POINT ( 'NONE',  ( 107.3571765045248299, -2.791137627527939813, -8.388885654883777576 ) ) ;
#20499 = AXIS2_PLACEMENT_3D ( 'NONE', #9683, #16759, #9918 ) ;
#20500 = EDGE_CURVE ( 'NONE', #19315, #30808, #9555, .T. ) ;
#20501 = CARTESIAN_POINT ( 'NONE',  ( 111.8319081442453182, -4.153390946401321671, -8.397313243818183892 ) ) ;
#20502 = DIRECTION ( 'NONE',  ( -0.9063289528979890930, -0.4225728684367167087, 0.000000000000000000 ) ) ;
#20503 = ORIENTED_EDGE ( 'NONE', *, *, #3058, .F. ) ;
#20504 = CARTESIAN_POINT ( 'NONE',  ( 118.6391081442452986, -4.089484607189486809, -7.948022111789456723 ) ) ;
#20505 = CARTESIAN_POINT ( 'NONE',  ( 121.0630641859119976, -0.8832429491016019485, -18.19431474523657855 ) ) ;
#20506 = CARTESIAN_POINT ( 'NONE',  ( 114.3846081442453197, -10.63000616557722466, -14.87417383870573495 ) ) ;
#20507 = ORIENTED_EDGE ( 'NONE', *, *, #41247, .F. ) ;
#20508 = CONICAL_SURFACE ( 'NONE', #26321, 2.541999999999999371, 1.047197551196596299 ) ;
#20509 = CARTESIAN_POINT ( 'NONE',  ( 125.9568481442452850, -6.344957434206665248, -7.627207830600338134 ) ) ;
#20510 = DIRECTION ( 'NONE',  ( -0.000000000000000000, -0.9284778069183718952, -0.3713878862591649677 ) ) ;
#20511 = CARTESIAN_POINT ( 'NONE',  ( 113.4202548109119846, 0.1319031606808879209, -14.10382304977623669 ) ) ;
#20512 = CARTESIAN_POINT ( 'NONE',  ( 78.03418817537199459, -57.63411461863086060, -0.9907621434124950222 ) ) ;
#20513 = CARTESIAN_POINT ( 'NONE',  ( 115.1220548109119761, -1.833838273342658809, -17.42832698103878286 ) ) ;
#20514 = LINE ( 'NONE', #6828, #15626 ) ;
#20515 = CARTESIAN_POINT ( 'NONE',  ( 116.3133148109120043, -2.084020599724406786, -8.691656652584148546 ) ) ;
#20516 = CARTESIAN_POINT ( 'NONE',  ( 71.02242295334774269, -61.55231263772585493, -40.92852729658892486 ) ) ;
#20517 = CARTESIAN_POINT ( 'NONE',  ( 114.4980614775786734, -2.084020599724406786, -8.691656652584148546 ) ) ;
#20518 = CARTESIAN_POINT ( 'NONE',  ( 121.5492360609119800, -6.564341423271550902, -7.887810678476487425 ) ) ;
#20519 = CARTESIAN_POINT ( 'NONE',  ( 114.6115148109119986, -3.383040157471821630, -19.15922257007629170 ) ) ;
#20520 = CARTESIAN_POINT ( 'NONE',  ( 125.4463081442452932, -5.638512984488999180, -18.83840828888717311 ) ) ;
#20521 = CARTESIAN_POINT ( 'NONE',  ( 118.5823814775786360, -7.643976991954077427, -18.09477374809248928 ) ) ;
#20522 = ORIENTED_EDGE ( 'NONE', *, *, #37928, .F. ) ;
#20523 = CARTESIAN_POINT ( 'NONE',  ( 112.2289948109119848, -1.834011780172310813, -8.268836392978581529 ) ) ;
#20524 = CARTESIAN_POINT ( 'NONE',  ( 106.1070202545248407, -10.62599879583958717, -15.77991374673208469 ) ) ;
#20525 = DIRECTION ( 'NONE',  ( 0.000000000000000000, 0.000000000000000000, 1.000000000000000000 ) ) ;
#20526 = DIRECTION ( 'NONE',  ( -0.8949343913984424415, -0.1703803081152067966, 0.4123869368673871993 ) ) ;
#20527 = VECTOR ( 'NONE', #44951, 1000.000000000000000 ) ;
#20528 = CARTESIAN_POINT ( 'NONE',  ( 64.33303459182538120, -36.44494369579175697, -5.635745537283291640 ) ) ;
#20529 = CARTESIAN_POINT ( 'NONE',  ( 123.3474214775786209, -9.988377603198976828, -10.36322818467138340 ) ) ;
#20530 = ORIENTED_EDGE ( 'NONE', *, *, #25373, .T. ) ;
#20531 = CARTESIAN_POINT ( 'NONE',  ( 120.7039275888224097, -2.372251574601201174, -17.96033910819751611 ) ) ;
#20532 = CARTESIAN_POINT ( 'NONE',  ( 117.9016614775786280, -0.1624402480850797581, -16.17319339645315424 ) ) ;
#20533 = CARTESIAN_POINT ( 'NONE',  ( 124.7655881442452852, -9.859900752359376241, -12.68260735090040114 ) ) ;
#20534 = CARTESIAN_POINT ( 'NONE',  ( 122.8368814775786291, -1.561330072975668948, -17.79121239304076951 ) ) ;
#20535 = CARTESIAN_POINT ( 'NONE',  ( 107.9128015045248219, -2.477300249445798297, -7.631215200338321125 ) ) ;
#20536 = CARTESIAN_POINT ( 'NONE',  ( 89.08937694410278141, -10.53878037750923546, -14.12219449423614037 ) ) ;
#20537 = ORIENTED_EDGE ( 'NONE', *, *, #9989, .F. ) ;
#20538 = CARTESIAN_POINT ( 'NONE',  ( 111.7751814775786556, -7.893985811506177619, -18.51759400769804742 ) ) ;
#20539 = CIRCLE ( 'NONE', #6706, 15.90000000000000036 ) ;
#20540 = CARTESIAN_POINT ( 'NONE',  ( 125.7866681442452688, -8.899110576539710493, -16.42337572283490132 ) ) ;
#20541 = CARTESIAN_POINT ( 'NONE',  ( 122.2128881442453263, -1.834011780172310813, -8.268836392978581529 ) ) ;
#20542 = CARTESIAN_POINT ( 'NONE',  ( 116.3133148109120043, -2.084020599724406786, -8.691656652584148546 ) ) ;
#20543 = CARTESIAN_POINT ( 'NONE',  ( 112.1722681442453222, -8.899110576539710493, -16.42337572283490132 ) ) ;
#20544 = CARTESIAN_POINT ( 'NONE',  ( 117.4478481442453131, 0.2603800115204892296, -16.42320221600525088 ) ) ;
#20545 = DIRECTION ( 'NONE',  ( 0.000000000000000000, 0.9284778069183720062, 0.3713878862591650232 ) ) ;
#20546 = CARTESIAN_POINT ( 'NONE',  ( 127.9806007748781838, -1.226557776704764624, -8.771704985610853100 ) ) ;
#20547 = CARTESIAN_POINT ( 'NONE',  ( 123.8579614775786126, -9.859900752359378018, -12.68260735090039759 ) ) ;
#20548 = VERTEX_POINT ( 'NONE', #40156 ) ;
#20549 = DIRECTION ( 'NONE',  ( 0.000000000000000000, -0.9242245927363027524, -0.3818493186865929978 ) ) ;
#20550 = CARTESIAN_POINT ( 'NONE',  ( 117.9583881442453048, -10.30919188438810075, -12.61870101168855918 ) ) ;
#20551 = CARTESIAN_POINT ( 'NONE',  ( 123.3474214775786209, -0.1624402480850797581, -16.17319339645315424 ) ) ;
#20552 = VERTEX_POINT ( 'NONE', #29891 ) ;
#20553 = CARTESIAN_POINT ( 'NONE',  ( 123.2855641859119942, -0.8832429491016019485, -18.19431474523657855 ) ) ;
#20554 = CARTESIAN_POINT ( 'NONE',  ( 61.46741937898128327, -12.47125186204822178, -9.654607599614944746 ) ) ;
#20555 = CARTESIAN_POINT ( 'NONE',  ( 123.7445081442452874, -1.561330072975668948, -17.79121239304076951 ) ) ;
#20556 = CARTESIAN_POINT ( 'NONE',  ( 109.6491296295247793, -4.863998795839590272, -19.15521520033831493 ) ) ;
#20557 = CARTESIAN_POINT ( 'NONE',  ( 120.9081748109119872, -4.153390946401325223, -8.397313243818185668 ) ) ;
#20558 = EDGE_CURVE ( 'NONE', #33021, #29611, #8960, .T. ) ;
#20559 = VERTEX_POINT ( 'NONE', #8689 ) ;
#20560 = EDGE_LOOP ( 'NONE', ( #32908, #4150, #10345, #43019 ) ) ;
#20561 = AXIS2_PLACEMENT_3D ( 'NONE', #13062, #33549, #40882 ) ;
#20562 = CARTESIAN_POINT ( 'NONE',  ( 113.9875214775786532, -0.4660016031367893996, -10.09054647747474043 ) ) ;
#20563 = CARTESIAN_POINT ( 'NONE',  ( 125.6732148109119862, -9.859900752359378018, -12.68260735090039759 ) ) ;
#20564 = CARTESIAN_POINT ( 'NONE',  ( 125.4584548109119737, -4.863998795839242995, -13.39321520033831447 ) ) ;
#20565 = CARTESIAN_POINT ( 'NONE',  ( 59.92022724782403742, -14.76985616374063426, -18.18981531286807041 ) ) ;
#20566 = ADVANCED_FACE ( 'NONE', ( #40383 ), #27194, .T. ) ;
#20567 = CARTESIAN_POINT ( 'NONE',  ( 120.6812681442452941, -10.30919188438810075, -12.61870101168855918 ) ) ;
#20568 = DIRECTION ( 'NONE',  ( -0.8636456077245090457, 0.5040994586965585889, 0.000000000000000000 ) ) ;
#20569 = CIRCLE ( 'NONE', #24952, 5.999999999999997335 ) ;
#20570 = FACE_OUTER_BOUND ( 'NONE', #45080, .T. ) ;
#20571 = CARTESIAN_POINT ( 'NONE',  ( 121.3619881442452879, -4.089484607189486809, -7.948022111789456723 ) ) ;
#20573 = CARTESIAN_POINT ( 'NONE',  ( 118.3554748109119998, -9.565557343593413364, -10.61323700422348004 ) ) ;
#20572 = CARTESIAN_POINT ( 'NONE',  ( 117.6747548109119919, -1.834011780172310813, -8.268836392978581529 ) ) ;
#20574 = CARTESIAN_POINT ( 'NONE',  ( 69.36136150295220659, -57.19420113100166958, -32.97568258837489452 ) ) ;
#20575 = CARTESIAN_POINT ( 'NONE',  ( 115.6893214775786447, 0.5811942927096154232, -14.16772938898807155 ) ) ;
#20576 = EDGE_LOOP ( 'NONE', ( #23588, #43544, #25761, #18502 ) ) ;
#20577 = CARTESIAN_POINT ( 'NONE',  ( 113.1933481442453058, -4.089484607189486809, -7.948022111789456723 ) ) ;
#20578 = CARTESIAN_POINT ( 'NONE',  ( 124.9252281442453238, -8.862178061931794915, -16.39564131203325559 ) ) ;
#20579 = CARTESIAN_POINT ( 'NONE',  ( 106.4542858795248179, -0.7896495226426338832, -17.46756447353520159 ) ) ;
#20580 = CARTESIAN_POINT ( 'NONE',  ( 107.3571765045248299, -2.791137627527939813, -8.388885654883777576 ) ) ;
#20581 = CARTESIAN_POINT ( 'NONE',  ( 107.8433483795247838, -0.7896495226426338832, -9.318865927141430916 ) ) ;
#20582 = CARTESIAN_POINT ( 'NONE',  ( 120.9649014775786355, -3.383040157471821630, -19.15922257007629170 ) ) ;
#20583 = CARTESIAN_POINT ( 'NONE',  ( 124.1983214775786166, -1.833838273342659697, -17.42832698103878286 ) ) ;
#20584 = VERTEX_POINT ( 'NONE', #30121 ) ;
#20585 = EDGE_CURVE ( 'NONE', #14378, #16340, #22073, .T. ) ;
#20586 = CARTESIAN_POINT ( 'NONE',  ( 123.5176014775786228, -9.261995988541697145, -16.69588392320189030 ) ) ;
#20587 = CARTESIAN_POINT ( 'NONE',  ( 111.1076452545248259, 0.8980012041604421569, -11.00651665394454071 ) ) ;
#20588 = CARTESIAN_POINT ( 'NONE',  ( 119.7434548109119703, -4.863998795839242995, -13.39321520033831447 ) ) ;
#20589 = CARTESIAN_POINT ( 'NONE',  ( 122.8936081442453059, 0.2603800115204892296, -16.42320221600525088 ) ) ;
#20590 =( BOUNDED_SURFACE ( )  B_SPLINE_SURFACE ( 1, 2, ( 
 ( #39371, #36604, #19296, #1951, #35933, #4701, #30230, #36825, #40958, #40499, #12460, #16560, #26361, #5594, #6285, #20206, #5820, #43685, #30002, #6515, #12687, #37049, #27041, #16788, #30455, #40268, #9713, #9260, #27271, #19518, #41185, #34091, #16099, #23170, #16328, #37280, #44375, #9035, #22932, #37745, #17014, #13366, #23859, #19740, #23626, #30684, #26586, #9945, #37512, #13137, #33624, #33395, #20430, #6047, #3087, #2169, #2400, #44152, #43918, #2627, #12917, #2857, #19970, #33858, #34314, #26813, #40724, #9481, #23394, #44603, #14472, #27495, #3748, #21312, #41415, #115, #28164, #562, #27719, #21083, #7622, #4199, #7394, #38400, #28380, #34960, #20870, #17670, #13808, #30905, #13585, #24299, #11055, #38186, #10612, #3309, #6745, #44827, #6963, #34531, #10169, #31566, #17232, #34748, #45048, #31123, #41634, #24729, #42074, #10390, #3971, #38617, #42293, #3530, #35195, #14028, #37969, #17446, #31341, #27942, #24076, #335, #35423, #20654, #41852, #31790, #17893, #24515, #7173, #14248, #10832, #24958, #38854, #21536, #18567, #29275, #25189, #4874, #8083, #39759, #18792, #29497, #39087, #14924, #29053, #8529, #15146, #22431, #11727, #26079, #14697, #18117, #42960, #7856, #39983, #15371, #43191, #25853, #1450, #8305, #12178 ),
 ( #39314, #36324, #11955, #5093, #15594, #25641, #1671, #19009, #39544, #21985, #32895, #43411, #4428, #11510, #22207, #36103, #32681, #28835, #8748, #28611, #42520, #22654, #35654, #36550, #21762, #32010, #35874, #774, #18344, #11281, #32237, #1008, #42745, #25414, #4645, #32459, #1234, #2808, #13087, #29952, #44328, #26985, #36772, #40905, #23116, #26764, #19460, #30631, #44099, #15820, #41136, #30181, #1892, #9659, #29719, #23579, #6234, #12864, #19684, #33572, #33343, #36993, #40673, #9895, #5324, #2116, #5763, #22878, #9425, #9207, #5997, #23338, #37223, #27218, #8980, #16046, #2348, #16279, #19920, #34039, #43632, #33806, #37461, #12406, #2577, #16507, #20156, #43867, #30406, #23807, #19240, #16735, #44547, #13311, #33123, #40445, #26307, #12639, #40215, #5543, #26535, #17840, #45000, #17401, #10123, #13537, #11004, #13760, #41367, #38350, #38138, #63, #3485, #24458, #27669, #13976, #10561, #3039, #42017, #31290, #31513, #17183, #16961, #285, #6909, #42240, #44778, #27445, #37695, #6468, #28113, #41582, #21261, #27889, #7126, #20819, #30855, #20378, #10782, #3921, #24245, #34698, #41803, #21037, #24026, #34910, #34479, #34264, #3700, #37915, #6692, #14195, #24678, #10341, #20604, #3258, #507, #31073, #17620, #38566, #7342 ) ),
 .UNSPECIFIED., .F., .F., .T. ) 
 B_SPLINE_SURFACE_WITH_KNOTS ( ( 2, 2 ),
 ( 3, 2, 2, 2, 2, 2, 2, 2, 2, 2, 2, 2, 2, 2, 2, 2, 2, 2, 2, 2, 2, 2, 2, 2, 2, 2, 2, 2, 2, 2, 2, 2, 2, 2, 2, 2, 2, 2, 2, 2, 2, 2, 2, 2, 2, 2, 2, 2, 2, 2, 2, 2, 2, 2, 2, 2, 2, 2, 2, 2, 2, 2, 2, 2, 2, 2, 2, 2, 2, 2, 2, 2, 2, 2, 2, 2, 2, 2, 2, 2, 3 ),
 ( 0.000000000000000000, 1.000000000000000000 ),
 ( 0.000000000000000000, 0.01250000000000000069, 0.02500000000000000139, 0.03749999999999999861, 0.05000000000000000278, 0.06250000000000000000, 0.07499999999999999722, 0.08749999999999999445, 0.1000000000000000056, 0.1125000000000000028, 0.1250000000000000000, 0.1375000000000000111, 0.1499999999999999944, 0.1625000000000000056, 0.1749999999999999889, 0.1875000000000000000, 0.2000000000000000111, 0.2124999999999999944, 0.2250000000000000056, 0.2374999999999999889, 0.2500000000000000000, 0.2625000000000000111, 0.2750000000000000222, 0.2874999999999999778, 0.2999999999999999889, 0.3125000000000000000, 0.3250000000000000111, 0.3375000000000000222, 0.3499999999999999778, 0.3624999999999999889, 0.3750000000000000000, 0.3875000000000000111, 0.4000000000000000222, 0.4124999999999999778, 0.4249999999999999889, 0.4375000000000000000, 0.4500000000000000111, 0.4625000000000000222, 0.4749999999999999778, 0.4874999999999999889, 0.5000000000000000000, 0.5124999999999999556, 0.5250000000000000222, 0.5374999999999999778, 0.5500000000000000444, 0.5625000000000000000, 0.5749999999999999556, 0.5875000000000000222, 0.5999999999999999778, 0.6125000000000000444, 0.6250000000000000000, 0.6374999999999999556, 0.6500000000000000222, 0.6624999999999999778, 0.6750000000000000444, 0.6875000000000000000, 0.6999999999999999556, 0.7125000000000000222, 0.7249999999999999778, 0.7375000000000000444, 0.7500000000000000000, 0.7624999999999999556, 0.7750000000000000222, 0.7874999999999999778, 0.8000000000000000444, 0.8125000000000000000, 0.8249999999999999556, 0.8375000000000000222, 0.8499999999999999778, 0.8625000000000000444, 0.8750000000000000000, 0.8874999999999999556, 0.9000000000000000222, 0.9124999999999999778, 0.9250000000000000444, 0.9375000000000000000, 0.9499999999999999556, 0.9625000000000000222, 0.9749999999999999778, 0.9875000000000000444, 1.000000000000000000 ),
 .UNSPECIFIED. ) 
 GEOMETRIC_REPRESENTATION_ITEM ( )  RATIONAL_B_SPLINE_SURFACE ( (
 ( 1.000000000000000000, 0.9238795325112869605, 1.000000000000000000, 0.9238795325112869605, 1.000000000000000000, 0.9238795325112869605, 1.000000000000000000, 0.9238795325112869605, 1.000000000000000000, 0.9238795325112869605, 1.000000000000000000, 0.9238795325112869605, 1.000000000000000000, 0.9238795325112869605, 1.000000000000000000, 0.9238795325112869605, 1.000000000000000000, 0.9238795325112869605, 1.000000000000000000, 0.9238795325112869605, 1.000000000000000000, 0.9238795325112869605, 1.000000000000000000, 0.9238795325112869605, 1.000000000000000000, 0.9238795325112869605, 1.000000000000000000, 0.9238795325112869605, 1.000000000000000000, 0.9238795325112869605, 1.000000000000000000, 0.9238795325112869605, 1.000000000000000000, 0.9238795325112869605, 1.000000000000000000, 0.9238795325112869605, 1.000000000000000000, 0.9238795325112869605, 1.000000000000000000, 0.9238795325112869605, 1.000000000000000000, 0.9238795325112869605, 1.000000000000000000, 0.9238795325112869605, 1.000000000000000000, 0.9238795325112869605, 1.000000000000000000, 0.9238795325112869605, 1.000000000000000000, 0.9238795325112869605, 1.000000000000000000, 0.9238795325112869605, 1.000000000000000000, 0.9238795325112869605, 1.000000000000000000, 0.9238795325112869605, 1.000000000000000000, 0.9238795325112869605, 1.000000000000000000, 0.9238795325112869605, 1.000000000000000000, 0.9238795325112869605, 1.000000000000000000, 0.9238795325112869605, 1.000000000000000000, 0.9238795325112869605, 1.000000000000000000, 0.9238795325112869605, 1.000000000000000000, 0.9238795325112869605, 1.000000000000000000, 0.9238795325112869605, 1.000000000000000000, 0.9238795325112869605, 1.000000000000000000, 0.9238795325112869605, 1.000000000000000000, 0.9238795325112869605, 1.000000000000000000, 0.9238795325112869605, 1.000000000000000000, 0.9238795325112869605, 1.000000000000000000, 0.9238795325112869605, 1.000000000000000000, 0.9238795325112869605, 1.000000000000000000, 0.9238795325112869605, 1.000000000000000000, 0.9238795325112869605, 1.000000000000000000, 0.9238795325112869605, 1.000000000000000000, 0.9238795325112869605, 1.000000000000000000, 0.9238795325112869605, 1.000000000000000000, 0.9238795325112869605, 1.000000000000000000, 0.9238795325112869605, 1.000000000000000000, 0.9238795325112869605, 1.000000000000000000, 0.9238795325112869605, 1.000000000000000000, 0.9238795325112869605, 1.000000000000000000, 0.9238795325112869605, 1.000000000000000000, 0.9238795325112869605, 1.000000000000000000, 0.9238795325112869605, 1.000000000000000000, 0.9238795325112869605, 1.000000000000000000, 0.9238795325112869605, 1.000000000000000000, 0.9238795325112869605, 1.000000000000000000, 0.9238795325112869605, 1.000000000000000000, 0.9238795325112869605, 1.000000000000000000, 0.9238795325112869605, 1.000000000000000000, 0.9238795325112869605, 1.000000000000000000, 0.9238795325112869605, 1.000000000000000000, 0.9238795325112869605, 1.000000000000000000, 0.9238795325112869605, 1.000000000000000000, 0.9238795325112869605, 1.000000000000000000, 0.9238795325112869605, 1.000000000000000000, 0.9238795325112869605, 1.000000000000000000, 0.9238795325112869605, 1.000000000000000000, 0.9238795325112869605, 1.000000000000000000, 0.9238795325112869605, 1.000000000000000000, 0.9238795325112869605, 1.000000000000000000, 0.9238795325112869605, 1.000000000000000000, 0.9238795325112869605, 1.000000000000000000, 0.9238795325112869605, 1.000000000000000000, 0.9238795325112869605, 1.000000000000000000, 0.9238795325112869605, 1.000000000000000000, 0.9238795325112869605, 1.000000000000000000, 0.9238795325112869605, 1.000000000000000000),
 ( 1.000000000000000000, 0.9238795325112869605, 1.000000000000000000, 0.9238795325112869605, 1.000000000000000000, 0.9238795325112869605, 1.000000000000000000, 0.9238795325112869605, 1.000000000000000000, 0.9238795325112869605, 1.000000000000000000, 0.9238795325112869605, 1.000000000000000000, 0.9238795325112869605, 1.000000000000000000, 0.9238795325112869605, 1.000000000000000000, 0.9238795325112869605, 1.000000000000000000, 0.9238795325112869605, 1.000000000000000000, 0.9238795325112869605, 1.000000000000000000, 0.9238795325112869605, 1.000000000000000000, 0.9238795325112869605, 1.000000000000000000, 0.9238795325112869605, 1.000000000000000000, 0.9238795325112869605, 1.000000000000000000, 0.9238795325112869605, 1.000000000000000000, 0.9238795325112869605, 1.000000000000000000, 0.9238795325112869605, 1.000000000000000000, 0.9238795325112869605, 1.000000000000000000, 0.9238795325112869605, 1.000000000000000000, 0.9238795325112869605, 1.000000000000000000, 0.9238795325112869605, 1.000000000000000000, 0.9238795325112869605, 1.000000000000000000, 0.9238795325112869605, 1.000000000000000000, 0.9238795325112869605, 1.000000000000000000, 0.9238795325112869605, 1.000000000000000000, 0.9238795325112869605, 1.000000000000000000, 0.9238795325112869605, 1.000000000000000000, 0.9238795325112869605, 1.000000000000000000, 0.9238795325112869605, 1.000000000000000000, 0.9238795325112869605, 1.000000000000000000, 0.9238795325112869605, 1.000000000000000000, 0.9238795325112869605, 1.000000000000000000, 0.9238795325112869605, 1.000000000000000000, 0.9238795325112869605, 1.000000000000000000, 0.9238795325112869605, 1.000000000000000000, 0.9238795325112869605, 1.000000000000000000, 0.9238795325112869605, 1.000000000000000000, 0.9238795325112869605, 1.000000000000000000, 0.9238795325112869605, 1.000000000000000000, 0.9238795325112869605, 1.000000000000000000, 0.9238795325112869605, 1.000000000000000000, 0.9238795325112869605, 1.000000000000000000, 0.9238795325112869605, 1.000000000000000000, 0.9238795325112869605, 1.000000000000000000, 0.9238795325112869605, 1.000000000000000000, 0.9238795325112869605, 1.000000000000000000, 0.9238795325112869605, 1.000000000000000000, 0.9238795325112869605, 1.000000000000000000, 0.9238795325112869605, 1.000000000000000000, 0.9238795325112869605, 1.000000000000000000, 0.9238795325112869605, 1.000000000000000000, 0.9238795325112869605, 1.000000000000000000, 0.9238795325112869605, 1.000000000000000000, 0.9238795325112869605, 1.000000000000000000, 0.9238795325112869605, 1.000000000000000000, 0.9238795325112869605, 1.000000000000000000, 0.9238795325112869605, 1.000000000000000000, 0.9238795325112869605, 1.000000000000000000, 0.9238795325112869605, 1.000000000000000000, 0.9238795325112869605, 1.000000000000000000, 0.9238795325112869605, 1.000000000000000000, 0.9238795325112869605, 1.000000000000000000, 0.9238795325112869605, 1.000000000000000000, 0.9238795325112869605, 1.000000000000000000, 0.9238795325112869605, 1.000000000000000000, 0.9238795325112869605, 1.000000000000000000, 0.9238795325112869605, 1.000000000000000000, 0.9238795325112869605, 1.000000000000000000, 0.9238795325112869605, 1.000000000000000000, 0.9238795325112869605, 1.000000000000000000, 0.9238795325112869605, 1.000000000000000000, 0.9238795325112869605, 1.000000000000000000, 0.9238795325112869605, 1.000000000000000000, 0.9238795325112869605, 1.000000000000000000, 0.9238795325112869605, 1.000000000000000000, 0.9238795325112869605, 1.000000000000000000, 0.9238795325112869605, 1.000000000000000000, 0.9238795325112869605, 1.000000000000000000, 0.9238795325112869605, 1.000000000000000000) ) ) 
 REPRESENTATION_ITEM ( '' )  SURFACE ( )  );
#20591 = EDGE_CURVE ( 'NONE', #35835, #43568, #5304, .T. ) ;
#20592 = CARTESIAN_POINT ( 'NONE',  ( 77.05532149770296257, 0.06670422450934243574, -16.89321520033831447 ) ) ;
#20593 = CARTESIAN_POINT ( 'NONE',  ( 119.6045485609119794, -0.08252387247370887580, -11.91645802438286417 ) ) ;
#20594 = CARTESIAN_POINT ( 'NONE',  ( 113.9875214775786532, -0.4660016031367893996, -10.09054647747474043 ) ) ;
#20595 = AXIS2_PLACEMENT_3D ( 'NONE', #28949, #42857, #42187 ) ;
#20596 = CARTESIAN_POINT ( 'NONE',  ( 111.7688629525735706, -1.111561923218670422, -17.14115599315433869 ) ) ;
#20597 = CARTESIAN_POINT ( 'NONE',  ( 114.6497546295247929, -4.863998795839590272, -18.39754474579285315 ) ) ;
#20598 = ORIENTED_EDGE ( 'NONE', *, *, #41658, .T. ) ;
#20599 = CARTESIAN_POINT ( 'NONE',  ( 123.9584548109119737, 3.074545301078819737, -12.40350937470759973 ) ) ;
#20600 = CARTESIAN_POINT ( 'NONE',  ( 112.4559014775786778, -0.1624402480850797581, -16.17319339645315424 ) ) ;
#20601 = AXIS2_PLACEMENT_3D ( 'NONE', #9937, #17008, #23386 ) ;
#20602 = CARTESIAN_POINT ( 'NONE',  ( 112.1155414775786454, 0.9020085738987339008, -11.91225656197089222 ) ) ;
#20603 = CARTESIAN_POINT ( 'NONE',  ( 107.4960827545248350, -6.936859964151250502, -8.388885654883777576 ) ) ;
#20604 = CARTESIAN_POINT ( 'NONE',  ( 105.3430358795248338, -8.402594152722688392, -9.854619843455216355 ) ) ;
#20605 = CARTESIAN_POINT ( 'NONE',  ( 120.1707281442453166, -9.565557343593413364, -10.61323700422348004 ) ) ;
#20606 = CARTESIAN_POINT ( 'NONE',  ( 116.9940348109119839, -0.1624402480850797581, -16.17319339645315424 ) ) ;
#20607 = CARTESIAN_POINT ( 'NONE',  ( 113.4202548109119846, 0.1319031606808879209, -14.10382304977623669 ) ) ;
#20608 = ORIENTED_EDGE ( 'NONE', *, *, #26430, .T. ) ;
#20609 = PRODUCT_DEFINITION_FORMATION_WITH_SPECIFIED_SOURCE ( 'ANY', '', #21957, .NOT_KNOWN. ) ;
#20610 = CARTESIAN_POINT ( 'NONE',  ( 124.5954081442453116, -6.222761293078241884, -8.102969835052219238 ) ) ;
#20611 = AXIS2_PLACEMENT_3D ( 'NONE', #40234, #39778, #19704 ) ;
#20612 = CARTESIAN_POINT ( 'NONE',  ( 118.1852948109119836, -5.638512984488999180, -18.83840828888717311 ) ) ;
#20613 = CARTESIAN_POINT ( 'NONE',  ( 125.5030348109119558, -6.222761293078241884, -8.102969835052219238 ) ) ;
#20614 = VERTEX_POINT ( 'NONE', #40842 ) ;
#20615 = CARTESIAN_POINT ( 'NONE',  ( 126.2872529661387091, -9.070044156411084302, -16.15989887877886133 ) ) ;
#20616 = EDGE_LOOP ( 'NONE', ( #1435, #6239, #12068, #24613, #41995 ) ) ;
#20617 = CARTESIAN_POINT ( 'NONE',  ( 116.6536748109119941, -10.15424416112533912, -14.75197769757731336 ) ) ;
#20618 = CARTESIAN_POINT ( 'NONE',  ( 113.4769814775786330, 0.4262465694468514643, -12.03445270309931736 ) ) ;
#20619 = CARTESIAN_POINT ( 'NONE',  ( 115.1787814775786529, -9.988377603198973276, -10.36322818467138163 ) ) ;
#20620 = CARTESIAN_POINT ( 'NONE',  ( 120.3685329359119862, -4.283928203966213211, -7.183505701512925334 ) ) ;
#20621 = ORIENTED_EDGE ( 'NONE', *, *, #19855, .T. ) ;
#20622 = VECTOR ( 'NONE', #10720, 1000.000000000000114 ) ;
#20623 = DIRECTION ( 'NONE',  ( 0.000000000000000000, -0.9242245927363029745, -0.3818493186865927758 ) ) ;
#20624 = DIRECTION ( 'NONE',  ( 0.000000000000000000, 0.3818493186865927203, -0.9242245927363029745 ) ) ;
#20625 = ADVANCED_FACE ( 'NONE', ( #23050 ), #26478, .F. ) ;
#20626 = CARTESIAN_POINT ( 'NONE',  ( 114.3719421295247827, 0.8980012041604618078, -13.39321520033831447 ) ) ;
#20627 = CARTESIAN_POINT ( 'NONE',  ( 117.9417709814547095, -2.395992375830784837, -17.92872468182854107 ) ) ;
#20628 = CARTESIAN_POINT ( 'NONE',  ( 122.6667014775786413, -2.084020599724406786, -8.691656652584148546 ) ) ;
#20629 = CARTESIAN_POINT ( 'NONE',  ( 114.1577014775786552, -3.505236298600246325, -18.68346056562440793 ) ) ;
#20630 = CARTESIAN_POINT ( 'NONE',  ( 113.8173414775786512, -9.565557343593411588, -10.61323700422346583 ) ) ;
#20631 = VERTEX_POINT ( 'NONE', #12574 ) ;
#20632 = CARTESIAN_POINT ( 'NONE',  ( 122.3620835773848654, -2.467220198592778413, -17.83387418641524391 ) ) ;
#20633 = CARTESIAN_POINT ( 'NONE',  ( 115.9947331777918862, -0.01829820670803256055, -14.64321520033831447 ) ) ;
#20634 = AXIS2_PLACEMENT_3D ( 'NONE', #21378, #25026, #4941 ) ;
#20635 = CARTESIAN_POINT ( 'NONE',  ( 122.5191809221557122, -2.372251574601201174, -17.96033910819751611 ) ) ;
#20636 = CARTESIAN_POINT ( 'NONE',  ( 111.5482748109120053, -0.1624402480850797581, -16.17319339645315424 ) ) ;
#20638 = CARTESIAN_POINT ( 'NONE',  ( 126.1837548109119211, -10.63000616557722466, -14.87417383870573495 ) ) ;
#20637 = CARTESIAN_POINT ( 'NONE',  ( 64.98167240748409768, -37.86052959031123777, -4.893215200338314474 ) ) ;
#20639 = CARTESIAN_POINT ( 'NONE',  ( 125.2761281442453054, 0.4262465694468514643, -12.03445270309931736 ) ) ;
#20640 = ORIENTED_EDGE ( 'NONE', *, *, #40516, .T. ) ;
#20641 = CARTESIAN_POINT ( 'NONE',  ( 114.2144281442453178, -8.166667518702817929, -8.995218007635859436 ) ) ;
#20642 = LINE ( 'NONE', #6732, #25328 ) ;
#20643 = CARTESIAN_POINT ( 'NONE',  ( 106.8710046295248759, -4.863998795839590272, -18.39754474579285315 ) ) ;
#20644 = EDGE_CURVE ( 'NONE', #5080, #38926, #10432, .T. ) ;
#20645 = CARTESIAN_POINT ( 'NONE',  ( 126.4673881442452910, -7.894159318335828068, -9.358103419637847864 ) ) ;
#20646 = CARTESIAN_POINT ( 'NONE',  ( 123.8012348109119642, -9.565557343593413364, -10.61323700422348004 ) ) ;
#20647 = LINE ( 'NONE', #44144, #23527 ) ;
#20648 = CARTESIAN_POINT ( 'NONE',  ( 112.2188952545247531, -9.868328341294098749, -15.46607636864997204 ) ) ;
#20649 = FACE_OUTER_BOUND ( 'NONE', #43767, .T. ) ;
#20650 = CARTESIAN_POINT ( 'NONE',  ( 112.3781902440515665, -2.467220198592768199, -17.83387418641523325 ) ) ;
#20651 = DIRECTION ( 'NONE',  ( 0.000000000000000000, -0.6004852223388321697, 0.7996358532186280677 ) ) ;
#20652 = DIRECTION ( 'NONE',  ( 0.1352586133457954198, 0.9908103287288503314, 0.000000000000000000 ) ) ;
#20653 = DIRECTION ( 'NONE',  ( 0.000000000000000000, -0.4669533266896290225, -0.8842819633428516957 ) ) ;
#20654 = CARTESIAN_POINT ( 'NONE',  ( 108.0517077545248696, -7.250697342233347165, -7.631215200338321125 ) ) ;
#20655 = CARTESIAN_POINT ( 'NONE',  ( 124.6521348109119884, -1.561330072975668948, -17.79121239304076951 ) ) ;
#20656 = CARTESIAN_POINT ( 'NONE',  ( 124.8223148109119762, 0.9020085738987339008, -11.91225656197089222 ) ) ;
#20657 = DIRECTION ( 'NONE',  ( -0.000000000000000000, -0.9284778069183721172, -0.3713878862591650232 ) ) ;
#20658 = EDGE_CURVE ( 'NONE', #27773, #27364, #12346, .T. ) ;
#20659 = CARTESIAN_POINT ( 'NONE',  ( 121.7023481442452777, -9.261995988541697145, -16.69588392320189030 ) ) ;
#20660 = CARTESIAN_POINT ( 'NONE',  ( 114.6682414775786469, -1.561330072975668060, -17.79121239304076596 ) ) ;
#20661 = ORIENTED_EDGE ( 'NONE', *, *, #11734, .T. ) ;
#20662 = CARTESIAN_POINT ( 'NONE',  ( 115.0086014775786509, -5.574606645277164318, -18.38911715685844683 ) ) ;
#20663 = AXIS2_PLACEMENT_3D ( 'NONE', #7546, #34072, #14851 ) ;
#20664 = CARTESIAN_POINT ( 'NONE',  ( 123.1205148109119563, -1.834011780172310813, -8.268836392978581529 ) ) ;
#20665 = CARTESIAN_POINT ( 'NONE',  ( 115.6893214775786447, 0.5811942927096154232, -14.16772938898807155 ) ) ;
#20666 = CARTESIAN_POINT ( 'NONE',  ( 116.9940348109119839, -0.1624402480850797581, -16.17319339645315424 ) ) ;
#20667 = ORIENTED_EDGE ( 'NONE', *, *, #20891, .F. ) ;
#20668 = CARTESIAN_POINT ( 'NONE',  ( 117.9016614775786280, -0.1624402480850797581, -16.17319339645315424 ) ) ;
#20669 = CIRCLE ( 'NONE', #37375, 1.500000000000000000 ) ;
#20670 = CARTESIAN_POINT ( 'NONE',  ( 115.8595014775786609, -1.834011780172310813, -8.268836392978581529 ) ) ;
#20671 = CARTESIAN_POINT ( 'NONE',  ( 124.9357681442453014, -7.643976991954077427, -18.09477374809248928 ) ) ;
#20672 = CARTESIAN_POINT ( 'NONE',  ( 116.8361907699537880, -1.174466963688203913, -17.11742336975050804 ) ) ;
#20673 = CARTESIAN_POINT ( 'NONE',  ( 112.9134265045247645, -7.250697342233347165, -19.15521520033831138 ) ) ;
#20674 = ORIENTED_EDGE ( 'NONE', *, *, #33820, .F. ) ;
#20675 = CARTESIAN_POINT ( 'NONE',  ( 65.53695226829334786, -0.2718670794236524024, -8.259322725476325289 ) ) ;
#20676 = CARTESIAN_POINT ( 'NONE',  ( 112.6609831777918913, -0.01829820670813664396, -14.64321520033831447 ) ) ;
#20677 = DIRECTION ( 'NONE',  ( 0.000000000000000000, 0.3713878862591650232, -0.9284778069183718952 ) ) ;
#20678 = CARTESIAN_POINT ( 'NONE',  ( 115.6893214775786447, 0.5811942927096154232, -14.16772938898807155 ) ) ;
#20679 = CARTESIAN_POINT ( 'NONE',  ( 112.6828081442453140, -7.893985811506177619, -18.51759400769804742 ) ) ;
#20680 = LINE ( 'NONE', #42096, #38200 ) ;
#20681 = CARTESIAN_POINT ( 'NONE',  ( 59.44377208703740223, -12.82110557137145967, -17.39288367676203606 ) ) ;
#20682 = EDGE_CURVE ( 'NONE', #23478, #20559, #35890, .T. ) ;
#20683 = CARTESIAN_POINT ( 'NONE',  ( 123.0760201386228800, -1.125321370491285444, -17.12283323191017814 ) ) ;
#20684 = CARTESIAN_POINT ( 'NONE',  ( 115.5526452545247622, -9.868328341294098749, -15.46607636864997204 ) ) ;
#20685 = CARTESIAN_POINT ( 'NONE',  ( 117.3911214775786505, -1.561330072975668504, -17.79121239304076951 ) ) ;
#20686 = CARTESIAN_POINT ( 'NONE',  ( 136.1634721355147803, -4.175307135294594296, -19.22903496993399841 ) ) ;
#20687 = DIRECTION ( 'NONE',  ( 0.000000000000000000, 0.4669533266896289669, 0.8842819633428516957 ) ) ;
#20688 = DIRECTION ( 'NONE',  ( 1.000000000000000000, 0.000000000000000000, -0.000000000000000000 ) ) ;
#20689 = CARTESIAN_POINT ( 'NONE',  ( 121.1350814775786233, -9.859900752359378018, -12.68260735090039759 ) ) ;
#20690 = ORIENTED_EDGE ( 'NONE', *, *, #8321, .F. ) ;
#20691 = CARTESIAN_POINT ( 'NONE',  ( 71.31713442278437753, 2.423123680056944007, -10.89321520033831447 ) ) ;
#20692 = CARTESIAN_POINT ( 'NONE',  ( 117.8449348109119938, -8.166667518702817929, -8.995218007635861213 ) ) ;
#20693 = CARTESIAN_POINT ( 'NONE',  ( 116.9417077545247992, -2.791137627527939813, -18.39754474579286025 ) ) ;
#20694 = CARTESIAN_POINT ( 'NONE',  ( 117.3343948109119737, -6.222761293078241884, -8.102969835052219238 ) ) ;
#20695 = CARTESIAN_POINT ( 'NONE',  ( 112.6260814775786514, -0.8288870151387760510, -10.36305467784173118 ) ) ;
#20696 = CARTESIAN_POINT ( 'NONE',  ( 111.5938171295247940, -10.62599879583958540, -13.39321520033831447 ) ) ;
#20697 = DIRECTION ( 'NONE',  ( 0.7400066460894876297, -0.6725995567522979890, -0.000000000000000000 ) ) ;
#20698 = CARTESIAN_POINT ( 'NONE',  ( 113.4690515045247992, -2.477300249445798297, -7.631215200338321125 ) ) ;
#20699 = CARTESIAN_POINT ( 'NONE',  ( 115.7460481442453357, -10.15424416112533912, -14.75197769757731336 ) ) ;
#20700 = CARTESIAN_POINT ( 'NONE',  ( 121.5888948109119809, 0.1319031606808879209, -14.10382304977623669 ) ) ;
#20701 = EDGE_CURVE ( 'NONE', #32144, #7030, #2408, .T. ) ;
#20702 = DIRECTION ( 'NONE',  ( 0.000000000000000000, 0.000000000000000000, -1.000000000000000000 ) ) ;
#20703 = CARTESIAN_POINT ( 'NONE',  ( 121.3408766859119794, -0.06289925094097943703, -9.412459353600674206 ) ) ;
#20704 = CARTESIAN_POINT ( 'NONE',  ( 107.7044421295247929, -9.868328341294093420, -13.39321520033831447 ) ) ;
#20705 = CARTESIAN_POINT ( 'NONE',  ( 109.2294433505451678, -0.4438500802042310012, -15.88352395893305413 ) ) ;
#20706 = CARTESIAN_POINT ( 'NONE',  ( 115.6325948109119821, 0.2603800115204892296, -16.42320221600525088 ) ) ;
#20707 = CARTESIAN_POINT ( 'NONE',  ( 114.1577014775786552, -6.344957434206662583, -7.627207830600332805 ) ) ;
#20708 = CARTESIAN_POINT ( 'NONE',  ( 122.6604860609119640, -3.387241619883791355, -18.17469012370385073 ) ) ;
#20709 = VERTEX_POINT ( 'NONE', #12121 ) ;
#20710 = CARTESIAN_POINT ( 'NONE',  ( 123.4721467849153527, -2.841504294525492913, -14.83747852055392968 ) ) ;
#20711 = ORIENTED_EDGE ( 'NONE', *, *, #3022, .F. ) ;
#20712 = CARTESIAN_POINT ( 'NONE',  ( 122.6099748109119929, -9.261995988541697145, -16.69588392320189030 ) ) ;
#20713 = CARTESIAN_POINT ( 'NONE',  ( 112.8529881442453302, -1.561330072975668060, -17.79121239304076596 ) ) ;
#20714 = CARTESIAN_POINT ( 'NONE',  ( 119.5467348109119712, -5.574606645277164318, -18.38911715685844683 ) ) ;
#20715 = DIRECTION ( 'NONE',  ( 0.000000000000000000, 0.000000000000000000, 1.000000000000000000 ) ) ;
#20716 = CARTESIAN_POINT ( 'NONE',  ( 121.2485348109119769, -0.4660016031367893996, -10.09054647747474043 ) ) ;
#20717 = CARTESIAN_POINT ( 'NONE',  ( 118.8092881442453290, -9.988377603198976828, -10.36322818467138340 ) ) ;
#20718 = AXIS2_PLACEMENT_3D ( 'NONE', #6379, #41930, #41274 ) ;
#20719 = CARTESIAN_POINT ( 'NONE',  ( 109.5102233795247884, -1.325403438956436419, -9.854619843455211026 ) ) ;
#20720 = CARTESIAN_POINT ( 'NONE',  ( 113.4769814775786330, 0.4262465694468514643, -12.03445270309931736 ) ) ;
#20721 = DIRECTION ( 'NONE',  ( 0.000000000000000000, -0.3818493186865927203, 0.9242245927363029745 ) ) ;
#20722 = ORIENTED_EDGE ( 'NONE', *, *, #27452, .T. ) ;
#20723 = CARTESIAN_POINT ( 'NONE',  ( 118.6958348109119754, -6.344957434206665248, -7.627207830600338134 ) ) ;
#20724 = CARTESIAN_POINT ( 'NONE',  ( 121.6186891859119896, -8.844754642576884152, -8.592115655440050404 ) ) ;
#20725 = CARTESIAN_POINT ( 'NONE',  ( 116.6536748109119941, 0.9020085738987339008, -11.91225656197089222 ) ) ;
#20726 = EDGE_LOOP ( 'NONE', ( #11504, #35481, #3880, #27732, #25141 ) ) ;
#20727 = CARTESIAN_POINT ( 'NONE',  ( 116.5944421295247793, 0.8980012041604618078, -13.39321520033831447 ) ) ;
#20728 = CARTESIAN_POINT ( 'NONE',  ( -13.90346622911622276, -4.337920416975670435, -8.893215200338337567 ) ) ;
#20729 = DIRECTION ( 'NONE',  ( 1.000000000000000000, 0.000000000000000000, 0.000000000000000000 ) ) ;
#20730 = DIRECTION ( 'NONE',  ( 0.000000000000000000, 0.000000000000000000, 1.000000000000000000 ) ) ;
#20731 = CYLINDRICAL_SURFACE ( 'NONE', #3984, 1.587500000000000355 ) ;
#20732 = CARTESIAN_POINT ( 'NONE',  ( 116.9373081442452929, -1.833838273342659253, -17.42832698103878286 ) ) ;
#20733 = DIRECTION ( 'NONE',  ( -1.000000000000000000, 0.000000000000000000, -0.000000000000000000 ) ) ;
#20734 = CARTESIAN_POINT ( 'NONE',  ( 118.4122014775786340, -9.859900752359374465, -12.68260735090039404 ) ) ;
#20735 = TOROIDAL_SURFACE ( 'NONE', #34545, 4.500000000000000000, 1.500000000000000000 ) ;
#20736 = PLANE ( 'NONE',  #8489 ) ;
#20737 = CARTESIAN_POINT ( 'NONE',  ( 118.5256548109119876, -8.899110576539710493, -16.42337572283490132 ) ) ;
#20738 = CARTESIAN_POINT ( 'NONE',  ( 121.4797829359119987, -4.283928203966213211, -7.183505701512925334 ) ) ;
#20739 = CARTESIAN_POINT ( 'NONE',  ( 116.6536748109119941, 0.9020085738987339008, -11.91225656197089222 ) ) ;
#20740 = CARTESIAN_POINT ( 'NONE',  ( 125.3895814775786448, -7.893985811506177619, -18.51759400769804742 ) ) ;
#20741 = AXIS2_PLACEMENT_3D ( 'NONE', #7474, #36190, #38707 ) ;
#20742 = CARTESIAN_POINT ( 'NONE',  ( 117.2209414775786485, -2.084020599724406786, -8.691656652584148546 ) ) ;
#20743 = ORIENTED_EDGE ( 'NONE', *, *, #15899, .T. ) ;
#20744 = CARTESIAN_POINT ( 'NONE',  ( 115.3489614775786407, -9.261995988541697145, -16.69588392320189030 ) ) ;
#20745 = CARTESIAN_POINT ( 'NONE',  ( 108.4684265045247997, -7.250697342233347165, -19.15521520033831138 ) ) ;
#20746 = CARTESIAN_POINT ( 'NONE',  ( 87.02785693856107230, -25.99489077589524300, -13.39321520033831447 ) ) ;
#20747 = CARTESIAN_POINT ( 'NONE',  ( 87.44708369096655076, -21.99489077589587538, -8.186108419151770121 ) ) ;
#20748 = ADVANCED_FACE ( 'NONE', ( #5264 ), #16983, .T. ) ;
#20749 = CARTESIAN_POINT ( 'NONE',  ( 113.6792791257774979, 0.2334052082820642360, -12.14321520033833046 ) ) ;
#20750 = CARTESIAN_POINT ( 'NONE',  ( 121.4754414775786131, -8.166667518702819706, -8.995218007635861213 ) ) ;
#20751 = VERTEX_POINT ( 'NONE', #29436 ) ;
#20752 = CARTESIAN_POINT ( 'NONE',  ( 118.4752466692503816, -2.311015703046731318, -18.04188382666268708 ) ) ;
#20753 = CARTESIAN_POINT ( 'NONE',  ( 117.2209414775786485, -2.084020599724406786, -8.691656652584148546 ) ) ;
#20754 = DIRECTION ( 'NONE',  ( -0.000000000000000000, -0.9284778069183721172, -0.3713878862591650232 ) ) ;
#20755 = CARTESIAN_POINT ( 'NONE',  ( 123.9800954359119913, -11.07370829466463391, -12.81314460846528469 ) ) ;
#20756 = CARTESIAN_POINT ( 'NONE',  ( 122.4397948109119767, -9.988377603198976828, -10.36322818467138340 ) ) ;
#20757 = CARTESIAN_POINT ( 'NONE',  ( 114.1635827545248389, -6.936859964151250502, -8.388885654883777576 ) ) ;
#20758 = CARTESIAN_POINT ( 'NONE',  ( 89.13851161028307502, -10.41525819279620357, -14.06723350770984382 ) ) ;
#20759 = EDGE_LOOP ( 'NONE', ( #1211, #8928, #15782, #21068 ) ) ;
#20760 = CARTESIAN_POINT ( 'NONE',  ( 113.1366214775786432, -1.834011780172310813, -8.268836392978581529 ) ) ;
#20761 = CARTESIAN_POINT ( 'NONE',  ( 112.2857214775786474, -4.089484607189486809, -7.948022111789456723 ) ) ;
#20762 = CARTESIAN_POINT ( 'NONE',  ( 123.6877814775786533, -3.383040157471821630, -19.15922257007629170 ) ) ;
#20763 = CARTESIAN_POINT ( 'NONE',  ( 118.2987481442453088, -7.894159318335828068, -9.358103419637847864 ) ) ;
#20764 = CARTESIAN_POINT ( 'NONE',  ( 83.02743615869442806, -30.94908174223593633, -21.89321520033831447 ) ) ;
#20765 = CARTESIAN_POINT ( 'NONE',  ( 118.3554748109119998, 0.2603800115204892296, -16.42320221600525088 ) ) ;
#20766 = CARTESIAN_POINT ( 'NONE',  ( 96.54708369096698561, -26.33989114581222424, -11.20947992683166916 ) ) ;
#20767 = CARTESIAN_POINT ( 'NONE',  ( 123.9714148109119805, -8.899110576539710493, -16.42337572283490132 ) ) ;
#20768 = ORIENTED_EDGE ( 'NONE', *, *, #40341, .F. ) ;
#20769 = AXIS2_PLACEMENT_3D ( 'NONE', #17149, #2773, #44510 ) ;
#20770 = DIRECTION ( 'NONE',  ( 0.000000000000000000, -0.3818493186865927203, 0.9242245927363029745 ) ) ;
#20771 = CARTESIAN_POINT ( 'NONE',  ( 116.1431348109119881, -10.30919188438810075, -12.61870101168855918 ) ) ;
#20772 = CARTESIAN_POINT ( 'NONE',  ( 123.6310548109119765, -4.153390946401325223, -8.397313243818185668 ) ) ;
#20773 = ORIENTED_EDGE ( 'NONE', *, *, #14051, .T. ) ;
#20774 = CARTESIAN_POINT ( 'NONE',  ( 83.44708369096697709, -26.60966817898065884, -11.90521360603286816 ) ) ;
#20775 = CARTESIAN_POINT ( 'NONE',  ( 136.7082020370487214, -1.261532916568094853, -9.046217426794857630 ) ) ;
#20776 = CARTESIAN_POINT ( 'NONE',  ( 123.9714148109119805, -0.4660016031367893996, -10.09054647747474043 ) ) ;
#20777 = AXIS2_PLACEMENT_3D ( 'NONE', #36056, #8482, #1624 ) ;
#20778 = CARTESIAN_POINT ( 'NONE',  ( 107.1488171295247867, -10.62599879583958540, -13.39321520033831447 ) ) ;
#20779 = CARTESIAN_POINT ( 'NONE',  ( 118.2987481442453088, -7.894159318335828068, -9.358103419637847864 ) ) ;
#20780 = ORIENTED_EDGE ( 'NONE', *, *, #10299, .F. ) ;
#20781 = VERTEX_POINT ( 'NONE', #33508 ) ;
#20782 = CARTESIAN_POINT ( 'NONE',  ( 113.7606148109119886, -1.561330072975668060, -17.79121239304076596 ) ) ;
#20783 = CARTESIAN_POINT ( 'NONE',  ( 124.4252281442452812, -0.8288870151387760510, -10.36305467784173118 ) ) ;
#20784 =( NAMED_UNIT ( * ) PLANE_ANGLE_UNIT ( ) SI_UNIT ( $, .RADIAN. ) );
#20785 = CARTESIAN_POINT ( 'NONE',  ( 67.30914723170953096, -56.02262229671700311, -36.50637067845163841 ) ) ;
#20786 = CARTESIAN_POINT ( 'NONE',  ( 121.3052614775786111, -1.834011780172310813, -8.268836392978581529 ) ) ;
#20787 = LINE ( 'NONE', #27636, #38602 ) ;
#20788 = CARTESIAN_POINT ( 'NONE',  ( 31.16203868753470019, 11.28474725185576055, -8.893215200338314474 ) ) ;
#20789 = PRODUCT_RELATED_PRODUCT_CATEGORY ( 'part', '', ( #3366 ) ) ;
#20790 = CARTESIAN_POINT ( 'NONE',  ( 120.9081748109119872, -5.638512984488999180, -18.83840828888717311 ) ) ;
#20792 = CARTESIAN_POINT ( 'NONE',  ( 118.6391081442452986, -5.574606645277164318, -18.38911715685844683 ) ) ;
#20791 = CARTESIAN_POINT ( 'NONE',  ( 117.8449348109119938, -8.166667518702817929, -8.995218007635861213 ) ) ;
#20793 = LINE ( 'NONE', #13951, #5048 ) ;
#20794 = CARTESIAN_POINT ( 'NONE',  ( 117.8449348109119938, -8.166667518702817929, -8.995218007635861213 ) ) ;
#20795 = EDGE_LOOP ( 'NONE', ( #33217, #39071, #17835, #23917, #26770, #2461, #20161, #27804, #15826, #7578 ) ) ;
#20796 = CARTESIAN_POINT ( 'NONE',  ( 125.5597614775786326, -7.894159318336616771, -9.358103419638441167 ) ) ;
#20797 = VECTOR ( 'NONE', #41334, 1000.000000000000114 ) ;
#20798 = CARTESIAN_POINT ( 'NONE',  ( 107.4960827545248350, -2.477300249445798297, -19.15521520033831138 ) ) ;
#20799 = CARTESIAN_POINT ( 'NONE',  ( 109.9963952545248134, -9.868328341294098749, -15.46607636864997204 ) ) ;
#20800 = CARTESIAN_POINT ( 'NONE',  ( 109.4407702545248355, -10.62599879583958717, -15.77991374673208469 ) ) ;
#20801 = DIRECTION ( 'NONE',  ( -0.000000000000000000, -0.9284778069183721172, -0.3713878862591650232 ) ) ;
#20802 = CARTESIAN_POINT ( 'NONE',  ( 126.4106614775786284, -6.222761293078241884, -8.102969835052219238 ) ) ;
#20803 = VERTEX_POINT ( 'NONE', #13023 ) ;
#20804 = CARTESIAN_POINT ( 'NONE',  ( 122.7234281442452755, -5.638512984488999180, -18.83840828888717311 ) ) ;
#20805 = CARTESIAN_POINT ( 'NONE',  ( 113.2606921295247702, 0.8980012041604618078, -13.39321520033831447 ) ) ;
#20806 = LINE ( 'NONE', #24666, #31417 ) ;
#20807 = CARTESIAN_POINT ( 'NONE',  ( 122.9503348109119827, 0.5811942927096110934, -14.16772938898807510 ) ) ;
#20808 = CARTESIAN_POINT ( 'NONE',  ( 125.3328548109119964, -9.261995988541697145, -16.69588392320189030 ) ) ;
#20810 = VECTOR ( 'NONE', #30705, 1000.000000000000000 ) ;
#20809 = CARTESIAN_POINT ( 'NONE',  ( 120.1569985609119726, -9.641336978641936284, -14.86869474514246647 ) ) ;
#20811 = CARTESIAN_POINT ( 'NONE',  ( 113.8173414775786512, 0.2603800115204892296, -16.42320221600525088 ) ) ;
#20812 = DIRECTION ( 'NONE',  ( -0.4461977533474358326, 0.3417300876246960328, -0.8271203734159366938 ) ) ;
#20813 = CARTESIAN_POINT ( 'NONE',  ( 106.3153796295248412, -4.863998795839590272, -19.15521520033831493 ) ) ;
#20814 = ORIENTED_EDGE ( 'NONE', *, *, #31182, .T. ) ;
#20815 = CYLINDRICAL_SURFACE ( 'NONE', #13569, 4.500000000000003553 ) ;
#20816 = CARTESIAN_POINT ( 'NONE',  ( 114.7816948109119863, -9.859900752359374465, -12.68260735090039404 ) ) ;
#20817 = CARTESIAN_POINT ( 'NONE',  ( 125.9001214775786224, -5.574606645277164318, -18.38911715685844683 ) ) ;
#20818 = CARTESIAN_POINT ( 'NONE',  ( 115.4137390045248566, 0.8980012041604421569, -15.77991374673208469 ) ) ;
#20819 = CARTESIAN_POINT ( 'NONE',  ( 106.6626452545248611, -9.868328341294098749, -15.46607636864997204 ) ) ;
#20820 = CARTESIAN_POINT ( 'NONE',  ( 120.3409081442453044, -8.899110576539710493, -16.42337572283490132 ) ) ;
#20821 = CARTESIAN_POINT ( 'NONE',  ( 116.1998614775786507, 0.4262465694468514643, -12.03445270309931736 ) ) ;
#20822 = CARTESIAN_POINT ( 'NONE',  ( 113.0798948109119948, -8.899110576539710493, -16.42337572283490132 ) ) ;
#20823 = VERTEX_POINT ( 'NONE', #15762 ) ;
#20824 = CARTESIAN_POINT ( 'NONE',  ( 120.7852516859119731, -0.6942167230862511529, -9.935906262978006609 ) ) ;
#20825 = CARTESIAN_POINT ( 'NONE',  ( 125.5597614775786326, -7.894159318335828068, -9.358103419637847864 ) ) ;
#20826 = CARTESIAN_POINT ( 'NONE',  ( 115.4056881442453459, -2.084020599724406786, -8.691656652584148546 ) ) ;
#20827 = EDGE_LOOP ( 'NONE', ( #5088, #22873, #15322, #19592, #24420 ) ) ;
#20828 = CARTESIAN_POINT ( 'NONE',  ( 126.4262034846904470, -9.248423787863409018, -16.00611581287409280 ) ) ;
#20829 = ORIENTED_EDGE ( 'NONE', *, *, #43145, .F. ) ;
#20830 = CARTESIAN_POINT ( 'NONE',  ( 120.1707281442453166, -9.565557343593413364, -10.61323700422348004 ) ) ;
#20831 = CARTESIAN_POINT ( 'NONE',  ( 112.1155414775786454, -10.15424416112533912, -14.75197769757731336 ) ) ;
#20832 = DIRECTION ( 'NONE',  ( 0.000000000000000000, 0.6004852223388321697, -0.7996358532186279566 ) ) ;
#20833 = ADVANCED_FACE ( 'NONE', ( #33746 ), #3132, .F. ) ;
#20834 = EDGE_CURVE ( 'NONE', #24866, #1124, #43351, .T. ) ;
#20835 = CIRCLE ( 'NONE', #14289, 0.8509999999999994236 ) ;
#20836 = CARTESIAN_POINT ( 'NONE',  ( 122.5215798109119874, -7.200787124940443817, -17.81845355600750835 ) ) ;
#20837 = ORIENTED_EDGE ( 'NONE', *, *, #8038, .T. ) ;
#20838 = FACE_OUTER_BOUND ( 'NONE', #3277, .T. ) ;
#20839 = CARTESIAN_POINT ( 'NONE',  ( 124.9063227527192765, 2.723630896063975015, -12.29189508076541415 ) ) ;
#20840 = CARTESIAN_POINT ( 'NONE',  ( 106.8015515045248378, -6.936859964151250502, -18.39754474579286025 ) ) ;
#20841 = VECTOR ( 'NONE', #12377, 1000.000000000000227 ) ;
#20842 = CARTESIAN_POINT ( 'NONE',  ( 70.19189222814998175, -100.0979043305785581, -53.24182196210380624 ) ) ;
#20843 = CARTESIAN_POINT ( 'NONE',  ( 123.8579614775786126, -9.859900752359378018, -12.68260735090039759 ) ) ;
#20844 = CARTESIAN_POINT ( 'NONE',  ( 116.0864081442453113, -0.1624402480850797581, -16.17319339645315424 ) ) ;
#20845 = DIRECTION ( 'NONE',  ( -0.7871354856660162103, -0.4483307682966942709, -0.4235767337848251879 ) ) ;
#20846 = VERTEX_POINT ( 'NONE', #26244 ) ;
#20847 = LINE ( 'NONE', #31318, #19336 ) ;
#20848 = CARTESIAN_POINT ( 'NONE',  ( 115.4056881442453459, -2.084020599724406786, -8.691656652584148546 ) ) ;
#20849 = B_SPLINE_CURVE_WITH_KNOTS ( 'NONE', 3,
 ( #16210, #12490, #9743, #20001, #33885, #2201, #2655, #16587, #30481, #2888 ),
 .UNSPECIFIED., .F., .F.,
 ( 4, 3, 3, 4 ),
 ( 0.000000000000000000, 0.0002476486447138955493, 0.0004952972925464370650, 0.0009604418836934769301 ),
 .UNSPECIFIED. ) ;
#20850 = CARTESIAN_POINT ( 'NONE',  ( 85.49677685831618135, -28.45307765865058514, -9.194547833600635656 ) ) ;
#20851 = CARTESIAN_POINT ( 'NONE',  ( 125.6164881442453094, 0.2603800115204892296, -16.42320221600525088 ) ) ;
#20852 = VECTOR ( 'NONE', #25183, 1000.000000000000000 ) ;
#20853 = CARTESIAN_POINT ( 'NONE',  ( 111.7184548109119788, -9.261995988541697145, -16.69588392320189030 ) ) ;
#20854 = ORIENTED_EDGE ( 'NONE', *, *, #14992, .T. ) ;
#20855 = CARTESIAN_POINT ( 'NONE',  ( 112.5126281442453120, -10.30919188438810075, -12.61870101168855918 ) ) ;
#20856 = CARTESIAN_POINT ( 'NONE',  ( 109.4627908578216733, 0.04929351793716424401, -12.14321520033835533 ) ) ;
#20857 = CARTESIAN_POINT ( 'NONE',  ( 115.0664733795247798, -8.938348069036489818, -17.46756447353520159 ) ) ;
#20858 = CARTESIAN_POINT ( 'NONE',  ( 113.0798948109119948, -0.4660016031367893996, -10.09054647747474043 ) ) ;
#20859 = CARTESIAN_POINT ( 'NONE',  ( 112.8529881442453302, -1.561330072975668060, -17.79121239304076596 ) ) ;
#20860 = CARTESIAN_POINT ( 'NONE',  ( 122.4965214775786251, 0.1319031606808879209, -14.10382304977623669 ) ) ;
#20861 = CARTESIAN_POINT ( 'NONE',  ( 112.3578015045248719, -6.936859964151197211, -18.39754474579287447 ) ) ;
#20862 = CARTESIAN_POINT ( 'NONE',  ( 109.2324108795247923, -1.325403438956436419, -16.93181055722141792 ) ) ;
#20863 = EDGE_CURVE ( 'NONE', #30793, #25225, #22819, .T. ) ;
#20864 = AXIS2_PLACEMENT_3D ( 'NONE', #30315, #37376, #44693 ) ;
#20865 = CARTESIAN_POINT ( 'NONE',  ( 111.5938171295247940, -10.62599879583958540, -13.39321520033832158 ) ) ;
#20866 = CARTESIAN_POINT ( 'NONE',  ( 109.2294413173287921, -4.065513199837466729, -18.48415429053572723 ) ) ;
#20867 = CARTESIAN_POINT ( 'NONE',  ( 116.4267681442453153, -6.222761293078241884, -8.102969835052219238 ) ) ;
#20868 = CARTESIAN_POINT ( 'NONE',  ( 105.8986608795248401, -8.938348069036489818, -9.318865927141430916 ) ) ;
#20869 = DIRECTION ( 'NONE',  ( 1.000000000000000000, 0.000000000000000000, -0.000000000000000000 ) ) ;
#20870 = CARTESIAN_POINT ( 'NONE',  ( 110.6214733795247867, -8.938348069036489818, -17.46756447353520159 ) ) ;
#20871 = CARTESIAN_POINT ( 'NONE',  ( 124.7088614775786226, 0.2603800115204892296, -16.42320221600525088 ) ) ;
#20872 = CARTESIAN_POINT ( 'NONE',  ( 125.3895814775786448, -7.893985811506177619, -18.51759400769804742 ) ) ;
#20873 = CARTESIAN_POINT ( 'NONE',  ( 84.39081516114413262, -30.32262605124143562, -4.893215200338314474 ) ) ;
#20874 = EDGE_CURVE ( 'NONE', #42698, #25860, #16096, .T. ) ;
#20875 = CARTESIAN_POINT ( 'NONE',  ( 119.7736414775786358, -10.30919188438810075, -12.61870101168855918 ) ) ;
#20876 = CARTESIAN_POINT ( 'NONE',  ( 114.6115148109119986, -3.383040157471821630, -19.15922257007629170 ) ) ;
#20877 = ORIENTED_EDGE ( 'NONE', *, *, #17484, .F. ) ;
#20878 = CIRCLE ( 'NONE', #28906, 5.132259260909266985 ) ;
#20879 = EDGE_CURVE ( 'NONE', #1042, #17628, #41955, .T. ) ;
#20880 = CARTESIAN_POINT ( 'NONE',  ( 115.5758681442453053, -7.894159318335828068, -9.358103419637847864 ) ) ;
#20881 = CARTESIAN_POINT ( 'NONE',  ( 122.4965214775786251, -10.30919188438810075, -12.61870101168855918 ) ) ;
#20882 = CARTESIAN_POINT ( 'NONE',  ( 112.9664414775786412, 0.5811942927096154232, -14.16772938898807155 ) ) ;
#20883 = CARTESIAN_POINT ( 'NONE',  ( 114.9518748109119883, -7.643976991954077427, -18.09477374809248928 ) ) ;
#20884 = VERTEX_POINT ( 'NONE', #6623 ) ;
#20885 = CARTESIAN_POINT ( 'NONE',  ( 120.6812681442452941, 0.1319031606808879209, -14.10382304977623669 ) ) ;
#20886 = EDGE_CURVE ( 'NONE', #32403, #11067, #946, .T. ) ;
#20887 = CARTESIAN_POINT ( 'NONE',  ( 118.1285681442453068, -7.893985811506177619, -18.51759400769804742 ) ) ;
#20888 = DIRECTION ( 'NONE',  ( 1.000000000000000000, 0.000000000000000000, 0.000000000000000000 ) ) ;
#20889 = CARTESIAN_POINT ( 'NONE',  ( 115.3442858795247759, -0.7896495226426338832, -17.46756447353520159 ) ) ;
#20890 = VERTEX_POINT ( 'NONE', #27822 ) ;
#20891 = EDGE_CURVE ( 'NONE', #41111, #36064, #43310, .T. ) ;
#20892 = EDGE_CURVE ( 'NONE', #19616, #42627, #6785, .T. ) ;
#20893 = EDGE_CURVE ( 'NONE', #25485, #39549, #13697, .T. ) ;
#20894 = DIRECTION ( 'NONE',  ( -0.000000000000000000, -0.9284778069183721172, -0.3713878862591650232 ) ) ;
#20895 = CARTESIAN_POINT ( 'NONE',  ( 94.20708369096698220, -26.78140590431383572, -13.71816897054060469 ) ) ;
#20896 = TOROIDAL_SURFACE ( 'NONE', #18707, 12.50000000000000000, 1.500000000000000000 ) ;
#20897 = CARTESIAN_POINT ( 'NONE',  ( 61.69189222814998175, -50.16718729050181480, -6.893215200338315363 ) ) ;
#20898 = CARTESIAN_POINT ( 'NONE',  ( 115.2355081442453155, -10.30919188438810075, -12.61870101168855918 ) ) ;
#20899 = CARTESIAN_POINT ( 'NONE',  ( 68.68839935636916039, -25.95913848132418522, -5.893215200338315363 ) ) ;
#20900 = CARTESIAN_POINT ( 'NONE',  ( 112.7962614775786676, -6.222761293078241884, -8.102969835052219238 ) ) ;
#20901 = CARTESIAN_POINT ( 'NONE',  ( 61.17398009194395314, -12.48488768724098108, -17.20141017814964357 ) ) ;
#20902 = CARTESIAN_POINT ( 'NONE',  ( 61.76986277844709861, -39.32091226840162079, -19.39321520033831447 ) ) ;
#20903 = CARTESIAN_POINT ( 'NONE',  ( 115.2748327545248657, -6.936859964151250502, -8.388885654883777576 ) ) ;
#20904 = CIRCLE ( 'NONE', #33247, 4.000000000000000888 ) ;
#20905 = CARTESIAN_POINT ( 'NONE',  ( 118.5256548109119876, -0.4660016031367893996, -10.09054647747474043 ) ) ;
#20906 = FACE_OUTER_BOUND ( 'NONE', #35785, .T. ) ;
#20907 = DIRECTION ( 'NONE',  ( -0.2768435750659239414, -0.3568721902840664151, 0.8921882507333142032 ) ) ;
#20908 = CARTESIAN_POINT ( 'NONE',  ( 124.6051735609119646, -9.645473719204691321, -14.86997237629403301 ) ) ;
#20909 = CARTESIAN_POINT ( 'NONE',  ( 122.8368814775786291, -7.894159318335828068, -9.358103419637847864 ) ) ;
#20910 = ORIENTED_EDGE ( 'NONE', *, *, #21656, .T. ) ;
#20911 = CARTESIAN_POINT ( 'NONE',  ( 61.69189222814998175, -40.21211973637273474, -7.393215200338315363 ) ) ;
#20912 = CARTESIAN_POINT ( 'NONE',  ( 119.3765548109119834, 0.9020085738987339008, -11.91225656197089222 ) ) ;
#20913 = CARTESIAN_POINT ( 'NONE',  ( 94.20708369096698220, -27.10035099198479358, -13.29271931396930739 ) ) ;
#20914 = CARTESIAN_POINT ( 'NONE',  ( 117.5045748109119756, -9.859900752359374465, -12.68260735090039404 ) ) ;
#20915 = CARTESIAN_POINT ( 'NONE',  ( 111.6617281442453304, 0.4262465694468514643, -12.03445270309931736 ) ) ;
#20916 = CYLINDRICAL_SURFACE ( 'NONE', #15471, 5.000000000000004441 ) ;
#20917 = CARTESIAN_POINT ( 'NONE',  ( 114.4413952545248350, 0.8980012041604421569, -11.00651665394454071 ) ) ;
#20918 = CARTESIAN_POINT ( 'NONE',  ( 119.0929214775786278, -4.153390946401325223, -8.397313243818185668 ) ) ;
#20919 = CARTESIAN_POINT ( 'NONE',  ( 118.5823814775786360, -7.643976991954077427, -18.09477374809248928 ) ) ;
#20920 = CARTESIAN_POINT ( 'NONE',  ( 109.2294426061139774, -0.2561256457631079786, -10.72386383753679340 ) ) ;
#20921 = CARTESIAN_POINT ( 'NONE',  ( 87.14323352029596492, -27.84333996136784961, -14.15691383771150136 ) ) ;
#20922 = VECTOR ( 'NONE', #26324, 1000.000000000000000 ) ;
#20923 = CARTESIAN_POINT ( 'NONE',  ( 107.2877233795247776, -1.325403438956436419, -9.854619843455211026 ) ) ;
#20924 = CARTESIAN_POINT ( 'NONE',  ( 83.83554121260367253, -25.99489077589524300, -13.39321520033831625 ) ) ;
#20925 = CARTESIAN_POINT ( 'NONE',  ( 114.7249681442453237, 0.2603800115204892296, -16.42320221600525088 ) ) ;
#20926 = CARTESIAN_POINT ( 'NONE',  ( 115.5758681442453053, -1.561330072975668060, -17.79121239304076951 ) ) ;
#20927 = CARTESIAN_POINT ( 'NONE',  ( 113.1217858795247935, -0.7896495226426338832, -17.46756447353520159 ) ) ;
#20928 = LINE ( 'NONE', #7228, #15535 ) ;
#20929 = EDGE_LOOP ( 'NONE', ( #19746, #4255, #45101, #25507, #26606 ) ) ;
#20930 = CARTESIAN_POINT ( 'NONE',  ( 117.4103264091100840, -0.9924539043446216624, -17.29976612834909133 ) ) ;
#20931 = CARTESIAN_POINT ( 'NONE',  ( 122.1561614775786353, -0.4660016031367893996, -10.09054647747474043 ) ) ;
#20932 = CARTESIAN_POINT ( 'NONE',  ( 114.1577014775786552, -6.344957434206662583, -7.627207830600332805 ) ) ;
#20933 = CARTESIAN_POINT ( 'NONE',  ( 117.2209414775786485, -2.084020599724406786, -8.691656652584148546 ) ) ;
#20934 = CARTESIAN_POINT ( 'NONE',  ( 111.3213681442453264, -7.643976991954077427, -18.09477374809248928 ) ) ;
#20935 = CARTESIAN_POINT ( 'NONE',  ( 119.8303681442453126, -10.63000616557722466, -14.87417383870573495 ) ) ;
#20936 = EDGE_CURVE ( 'NONE', #3470, #14232, #2, .T. ) ;
#20937 = AXIS2_PLACEMENT_3D ( 'NONE', #7651, #14952, #11308 ) ;
#20938 = B_SPLINE_CURVE_WITH_KNOTS ( 'NONE', 3,
 ( #799, #42313, #14942, #7410, #36119, #14717, #28403, #35898, #31808, #11072, #18585, #38871, #21330, #4664 ),
 .UNSPECIFIED., .F., .F.,
 ( 4, 2, 2, 2, 2, 2, 4 ),
 ( 0.006010506521692418960, 0.007331959427853154687, 0.007992685880933507805, 0.008653412334013860924, 0.009314138787094194960, 0.009974865240174530731, 0.01129631814633520054 ),
 .UNSPECIFIED. ) ;
#20939 = CARTESIAN_POINT ( 'NONE',  ( 106.2459265045248173, -2.791137627527939813, -8.388885654883777576 ) ) ;
#20940 = CARTESIAN_POINT ( 'NONE',  ( 126.1270281442452870, -10.30919188438810075, -12.61870101168855918 ) ) ;
#20941 = CARTESIAN_POINT ( 'NONE',  ( 85.31664890835789095, -21.99489077589589314, -15.39321520033831980 ) ) ;
#20942 = ORIENTED_EDGE ( 'NONE', *, *, #17584, .F. ) ;
#20943 = CARTESIAN_POINT ( 'NONE',  ( 117.9583881442453048, -10.30919188438810075, -12.61870101168855918 ) ) ;
#20944 = LINE ( 'NONE', #24587, #28573 ) ;
#20945 = CARTESIAN_POINT ( 'NONE',  ( 115.6893214775786447, 0.5811942927096154232, -14.16772938898807155 ) ) ;
#20946 = ORIENTED_EDGE ( 'NONE', *, *, #11364, .F. ) ;
#20947 = CARTESIAN_POINT ( 'NONE',  ( 116.4555358795247884, -0.7896495226426338832, -17.46756447353520159 ) ) ;
#20948 = CARTESIAN_POINT ( 'NONE',  ( 125.1626748109119802, -9.988377603198980381, -10.36322818467138518 ) ) ;
#20950 = CARTESIAN_POINT ( 'NONE',  ( 27.57768543387103222, -14.97172645945875935, -8.893215200338314474 ) ) ;
#20949 = CIRCLE ( 'NONE', #10764, 2.999999999999999556 ) ;
#20951 = CARTESIAN_POINT ( 'NONE',  ( 90.20794100481921873, -11.57440209418094668, -18.64321520033831803 ) ) ;
#20952 = FACE_OUTER_BOUND ( 'NONE', #32196, .T. ) ;
#20953 = EDGE_CURVE ( 'NONE', #43475, #7179, #24262, .T. ) ;
#20954 = CARTESIAN_POINT ( 'NONE',  ( 120.0572748109119772, -6.222761293078241884, -8.102969835052219238 ) ) ;
#20955 = CYLINDRICAL_SURFACE ( 'NONE', #20718, 1.999999999999998668 ) ;
#20956 = CARTESIAN_POINT ( 'NONE',  ( 116.4267681442453153, -6.222761293078241884, -8.102969835052219238 ) ) ;
#20957 = FACE_OUTER_BOUND ( 'NONE', #12575, .T. ) ;
#20958 = CARTESIAN_POINT ( 'NONE',  ( 118.1285681442453068, -2.084020599724406786, -8.691656652584148546 ) ) ;
#20959 = CARTESIAN_POINT ( 'NONE',  ( 121.8965016859119856, -9.665098340737509730, -17.37397104707595474 ) ) ;
#20960 = CARTESIAN_POINT ( 'NONE',  ( 117.1642148109119859, -9.261995988541697145, -16.69588392320189030 ) ) ;
#20961 = DIRECTION ( 'NONE',  ( -0.9498278979187093629, -0.3127730236694430954, 0.000000000000000000 ) ) ;
#20962 = CARTESIAN_POINT ( 'NONE',  ( 117.3911214775786505, -7.894159318335828068, -9.358103419637847864 ) ) ;
#20963 = ORIENTED_EDGE ( 'NONE', *, *, #24911, .F. ) ;
#20964 = CARTESIAN_POINT ( 'NONE',  ( 116.5402214775786405, 0.2603800115204892296, -16.42320221600525088 ) ) ;
#20965 = CARTESIAN_POINT ( 'NONE',  ( 108.7462390045248242, 0.8980012041604421569, -15.77991374673208469 ) ) ;
#20966 = CARTESIAN_POINT ( 'NONE',  ( 115.9613248136183614, -3.929494816604736318, -18.62311481910882094 ) ) ;
#20967 = CARTESIAN_POINT ( 'NONE',  ( 114.7886608795247696, -1.325403438956436419, -16.93181055722138595 ) ) ;
#20968 = CARTESIAN_POINT ( 'NONE',  ( 121.5038390224331835, -4.681800857092175860, -18.57451437749315559 ) ) ;
#20969 = CARTESIAN_POINT ( 'NONE',  ( 124.0281414775786146, -1.834011780172310813, -8.268836392978581529 ) ) ;
#20970 = ORIENTED_EDGE ( 'NONE', *, *, #28100, .F. ) ;
#20971 = CARTESIAN_POINT ( 'NONE',  ( 126.6827570900284599, -8.613729037902059460, -9.744110473525523730 ) ) ;
#20972 = CARTESIAN_POINT ( 'NONE',  ( 117.3911214775786505, -7.894159318335828068, -9.358103419637847864 ) ) ;
#20973 = CARTESIAN_POINT ( 'NONE',  ( 116.2565881442452991, -9.261995988541702474, -16.69588392320188319 ) ) ;
#20974 = CARTESIAN_POINT ( 'NONE',  ( 109.3272331777918822, -0.01829820670803256055, -14.64321520033831447 ) ) ;
#20975 = CARTESIAN_POINT ( 'NONE',  ( 124.0281414775786146, -1.834011780172310813, -8.268836392978581529 ) ) ;
#20976 = CARTESIAN_POINT ( 'NONE',  ( 113.0523327545247838, -6.936859964151250502, -8.388885654883777576 ) ) ;
#20977 = CARTESIAN_POINT ( 'NONE',  ( 124.5539070589982060, -1.063912429576147511, -17.20460841810472985 ) ) ;
#20978 = EDGE_LOOP ( 'NONE', ( #43115, #43829, #1014, #16239 ) ) ;
#20979 = CARTESIAN_POINT ( 'NONE',  ( 115.5758681442453053, -1.561330072975668060, -17.79121239304076951 ) ) ;
#20980 = CARTESIAN_POINT ( 'NONE',  ( 125.5597614775786326, -7.894159318335828068, -9.358103419637847864 ) ) ;
#20981 = CARTESIAN_POINT ( 'NONE',  ( 122.6099748109119929, -9.261995988541697145, -16.69588392320189030 ) ) ;
#20982 = CARTESIAN_POINT ( 'NONE',  ( 118.7525614775786380, -1.833838273342659253, -17.42832698103878286 ) ) ;
#20983 = CARTESIAN_POINT ( 'NONE',  ( 70.19189222814998175, -57.25954915413987578, -36.10662921840084749 ) ) ;
#20984 = CARTESIAN_POINT ( 'NONE',  ( 117.3911214775786505, -1.561330072975668504, -17.79121239304076951 ) ) ;
#20985 = DIRECTION ( 'NONE',  ( -0.000000000000000000, -0.9284778069183720062, -0.3713878862591650232 ) ) ;
#20986 = CARTESIAN_POINT ( 'NONE',  ( 123.6877814775786533, -6.222761293078241884, -8.102969835052219238 ) ) ;
#20987 = ORIENTED_EDGE ( 'NONE', *, *, #16294, .F. ) ;
#20988 = CARTESIAN_POINT ( 'NONE',  ( 110.2184548109119788, -3.410847707154508246, -16.57729307524250473 ) ) ;
#20989 = CARTESIAN_POINT ( 'NONE',  ( 117.2776681442452968, -5.638512984488999180, -18.83840828888717311 ) ) ;
#20990 = CARTESIAN_POINT ( 'NONE',  ( 124.2550481442452792, -0.1624402480850797581, -16.17319339645315424 ) ) ;
#20991 = ORIENTED_EDGE ( 'NONE', *, *, #10543, .T. ) ;
#20992 = CARTESIAN_POINT ( 'NONE',  ( 136.0617147589318279, -1.217740506595299310, -8.750557032691128612 ) ) ;
#20993 = CARTESIAN_POINT ( 'NONE',  ( 122.7234281442452755, -5.638512984488999180, -18.83840828888717311 ) ) ;
#20994 = CARTESIAN_POINT ( 'NONE',  ( 106.1764733795248219, -8.938348069036489818, -17.46756447353520159 ) ) ;
#20995 = CARTESIAN_POINT ( 'NONE',  ( 119.1496481442453046, -6.222761293078241884, -8.102969835052219238 ) ) ;
#20996 = ORIENTED_EDGE ( 'NONE', *, *, #7822, .F. ) ;
#20997 = ORIENTED_EDGE ( 'NONE', *, *, #935, .F. ) ;
#20998 = CARTESIAN_POINT ( 'NONE',  ( 115.9162281442453235, -4.089484607189486809, -7.948022111789456723 ) ) ;
#20999 = EDGE_CURVE ( 'NONE', #32579, #40888, #6816, .T. ) ;
#21000 = CARTESIAN_POINT ( 'NONE',  ( 125.7866681442452688, -8.899110576539710493, -16.42337572283490132 ) ) ;
#21001 = CARTESIAN_POINT ( 'NONE',  ( 120.3409081442453044, -0.4660016031367703038, -10.09054647747476707 ) ) ;
#21002 = CARTESIAN_POINT ( 'NONE',  ( 77.25325688895158294, -4.012910213732562070, -7.993215200338315007 ) ) ;
#21003 = CARTESIAN_POINT ( 'NONE',  ( 121.5888948109119809, -10.30919188438810075, -12.61870101168855918 ) ) ;
#21004 = DIRECTION ( 'NONE',  ( 0.1352586133457950590, 0.9908103287288504424, 0.000000000000000000 ) ) ;
#21005 = AXIS2_PLACEMENT_3D ( 'NONE', #19350, #19123, #8858 ) ;
#21006 = DIRECTION ( 'NONE',  ( 0.9063289528979890930, 0.4225728684367167087, 0.000000000000000000 ) ) ;
#21007 = CARTESIAN_POINT ( 'NONE',  ( 122.8936081442453059, 0.2603800115204892296, -16.42320221600525088 ) ) ;
#21009 = CARTESIAN_POINT ( 'NONE',  ( 124.9357681442453014, -7.643976991954077427, -18.09477374809248928 ) ) ;
#21008 = CARTESIAN_POINT ( 'NONE',  ( 118.0718414775786300, -9.261995988541697145, -16.69588392320189030 ) ) ;
#21010 = CARTESIAN_POINT ( 'NONE',  ( 118.5823814775786360, -7.643976991954077427, -18.09477374809248928 ) ) ;
#21011 = CARTESIAN_POINT ( 'NONE',  ( 64.57998409241588433, -15.42822026892965326, -16.02015606411926996 ) ) ;
#21012 = CARTESIAN_POINT ( 'NONE',  ( 116.3133148109119759, -7.893985811506177619, -18.51759400769804742 ) ) ;
#21013 = ORIENTED_EDGE ( 'NONE', *, *, #21238, .T. ) ;
#21014 = CARTESIAN_POINT ( 'NONE',  ( 124.9819548109120291, -7.618532446444632455, -18.05174138884769874 ) ) ;
#21015 = CARTESIAN_POINT ( 'NONE',  ( 113.3301452545248083, -9.868328341294098749, -15.46607636864997204 ) ) ;
#21016 = CARTESIAN_POINT ( 'NONE',  ( 107.7738952545248310, -9.868328341294098749, -15.46607636864997204 ) ) ;
#21017 = CARTESIAN_POINT ( 'NONE',  ( 107.7738952545248310, 0.8980012041604421569, -11.00651665394454071 ) ) ;
#21018 = EDGE_CURVE ( 'NONE', #5955, #9699, #19070, .T. ) ;
#21019 = CARTESIAN_POINT ( 'NONE',  ( 125.0954081442453401, -3.517672760958747702, -18.63504008191803152 ) ) ;
#21020 = CARTESIAN_POINT ( 'NONE',  ( 124.8790414775786246, -8.899110576539710493, -16.42337572283490132 ) ) ;
#21021 = ORIENTED_EDGE ( 'NONE', *, *, #179, .F. ) ;
#21022 = CARTESIAN_POINT ( 'NONE',  ( 113.9307948109119764, -10.15424416112533912, -14.75197769757731336 ) ) ;
#21023 = CARTESIAN_POINT ( 'NONE',  ( 113.4690515045247992, -2.477300249445798297, -7.631215200338321125 ) ) ;
#21024 = CARTESIAN_POINT ( 'NONE',  ( 122.1561614775786353, -8.899110576539724704, -16.42337572283488356 ) ) ;
#21025 = CARTESIAN_POINT ( 'NONE',  ( 123.4608748109119745, -10.63000616557722466, -14.87417383870573495 ) ) ;
#21026 = CARTESIAN_POINT ( 'NONE',  ( 123.8579614775786126, 0.5811942927096110934, -14.16772938898807510 ) ) ;
#21027 = CARTESIAN_POINT ( 'NONE',  ( 120.2296266859119953, -9.033780868592240054, -16.85052413769862056 ) ) ;
#21028 = CARTESIAN_POINT ( 'NONE',  ( 113.7038881442453402, -3.383040157471821630, -19.15922257007629170 ) ) ;
#21029 = CARTESIAN_POINT ( 'NONE',  ( 114.2330358795247776, -0.7896495226426338832, -17.46756447353520159 ) ) ;
#21030 = CARTESIAN_POINT ( 'NONE',  ( 106.5237390045248418, 0.8980012041604421569, -15.77991374673208469 ) ) ;
#21031 = VERTEX_POINT ( 'NONE', #15656 ) ;
#21032 = CARTESIAN_POINT ( 'NONE',  ( 124.7503625628256714, -2.263366209404227281, -18.10533625161308180 ) ) ;
#21033 = CARTESIAN_POINT ( 'NONE',  ( 115.0653281442453277, -3.505236298600246325, -18.68346056562440793 ) ) ;
#21034 = CARTESIAN_POINT ( 'NONE',  ( 113.0231681442453322, 0.9020085738987339008, -11.91225656197089222 ) ) ;
#21035 = B_SPLINE_CURVE_WITH_KNOTS ( 'NONE', 3,
 ( #11465, #4825, #32637, #22386, #1403, #36281, #38808, #5049, #15544, #39038 ),
 .UNSPECIFIED., .F., .F.,
 ( 4, 3, 3, 4 ),
 ( 0.000000000000000000, 0.0002476487219222790075, 0.0004952974148303609372, 0.0009534114850261630417 ),
 .UNSPECIFIED. ) ;
#21036 = CARTESIAN_POINT ( 'NONE',  ( 114.3719421295247827, 0.8980012041604618078, -13.39321520033831447 ) ) ;
#21037 = CARTESIAN_POINT ( 'NONE',  ( 106.1070202545248407, 0.1403307496149616695, -11.32035403202665336 ) ) ;
#21038 = CARTESIAN_POINT ( 'NONE',  ( 122.1561614775786353, -8.899110576539710493, -16.42337572283490132 ) ) ;
#21039 = CARTESIAN_POINT ( 'NONE',  ( 118.4689281442453250, -10.15424416112533912, -14.75197769757731336 ) ) ;
#21040 = CARTESIAN_POINT ( 'NONE',  ( 111.7751814775786556, -2.084020599724406786, -8.691656652584148546 ) ) ;
#21041 = ORIENTED_EDGE ( 'NONE', *, *, #42209, .F. ) ;
#21042 = CARTESIAN_POINT ( 'NONE',  ( 125.5030348109119558, -6.222761293078241884, -8.102969835052219238 ) ) ;
#21043 = CARTESIAN_POINT ( 'NONE',  ( 96.21525317080913453, -26.27671625074736994, -11.36238786408634738 ) ) ;
#21044 = CARTESIAN_POINT ( 'NONE',  ( 114.8951481442453115, -8.899110576539710493, -16.42337572283490132 ) ) ;
#21045 = VERTEX_POINT ( 'NONE', #5384 ) ;
#21046 = DIRECTION ( 'NONE',  ( -0.9609149988134837450, 0.1028163501681639419, -0.2570431154366518145 ) ) ;
#21047 = CARTESIAN_POINT ( 'NONE',  ( 111.2465515045248168, -6.936859964151250502, -18.39754474579286025 ) ) ;
#21048 = EDGE_LOOP ( 'NONE', ( #2769, #32833, #41596, #41485 ) ) ;
#21049 = CARTESIAN_POINT ( 'NONE',  ( 120.3409081442453044, -8.899110576539710493, -16.42337572283490132 ) ) ;
#21050 = CARTESIAN_POINT ( 'NONE',  ( 112.3991748109119868, -1.833838273342658809, -17.42832698103878286 ) ) ;
#21051 = CARTESIAN_POINT ( 'NONE',  ( 114.7816948109119863, 0.5811942927096102052, -14.16772938898808221 ) ) ;
#21052 = CARTESIAN_POINT ( 'NONE',  ( 122.7299391859119737, -8.844754642576884152, -8.592115655440050404 ) ) ;
#21053 = EDGE_LOOP ( 'NONE', ( #25788, #33986, #2476, #24003 ) ) ;
#21054 = CARTESIAN_POINT ( 'NONE',  ( 75.95778847736514194, -3.256761025687008537, -7.147228641687434880 ) ) ;
#21055 = CARTESIAN_POINT ( 'NONE',  ( 63.69189222814998175, -74.27079820037398861, -36.22049641875047143 ) ) ;
#21056 = CARTESIAN_POINT ( 'NONE',  ( 116.3860827545247787, -2.477300249445798297, -19.15521520033831138 ) ) ;
#21057 = CARTESIAN_POINT ( 'NONE',  ( 111.8886348109120092, -3.383040157471821630, -19.15922257007629170 ) ) ;
#21058 = CARTESIAN_POINT ( 'NONE',  ( 122.1561614775786353, -8.899110576539710493, -16.42337572283490132 ) ) ;
#21059 = CARTESIAN_POINT ( 'NONE',  ( 119.3765548109119834, -10.15424416112533912, -14.75197769757731336 ) ) ;
#21060 = CARTESIAN_POINT ( 'NONE',  ( 138.2184548109119930, -3.878253464830349273, -6.462969451276144639 ) ) ;
#21061 = ORIENTED_EDGE ( 'NONE', *, *, #14202, .F. ) ;
#21062 = CARTESIAN_POINT ( 'NONE',  ( 115.0086014775786509, -5.574606645277164318, -18.38911715685844683 ) ) ;
#21063 = CARTESIAN_POINT ( 'NONE',  ( 119.7434548109119703, -5.696008164919469152, -19.01495265173020499 ) ) ;
#21064 = CARTESIAN_POINT ( 'NONE',  ( 125.1269327111056953, -1.267766418764818770, -16.93314635290698078 ) ) ;
#21065 = CYLINDRICAL_SURFACE ( 'NONE', #31966, 4.000000000000000888 ) ;
#21066 = AXIS2_PLACEMENT_3D ( 'NONE', #15885, #29781, #32737 ) ;
#21067 = CARTESIAN_POINT ( 'NONE',  ( 114.9518748109119883, -1.834011780172310813, -8.268836392978581529 ) ) ;
#21068 = ORIENTED_EDGE ( 'NONE', *, *, #18422, .F. ) ;
#21069 = CARTESIAN_POINT ( 'NONE',  ( 113.1933481442453058, -4.089484607189486809, -7.948022111789456723 ) ) ;
#21070 = CIRCLE ( 'NONE', #13794, 3.999999999999997780 ) ;
#21071 = DIRECTION ( 'NONE',  ( -1.000000000000000000, 0.000000000000000000, 0.000000000000000000 ) ) ;
#21072 = CARTESIAN_POINT ( 'NONE',  ( 110.3436608795247764, -8.938348069036489818, -9.318865927141430916 ) ) ;
#21073 = CARTESIAN_POINT ( 'NONE',  ( 114.2144281442453178, -8.166667518702817929, -8.995218007635859436 ) ) ;
#21074 = CARTESIAN_POINT ( 'NONE',  ( 114.3278814775786429, -10.30919188438810075, -12.61870101168855918 ) ) ;
#21075 = CARTESIAN_POINT ( 'NONE',  ( 121.9292548109119849, -7.894159318335828068, -9.358103419637847864 ) ) ;
#21076 = CARTESIAN_POINT ( 'NONE',  ( 60.49017502987772588, -14.58217554126443893, -18.15922316508111933 ) ) ;
#21077 = CARTESIAN_POINT ( 'NONE',  ( 112.2883483795247770, -8.402594152722688392, -16.93181055722141792 ) ) ;
#21078 = CARTESIAN_POINT ( 'NONE',  ( 112.0435892294923974, -2.263366209404214402, -18.10533625161307114 ) ) ;
#21079 = CARTESIAN_POINT ( 'NONE',  ( 109.2294421291290405, -4.119415819779401744, -18.49485328025912878 ) ) ;
#21080 = CARTESIAN_POINT ( 'NONE',  ( 116.2565881442453133, -0.8288870151387760510, -10.36305467784173118 ) ) ;
#21081 = CARTESIAN_POINT ( 'NONE',  ( 106.3848327545248651, -2.477300249445798297, -19.15521520033831138 ) ) ;
#21082 = CARTESIAN_POINT ( 'NONE',  ( 116.9417077545247992, -2.791137627527939813, -18.39754474579286025 ) ) ;
#21083 = CARTESIAN_POINT ( 'NONE',  ( 111.1076452545248259, 0.8980012041604421569, -11.00651665394454071 ) ) ;
#21084 = CARTESIAN_POINT ( 'NONE',  ( 121.7136302882355068, -1.135392229370310258, -17.10942237759953244 ) ) ;
#21085 = CARTESIAN_POINT ( 'NONE',  ( 124.1415948109119540, -6.344957434206665248, -7.627207830600338134 ) ) ;
#21086 = CARTESIAN_POINT ( 'NONE',  ( 125.2194014775786286, -10.30919188438810075, -12.61870101168855918 ) ) ;
#21087 = EDGE_CURVE ( 'NONE', #31092, #43396, #29334, .T. ) ;
#21088 = CARTESIAN_POINT ( 'NONE',  ( 117.3343948109119737, -3.383040157471821630, -19.15922257007629170 ) ) ;
#21089 = VERTEX_POINT ( 'NONE', #8590 ) ;
#21090 = CARTESIAN_POINT ( 'NONE',  ( 114.3278814775786429, 0.1319031606808879209, -14.10382304977623669 ) ) ;
#21091 = CARTESIAN_POINT ( 'NONE',  ( 112.9664414775786412, 0.5811942927096154232, -14.16772938898807155 ) ) ;
#21092 = CARTESIAN_POINT ( 'NONE',  ( 118.1852948109119836, -5.638512984488999180, -18.83840828888717311 ) ) ;
#21093 = CARTESIAN_POINT ( 'NONE',  ( 117.5613014775786525, -10.15424416112533912, -14.75197769757731336 ) ) ;
#21094 = ORIENTED_EDGE ( 'NONE', *, *, #34810, .T. ) ;
#21095 = CARTESIAN_POINT ( 'NONE',  ( 121.7023481442452777, -0.8288870151387760510, -10.36305467784173118 ) ) ;
#21096 = CARTESIAN_POINT ( 'NONE',  ( 116.6536748109119941, 0.9020085738987339008, -11.91225656197089222 ) ) ;
#21097 = VECTOR ( 'NONE', #35113, 1000.000000000000114 ) ;
#21098 = CARTESIAN_POINT ( 'NONE',  ( 42.36021970110777346, -12.73296999994090761, -19.39321520033831447 ) ) ;
#21099 = CARTESIAN_POINT ( 'NONE',  ( 112.8439733795247832, -8.938348069036489818, -17.46756447353520159 ) ) ;
#21100 = CARTESIAN_POINT ( 'NONE',  ( 59.90552009294155766, -2.897503654462286971, -7.393215200338319804 ) ) ;
#21101 = CYLINDRICAL_SURFACE ( 'NONE', #8433, 4.999999999999997335 ) ;
#21102 = EDGE_CURVE ( 'NONE', #24192, #35546, #32954, .T. ) ;
#21103 = DIRECTION ( 'NONE',  ( 0.000000000000000000, -0.9284778069183718952, -0.3713878862591650232 ) ) ;
#21104 = AXIS2_PLACEMENT_3D ( 'NONE', #7620, #28833, #7392 ) ;
#21105 = CARTESIAN_POINT ( 'NONE',  ( 115.0653281442453277, -6.344957434206662583, -7.627207830600332805 ) ) ;
#21106 = CONICAL_SURFACE ( 'NONE', #20389, 2.445500000000004448, 0.9599310885968757034 ) ;
#21107 = DIRECTION ( 'NONE',  ( -1.000000000000000000, 0.000000000000000000, -0.000000000000000000 ) ) ;
#21108 = CARTESIAN_POINT ( 'NONE',  ( 113.7606148109119886, -7.894159318335828068, -9.358103419637847864 ) ) ;
#21109 = EDGE_CURVE ( 'NONE', #13898, #21831, #36162, .T. ) ;
#21110 = CARTESIAN_POINT ( 'NONE',  ( 59.90552009294157898, -2.897503654462289191, -8.893215200338314474 ) ) ;
#21111 = B_SPLINE_CURVE_WITH_KNOTS ( 'NONE', 3,
 ( #21721, #7812, #14881, #29679, #26038, #1191 ),
 .UNSPECIFIED., .F., .F.,
 ( 4, 2, 4 ),
 ( 0.001955951169366054645, 0.002520422424572374680, 0.003084893679778694716 ),
 .UNSPECIFIED. ) ;
#21112 = CARTESIAN_POINT ( 'NONE',  ( 115.2878193026122915, -1.179503403430490538, -17.05068175419388865 ) ) ;
#21113 = CARTESIAN_POINT ( 'NONE',  ( 115.2053796295247849, -4.863998795839590272, -8.388885654883775800 ) ) ;
#21114 = CARTESIAN_POINT ( 'NONE',  ( 117.5613014775786525, 0.9020085738987339008, -11.91225656197089222 ) ) ;
#21115 = CARTESIAN_POINT ( 'NONE',  ( 76.36356431740252049, -0.2843300395004543235, -12.39321520033831447 ) ) ;
#21116 = EDGE_CURVE ( 'NONE', #38150, #12241, #11181, .T. ) ;
#21117 = PLANE ( 'NONE',  #41348 ) ;
#21119 = CARTESIAN_POINT ( 'NONE',  ( 114.7816948109119863, 0.5811942927096154232, -14.16772938898807155 ) ) ;
#21118 = CARTESIAN_POINT ( 'NONE',  ( 89.12784890491134604, -26.75858941326842810, -11.54476601486570964 ) ) ;
#21120 = CARTESIAN_POINT ( 'NONE',  ( 123.2906948109119867, -1.833838273342659697, -17.42832698103878286 ) ) ;
#21121 = CARTESIAN_POINT ( 'NONE',  ( 119.7169148109119874, -0.1624402480850797581, -16.17319339645315424 ) ) ;
#21122 = VERTEX_POINT ( 'NONE', #28269 ) ;
#21123 = CARTESIAN_POINT ( 'NONE',  ( 135.5837700375767554, -9.599696963706330521, -9.723723590361398550 ) ) ;
#21124 = CARTESIAN_POINT ( 'NONE',  ( 123.2906948109119867, -8.166667518702819706, -8.995218007635861213 ) ) ;
#21125 = CARTESIAN_POINT ( 'NONE',  ( 114.5108483795247878, -8.402594152722688392, -16.93181055722141792 ) ) ;
#21126 = CARTESIAN_POINT ( 'NONE',  ( 114.3846081442453197, 0.4262465694468514643, -12.03445270309931736 ) ) ;
#21127 = CARTESIAN_POINT ( 'NONE',  ( 114.4980614775786734, -2.084020599724406786, -8.691656652584148546 ) ) ;
#21128 = CARTESIAN_POINT ( 'NONE',  ( 85.03101011666282716, -29.58136537014402023, -10.62075117454815043 ) ) ;
#21129 = CARTESIAN_POINT ( 'NONE',  ( 110.8298327545248299, -2.477300249445798297, -19.15521520033831138 ) ) ;
#21130 = CARTESIAN_POINT ( 'NONE',  ( 118.8092881442453290, -0.1624402480850797581, -16.17319339645315424 ) ) ;
#21131 = CARTESIAN_POINT ( 'NONE',  ( 121.3619881442452879, -5.574606645277164318, -18.38911715685844683 ) ) ;
#21132 = CARTESIAN_POINT ( 'NONE',  ( 74.69189222814998175, -41.76310523276723785, -4.893215200338314474 ) ) ;
#21133 = AXIS2_PLACEMENT_3D ( 'NONE', #18714, #8452, #1150 ) ;
#21134 = CARTESIAN_POINT ( 'NONE',  ( 109.2294423051889112, -0.2441102078206954518, -10.74723311813985305 ) ) ;
#21135 = DIRECTION ( 'NONE',  ( 0.000000000000000000, -0.3818493186865936084, 0.9242245927363024194 ) ) ;
#21136 = CARTESIAN_POINT ( 'NONE',  ( 109.0240515045248202, -6.936859964151250502, -18.39754474579286025 ) ) ;
#21137 = EDGE_CURVE ( 'NONE', #44361, #4412, #43474, .T. ) ;
#21138 = CARTESIAN_POINT ( 'NONE',  ( 116.7096590385446433, 2.077600134054068626, -20.77163152589008632 ) ) ;
#21139 = CARTESIAN_POINT ( 'NONE',  ( 117.1642148109119859, -9.261995988541697145, -16.69588392320189030 ) ) ;
#21140 = CARTESIAN_POINT ( 'NONE',  ( 115.0086014775786509, -4.089484607189486809, -7.948022111789456723 ) ) ;
#21141 = CARTESIAN_POINT ( 'NONE',  ( 110.4825671295247815, -10.62599879583958540, -13.39321520033831447 ) ) ;
#21142 = CARTESIAN_POINT ( 'NONE',  ( 123.6328298109119714, -7.200787124940443817, -17.81845355600750835 ) ) ;
#21143 = ADVANCED_FACE ( 'NONE', ( #22488, #25695 ), #3854, .T. ) ;
#21144 = EDGE_CURVE ( 'NONE', #28337, #2441, #34456, .T. ) ;
#21145 = ORIENTED_EDGE ( 'NONE', *, *, #24741, .F. ) ;
#21146 = DIRECTION ( 'NONE',  ( 1.000000000000000000, 0.000000000000000000, -0.000000000000000000 ) ) ;
#21147 = CARTESIAN_POINT ( 'NONE',  ( 120.6245414775786458, -9.988377603198976828, -10.36322818467138340 ) ) ;
#21148 = AXIS2_PLACEMENT_3D ( 'NONE', #3247, #17173, #31062 ) ;
#21149 = CARTESIAN_POINT ( 'NONE',  ( 112.0588148109119828, 0.5811942927096154232, -14.16772938898807155 ) ) ;
#21150 = CARTESIAN_POINT ( 'NONE',  ( 123.8012348109119642, -9.565557343593413364, -10.61323700422348004 ) ) ;
#21151 = CIRCLE ( 'NONE', #1472, 8.000000000000001776 ) ;
#21152 = CARTESIAN_POINT ( 'NONE',  ( 111.2646414775786496, -8.899110576539710493, -16.42337572283490132 ) ) ;
#21153 = CARTESIAN_POINT ( 'NONE',  ( 120.2841814775786276, 0.9020085738987339008, -11.91225656197089222 ) ) ;
#21154 = CARTESIAN_POINT ( 'NONE',  ( 108.6767858795247861, -8.402594152722688392, -9.854619843455216355 ) ) ;
#21155 = CARTESIAN_POINT ( 'NONE',  ( 115.9162281442453093, -5.574606645277164318, -18.38911715685844683 ) ) ;
#21156 = CARTESIAN_POINT ( 'NONE',  ( 111.4241771286805260, -2.495269033102075262, -17.79652296963211455 ) ) ;
#21157 = VERTEX_POINT ( 'NONE', #40041 ) ;
#21158 = CARTESIAN_POINT ( 'NONE',  ( 120.6812681442452941, -10.30919188438810075, -12.61870101168855918 ) ) ;
#21159 = DIRECTION ( 'NONE',  ( 0.000000000000000000, -0.3818493186865936084, 0.9242245927363024194 ) ) ;
#21160 = CARTESIAN_POINT ( 'NONE',  ( 114.6115148109119986, -3.383040157471821630, -19.15922257007629170 ) ) ;
#21161 = ORIENTED_EDGE ( 'NONE', *, *, #6632, .T. ) ;
#21162 = CARTESIAN_POINT ( 'NONE',  ( 116.1082702545247827, -10.62599879583958717, -15.77991374673208469 ) ) ;
#21163 = CARTESIAN_POINT ( 'NONE',  ( 124.5954081442453116, -3.383040157471821630, -19.15922257007629170 ) ) ;
#21164 = VECTOR ( 'NONE', #37098, 1000.000000000000000 ) ;
#21166 = CARTESIAN_POINT ( 'NONE',  ( 122.7234281442452755, -5.638512984489030266, -18.83840828888716601 ) ) ;
#21165 = B_SPLINE_CURVE_WITH_KNOTS ( 'NONE', 3,
 ( #34194, #44712, #34413, #2968 ),
 .UNSPECIFIED., .F., .F.,
 ( 4, 4 ),
 ( 0.000000000000000000, 1.000000000000000000 ),
 .UNSPECIFIED. ) ;
#21167 = CARTESIAN_POINT ( 'NONE',  ( 116.2565881442453133, -0.8288870151387760510, -10.36305467784173118 ) ) ;
#21168 = CARTESIAN_POINT ( 'NONE',  ( 77.41180319171111535, -56.67956859520202073, -1.766371313089957651 ) ) ;
#21169 = CARTESIAN_POINT ( 'NONE',  ( 120.2274548109119934, -9.859900752359378018, -12.68260735090039759 ) ) ;
#21170 = CARTESIAN_POINT ( 'NONE',  ( 120.1339464975817748, -2.215723800389698184, -18.16877924232191788 ) ) ;
#21171 = CARTESIAN_POINT ( 'NONE',  ( 121.7023481442452777, -0.8288870151387760510, -10.36305467784173118 ) ) ;
#21172 = EDGE_CURVE ( 'NONE', #38570, #31472, #1956, .T. ) ;
#21173 = AXIS2_PLACEMENT_3D ( 'NONE', #19973, #6518, #3090 ) ;
#21174 = DIRECTION ( 'NONE',  ( 1.000000000000000000, 0.000000000000000000, 0.000000000000000000 ) ) ;
#21175 = CARTESIAN_POINT ( 'NONE',  ( 118.2987481442453088, -7.894159318335828068, -9.358103419637847864 ) ) ;
#21176 = CIRCLE ( 'NONE', #36463, 2.000000000000000444 ) ;
#21177 = CARTESIAN_POINT ( 'NONE',  ( 123.4939235609119663, 0.6414057260225851653, -11.69287257290600657 ) ) ;
#21178 = CARTESIAN_POINT ( 'NONE',  ( 114.8951481442453115, -0.4660016031367893996, -10.09054647747474043 ) ) ;
#21179 = CARTESIAN_POINT ( 'NONE',  ( 95.28169473643895060, -25.99489077589524300, -13.39321520033831447 ) ) ;
#21180 = CARTESIAN_POINT ( 'NONE',  ( 121.9292548109119849, -7.894159318335828068, -9.358103419637847864 ) ) ;
#21181 = ORIENTED_EDGE ( 'NONE', *, *, #27844, .F. ) ;
#21182 = CARTESIAN_POINT ( 'NONE',  ( 116.4834948109119779, -1.561330072975668504, -17.79121239304076951 ) ) ;
#21183 = CARTESIAN_POINT ( 'NONE',  ( 108.1211608795247798, -8.938348069036489818, -9.318865927141430916 ) ) ;
#21184 = DIRECTION ( 'NONE',  ( -0.05270788615228318846, 0.9986099732815399976, 2.696077241641140828E-16 ) ) ;
#21185 = DIRECTION ( 'NONE',  ( -0.9609149988134837450, 0.1028163501681639419, -0.2570431154366518145 ) ) ;
#21186 = CYLINDRICAL_SURFACE ( 'NONE', #34934, 5.000000000000004441 ) ;
#21187 = CARTESIAN_POINT ( 'NONE',  ( 120.9649014775786355, -3.383040157471821630, -19.15922257007629170 ) ) ;
#21188 = ORIENTED_EDGE ( 'NONE', *, *, #15264, .F. ) ;
#21189 = CARTESIAN_POINT ( 'NONE',  ( 90.72400676789006013, -25.99489077589524300, -13.39321520033831625 ) ) ;
#21190 = CARTESIAN_POINT ( 'NONE',  ( 117.7314814775786260, -5.574606645277164318, -18.38911715685844683 ) ) ;
#21191 = CARTESIAN_POINT ( 'NONE',  ( 125.3666772207509865, -8.500505272813764890, -17.56000656032637153 ) ) ;
#21192 = CARTESIAN_POINT ( 'NONE',  ( 64.78873258728907558, -15.59143358259173873, -15.46696664105744290 ) ) ;
#21193 = ADVANCED_FACE ( 'NONE', ( #29779 ), #12466, .T. ) ;
#21194 = CARTESIAN_POINT ( 'NONE',  ( 111.4665458264767750, -1.295815253274133161, -16.89579513612386563 ) ) ;
#21195 = CARTESIAN_POINT ( 'NONE',  ( 110.4825671295247815, 0.1403307496149613920, -13.39321520033831447 ) ) ;
#21196 = CARTESIAN_POINT ( 'NONE',  ( 121.9470836909669913, -25.99489077589524300, -13.39321520033831447 ) ) ;
#21197 = ORIENTED_EDGE ( 'NONE', *, *, #9730, .T. ) ;
#21198 = CARTESIAN_POINT ( 'NONE',  ( 113.8173414775786512, 0.2603800115204892296, -16.42320221600525088 ) ) ;
#21199 = CARTESIAN_POINT ( 'NONE',  ( 112.9664414775786412, 0.5811942927096154232, -14.16772938898807155 ) ) ;
#21200 = CARTESIAN_POINT ( 'NONE',  ( 121.8158014775786171, -5.638512984488999180, -18.83840828888717311 ) ) ;
#21201 = CARTESIAN_POINT ( 'NONE',  ( 115.4624148109119943, -4.153390946401321671, -8.397313243818183892 ) ) ;
#21202 = DIRECTION ( 'NONE',  ( -0.9609149988134837450, 0.1028163501681639419, -0.2570431154366518145 ) ) ;
#21203 = CARTESIAN_POINT ( 'NONE',  ( 120.3409081442453044, -0.4660016031367893996, -10.09054647747474043 ) ) ;
#21204 = CARTESIAN_POINT ( 'NONE',  ( 111.6050014775786536, 0.1319031606808879209, -14.10382304977623669 ) ) ;
#21205 = ADVANCED_FACE ( 'NONE', ( #17777 ), #38732, .F. ) ;
#21206 = CYLINDRICAL_SURFACE ( 'NONE', #6293, 5.132259260909280307 ) ;
#21207 = CARTESIAN_POINT ( 'NONE',  ( 94.99177781699742695, -29.69178914684045623, -14.92061247508468647 ) ) ;
#21208 = CARTESIAN_POINT ( 'NONE',  ( 122.1561614775786353, -8.899110576539710493, -16.42337572283490132 ) ) ;
#21209 = ORIENTED_EDGE ( 'NONE', *, *, #2177, .T. ) ;
#21210 = CARTESIAN_POINT ( 'NONE',  ( 116.5944421295247793, -9.863109299026486809, -13.29890625629612622 ) ) ;
#21211 = AXIS2_PLACEMENT_3D ( 'NONE', #23668, #37323, #41673 ) ;
#21212 = CARTESIAN_POINT ( 'NONE',  ( 115.2355081442453155, -10.30919188438810075, -12.61870101168855918 ) ) ;
#21213 = CARTESIAN_POINT ( 'NONE',  ( 125.1059481442452750, -1.833838273342660141, -17.42832698103878286 ) ) ;
#21214 = VERTEX_POINT ( 'NONE', #8362 ) ;
#21215 = AXIS2_PLACEMENT_3D ( 'NONE', #28968, #25096, #35557 ) ;
#21216 = PRODUCT_DEFINITION_SHAPE ( 'NONE', 'NONE',  #12711 ) ;
#21217 = CARTESIAN_POINT ( 'NONE',  ( 136.4173705901518190, 0.4780847289399532962, -11.17367218403365925 ) ) ;
#21218 = CARTESIAN_POINT ( 'NONE',  ( 123.2339681442453241, -6.344957434206665248, -7.627207830600338134 ) ) ;
#21219 = CARTESIAN_POINT ( 'NONE',  ( 105.8292077545248446, -7.250697342233347165, -7.631215200338321125 ) ) ;
#21220 = CARTESIAN_POINT ( 'NONE',  ( 119.4900081442453086, -7.643976991954077427, -18.09477374809248928 ) ) ;
#21221 = ORIENTED_EDGE ( 'NONE', *, *, #26446, .F. ) ;
#21222 = CARTESIAN_POINT ( 'NONE',  ( 113.5337081442453240, -9.261995988541697145, -16.69588392320189030 ) ) ;
#21223 = CARTESIAN_POINT ( 'NONE',  ( 124.1415948109119540, -3.505236298600246325, -18.68346056562440793 ) ) ;
#21224 = CARTESIAN_POINT ( 'NONE',  ( 79.05243529145373316, 4.793396140045460108, -21.04957699274893557 ) ) ;
#21225 = CARTESIAN_POINT ( 'NONE',  ( 59.41811746136757222, -12.82955349636864639, -9.393325708960333031 ) ) ;
#21226 = CARTESIAN_POINT ( 'NONE',  ( 124.4819548109119722, -7.893985811506177619, -18.51759400769804742 ) ) ;
#21227 = CARTESIAN_POINT ( 'NONE',  ( 123.1158699480702552, -6.365377317481717867, -18.95617363400926081 ) ) ;
#21228 = CIRCLE ( 'NONE', #35029, 3.853420195439741125 ) ;
#21229 = CARTESIAN_POINT ( 'NONE',  ( 85.45605303719084134, -15.74807682313488222, -9.893215200338316251 ) ) ;
#21230 = CARTESIAN_POINT ( 'NONE',  ( 123.6310548109119765, -5.638512984488999180, -18.83840828888717311 ) ) ;
#21232 = CARTESIAN_POINT ( 'NONE',  ( 122.6099748109119929, -0.8288870151387760510, -10.36305467784173118 ) ) ;
#21231 = CARTESIAN_POINT ( 'NONE',  ( 121.3052614775786111, -1.834011780172310813, -8.268836392978581529 ) ) ;
#21233 = CARTESIAN_POINT ( 'NONE',  ( 119.0361948109119652, -2.084020599724406786, -8.691656652584148546 ) ) ;
#21234 =( BOUNDED_SURFACE ( )  B_SPLINE_SURFACE ( 3, 2, ( 
 ( #23169, #26360, #43468 ),
 ( #12008, #33394, #8801 ),
 ( #29101, #1285, #43917 ),
 ( #39595, #25910, #12459 ),
 ( #19295, #36376, #11781 ),
 ( #9259, #39815, #19064 ),
 ( #36824, #2168, #15197 ),
 ( #22705, #22260, #5378 ),
 ( #5593, #5147, #30001 ),
 ( #12686, #5819, #37048 ),
 ( #26585, #33173, #1950 ),
 ( #15876, #29773, #43684 ) ),
 .UNSPECIFIED., .F., .F., .F. ) 
 B_SPLINE_SURFACE_WITH_KNOTS ( ( 4, 2, 2, 2, 2, 4 ),
 ( 3, 3 ),
 ( 0.001037087982888927054, 0.001174868562012537990, 0.001312649141136149143, 0.001381539430697954719, 0.001450429720259760295, 0.001588210299383371448 ),
 ( 0.000000000000000000, 1.000000000000000000 ),
 .UNSPECIFIED. ) 
 GEOMETRIC_REPRESENTATION_ITEM ( )  RATIONAL_B_SPLINE_SURFACE ( (
 ( 1.000000000000000000, 0.7071067811865475727, 1.000000000000000000),
 ( 1.000000000000000000, 0.7345423267586178584, 1.000000000000000000),
 ( 1.000000000000000000, 0.7596204909257884275, 1.000000000000000000),
 ( 1.000000000000000000, 0.8061747443791169587, 1.000000000000000000),
 ( 1.000000000000000000, 0.8273618726001445989, 1.000000000000000000),
 ( 1.000000000000000000, 0.8547411548254547631, 1.000000000000000000),
 ( 1.000000000000000000, 0.8633031996701927557, 1.000000000000000000),
 ( 1.000000000000000000, 0.8784466432148445580, 1.000000000000000000),
 ( 1.000000000000000000, 0.8850520986738202867, 1.000000000000000000),
 ( 1.000000000000000000, 0.9017204459549897910, 1.000000000000000000),
 ( 1.000000000000000000, 0.9078805346385753205, 1.000000000000000000),
 ( 1.000000000000000000, 0.9079001203735741488, 1.000000000000000000) ) ) 
 REPRESENTATION_ITEM ( '' )  SURFACE ( )  );
#21235 = CARTESIAN_POINT ( 'NONE',  ( 125.3790414775786388, -0.8658195297466895202, -10.39078908864337514 ) ) ;
#21236 = CARTESIAN_POINT ( 'NONE',  ( 114.8951481442453115, -0.4660016031367893996, -10.09054647747474043 ) ) ;
#21237 = ORIENTED_EDGE ( 'NONE', *, *, #16124, .T. ) ;
#21238 = EDGE_CURVE ( 'NONE', #23757, #13343, #4706, .T. ) ;
#21239 = CARTESIAN_POINT ( 'NONE',  ( 116.0850743346829859, -0.02132060320154255395, -12.14321520033831625 ) ) ;
#21240 = CARTESIAN_POINT ( 'NONE',  ( 115.2053796295247849, -4.863998795839590272, -8.388885654883775800 ) ) ;
#21241 = CARTESIAN_POINT ( 'NONE',  ( 110.8992858795247827, -8.402594152722688392, -9.854619843455216355 ) ) ;
#21242 = CARTESIAN_POINT ( 'NONE',  ( 113.9552233795247815, -1.325403438956436419, -9.854619843455211026 ) ) ;
#21243 = CARTESIAN_POINT ( 'NONE',  ( 125.3328548109119964, -9.261995988541697145, -16.69588392320189030 ) ) ;
#21244 = CARTESIAN_POINT ( 'NONE',  ( 125.4463081442452932, -4.153390946401325223, -8.397313243818185668 ) ) ;
#21245 = ORIENTED_EDGE ( 'NONE', *, *, #16414, .T. ) ;
#21246 = CARTESIAN_POINT ( 'NONE',  ( 111.8319081442453182, -4.153390946401321671, -8.397313243818183892 ) ) ;
#21247 = CARTESIAN_POINT ( 'NONE',  ( 113.3995983795247895, -0.7896495226426338832, -9.318865927141430916 ) ) ;
#21248 = CARTESIAN_POINT ( 'NONE',  ( 86.39381242489322688, -8.190259192973641689, -13.24321520033830879 ) ) ;
#21249 = CARTESIAN_POINT ( 'NONE',  ( 123.9714148109119805, -0.4660016031367893996, -10.09054647747474043 ) ) ;
#21250 = CARTESIAN_POINT ( 'NONE',  ( 125.9568481442452850, -6.344957434206665248, -7.627207830600338134 ) ) ;
#21251 = CYLINDRICAL_SURFACE ( 'NONE', #39490, 1.999999999999998890 ) ;
#21252 = CARTESIAN_POINT ( 'NONE',  ( 115.9162281442453235, -4.089484607189486809, -7.948022111789456723 ) ) ;
#21253 = CARTESIAN_POINT ( 'NONE',  ( 114.5803015045248117, -2.477300249445798297, -7.631215200338321125 ) ) ;
#21254 = CARTESIAN_POINT ( 'NONE',  ( 115.1359265045248605, -2.791137627527939813, -8.388885654883777576 ) ) ;
#21255 = ORIENTED_EDGE ( 'NONE', *, *, #28168, .F. ) ;
#21256 = CARTESIAN_POINT ( 'NONE',  ( 126.9276200068739655, -7.231923266987396737, -8.590624321703938193 ) ) ;
#21257 = CARTESIAN_POINT ( 'NONE',  ( 115.4624148109119943, -4.153390946401321671, -8.397313243818183892 ) ) ;
#21258 = CARTESIAN_POINT ( 'NONE',  ( 114.2711548109119803, -9.988377603198976828, -10.36322818467138340 ) ) ;
#21259 = ADVANCED_FACE ( 'NONE', ( #1291 ), #35203, .T. ) ;
#21260 = CARTESIAN_POINT ( 'NONE',  ( 114.1635827545248389, -2.477300249445798297, -19.15521520033831138 ) ) ;
#21261 = CARTESIAN_POINT ( 'NONE',  ( 106.8710046295248759, -4.863998795839590272, -18.39754474579285315 ) ) ;
#21262 = CARTESIAN_POINT ( 'NONE',  ( 120.1140014775786398, -7.894159318335828068, -9.358103419637847864 ) ) ;
#21263 = CARTESIAN_POINT ( 'NONE',  ( 119.3765548109119834, -10.15424416112533912, -14.75197769757731336 ) ) ;
#21264 = CARTESIAN_POINT ( 'NONE',  ( 125.9568481442452850, -6.344957434206665248, -7.627207830600338134 ) ) ;
#21265 = ORIENTED_EDGE ( 'NONE', *, *, #19629, .F. ) ;
#21266 = CARTESIAN_POINT ( 'NONE',  ( 124.3117748109119844, 0.1319031606808879209, -14.10382304977623669 ) ) ;
#21267 = DIRECTION ( 'NONE',  ( -0.5735764363510446051, 0.3127926500124816878, -0.7570804645221042017 ) ) ;
#21268 = CARTESIAN_POINT ( 'NONE',  ( 115.5758681442453053, -7.894159318335828068, -9.358103419637847864 ) ) ;
#21269 = ORIENTED_EDGE ( 'NONE', *, *, #18100, .T. ) ;
#21270 = CARTESIAN_POINT ( 'NONE',  ( 126.2275303246267697, -8.934542061787519529, -16.30473108686274131 ) ) ;
#21271 = LINE ( 'NONE', #6529, #16167 ) ;
#21272 = CARTESIAN_POINT ( 'NONE',  ( 110.6909265045248247, -2.791137627527939813, -8.388885654883777576 ) ) ;
#21273 = ORIENTED_EDGE ( 'NONE', *, *, #40117, .T. ) ;
#21274 = CARTESIAN_POINT ( 'NONE',  ( 120.1140014775786398, -7.894159318335828068, -9.358103419637847864 ) ) ;
#21275 = CARTESIAN_POINT ( 'NONE',  ( 114.6682414775786469, -7.894159318335828068, -9.358103419637847864 ) ) ;
#21276 = CARTESIAN_POINT ( 'NONE',  ( 124.5487329937728873, -9.861982936719853043, -13.21808400482192880 ) ) ;
#21277 = CARTESIAN_POINT ( 'NONE',  ( 122.1048610609119720, -3.163656168406935087, -18.89861972220014508 ) ) ;
#21278 = VERTEX_POINT ( 'NONE', #29107 ) ;
#21279 = CARTESIAN_POINT ( 'NONE',  ( 124.0650380271176800, -2.421111565351928618, -5.775362573634398089 ) ) ;
#21280 = CARTESIAN_POINT ( 'NONE',  ( 114.8581140045248361, -10.62599879583958717, -11.00651665394454604 ) ) ;
#21281 = CARTESIAN_POINT ( 'NONE',  ( 114.4413348109119823, -9.261995988541697145, -16.69588392320189030 ) ) ;
#21282 = CARTESIAN_POINT ( 'NONE',  ( 125.2761281442453054, 0.4262465694468514643, -12.03445270309931736 ) ) ;
#21283 = CARTESIAN_POINT ( 'NONE',  ( 116.0296814775786345, -1.833838273342658809, -17.42832698103878286 ) ) ;
#21284 = FACE_OUTER_BOUND ( 'NONE', #20560, .T. ) ;
#21285 = B_SPLINE_CURVE_WITH_KNOTS ( 'NONE', 3,
 ( #30934, #27521, #20231, #24102, #23884, #27068, #12942, #30708, #26840, #34118, #40752, #34339, #13165, #37768, #9509, #23425, #13395, #37311, #44857, #6078, #44631, #6541, #41437, #26612, #27298, #33884, #2654, #37995, #16586, #41212, #9973, #38875, #11078, #24981, #39110 ),
 .UNSPECIFIED., .F., .F.,
 ( 4, 2, 2, 1, 1, 1, 2, 2, 2, 2, 1, 1, 2, 2, 2, 2, 1, 1, 2, 2, 4 ),
 ( 0.000000000000000000, 0.1249999999996228572, 0.1874999999994343414, 0.2187499999993456345, 0.2343749999992951194, 0.2421874999992763844, 0.2460937499992742750, 0.2499999999992721378, 0.3749999999993665067, 0.4374999999994138022, 0.4687499999994378941, 0.4843749999994453881, 0.4921874999994536592, 0.4999999999994618749, 0.6249999999996362909, 0.6874999999997234434, 0.7187499999997635225, 0.7343749999997836175, 0.7421874999997902789, 0.7499999999997970512, 1.000000000000000000 ),
 .UNSPECIFIED. ) ;
#21286 = ORIENTED_EDGE ( 'NONE', *, *, #37861, .F. ) ;
#21287 = CARTESIAN_POINT ( 'NONE',  ( 114.8384214775786489, -10.15424416112533912, -14.75197769757731336 ) ) ;
#21288 = VECTOR ( 'NONE', #40850, 1000.000000000000000 ) ;
#21289 = FACE_OUTER_BOUND ( 'NONE', #2074, .T. ) ;
#21290 = CIRCLE ( 'NONE', #22005, 2.000000000000000444 ) ;
#21291 = CARTESIAN_POINT ( 'NONE',  ( 84.51109360120207725, -29.99489077589584696, -11.85273644461004672 ) ) ;
#21292 = CARTESIAN_POINT ( 'NONE',  ( 115.6915515045247531, -2.477300249445798297, -7.631215200338321125 ) ) ;
#21293 = CARTESIAN_POINT ( 'NONE',  ( 115.6893214775786447, 0.5811942927096154232, -14.16772938898807155 ) ) ;
#21294 =( REPRESENTATION_RELATIONSHIP ('NONE','NONE', #36667, #21588 ) REPRESENTATION_RELATIONSHIP_WITH_TRANSFORMATION ( #19529 )SHAPE_REPRESENTATION_RELATIONSHIP( ) );
#21295 = ORIENTED_EDGE ( 'NONE', *, *, #25124, .F. ) ;
#21296 = CARTESIAN_POINT ( 'NONE',  ( 118.2420214775786320, -3.383040157471821630, -19.15922257007629170 ) ) ;
#21297 = DIRECTION ( 'NONE',  ( 0.8949343913984423304, 0.1703803081152067689, -0.4123869368673877545 ) ) ;
#21298 = CARTESIAN_POINT ( 'NONE',  ( 110.7603796295247918, -4.863998795839590272, -19.15521520033831493 ) ) ;
#21299 = CARTESIAN_POINT ( 'NONE',  ( 114.5547881442453217, -5.638512984488999180, -18.83840828888717311 ) ) ;
#21300 = CARTESIAN_POINT ( 'NONE',  ( 113.2500748109119968, -6.344957434206662583, -7.627207830600332805 ) ) ;
#21301 =( GEOMETRIC_REPRESENTATION_CONTEXT ( 3 ) GLOBAL_UNCERTAINTY_ASSIGNED_CONTEXT ( ( #35598 ) ) GLOBAL_UNIT_ASSIGNED_CONTEXT ( ( #33697, #10012, #37802 ) ) REPRESENTATION_CONTEXT ( 'NONE', 'WORKASPACE' ) );
#21302 = CARTESIAN_POINT ( 'NONE',  ( 124.1415948109119540, -3.505236298600246325, -18.68346056562440793 ) ) ;
#21303 = CARTESIAN_POINT ( 'NONE',  ( 123.9584548109119737, -1.204716393658298523, -20.50726132761981901 ) ) ;
#21304 = CARTESIAN_POINT ( 'NONE',  ( 111.5243640045248412, 0.1403307496149616695, -15.46607636864997204 ) ) ;
#21305 = ORIENTED_EDGE ( 'NONE', *, *, #301, .T. ) ;
#21306 = CARTESIAN_POINT ( 'NONE',  ( 121.8139395652850538, -6.239497348973043422, -18.71779138178828106 ) ) ;
#21307 = CARTESIAN_POINT ( 'NONE',  ( 109.2294940316331662, -8.917758382726240995, -16.95199246166307461 ) ) ;
#21308 = CARTESIAN_POINT ( 'NONE',  ( 115.0653281442453277, -3.505236298600246325, -18.68346056562440793 ) ) ;
#21309 = EDGE_CURVE ( 'NONE', #32855, #20113, #18844, .T. ) ;
#21310 = CARTESIAN_POINT ( 'NONE',  ( 65.23579839261728353, -13.46795819349411616, -11.98898727572936451 ) ) ;
#21311 = CARTESIAN_POINT ( 'NONE',  ( 115.7610046295247912, -4.863998795839590272, -18.39754474579285315 ) ) ;
#21312 = CARTESIAN_POINT ( 'NONE',  ( 111.5243640045248412, -10.62599879583958717, -11.00651665394454604 ) ) ;
#21313 = FACE_OUTER_BOUND ( 'NONE', #14658, .T. ) ;
#21314 = CARTESIAN_POINT ( 'NONE',  ( 124.7655881442452852, 0.5811942927096110934, -14.16772938898807510 ) ) ;
#21315 = CARTESIAN_POINT ( 'NONE',  ( 138.2184548109119930, -6.243778871467079661, -12.80482167309617125 ) ) ;
#21316 = CARTESIAN_POINT ( 'NONE',  ( 124.4819548109119722, -7.893985811506177619, -18.51759400769804742 ) ) ;
#21317 = CARTESIAN_POINT ( 'NONE',  ( 116.5402214775786405, 0.2603800115204892296, -16.42320221600525088 ) ) ;
#21318 = ORIENTED_EDGE ( 'NONE', *, *, #34504, .T. ) ;
#21319 = CARTESIAN_POINT ( 'NONE',  ( 114.2711548109119803, -0.1624402480850797581, -16.17319339645315424 ) ) ;
#21320 = CARTESIAN_POINT ( 'NONE',  ( 125.7866681442452688, -0.4660016031367893996, -10.09054647747474043 ) ) ;
#21321 = CARTESIAN_POINT ( 'NONE',  ( 117.9016614775786280, -9.988377603198976828, -10.36322818467138340 ) ) ;
#21322 = CARTESIAN_POINT ( 'NONE',  ( 118.0151148109119816, 0.4262465694468514643, -12.03445270309931736 ) ) ;
#21323 = EDGE_LOOP ( 'NONE', ( #2665, #19804, #29725, #29503 ) ) ;
#21324 = CARTESIAN_POINT ( 'NONE',  ( 119.7169148109119874, -0.1624402480850797581, -16.17319339645315424 ) ) ;
#21325 = B_SPLINE_CURVE_WITH_KNOTS ( 'NONE', 3,
 ( #5233, #32812, #5452, #43096, #32594, #11865, #8888, #22346, #36240, #33480 ),
 .UNSPECIFIED., .F., .F.,
 ( 4, 3, 3, 4 ),
 ( 0.000000000000000000, 0.0002476486447138720221, 0.0004952972925464129957, 0.0009604418836934600166 ),
 .UNSPECIFIED. ) ;
#21326 = CIRCLE ( 'NONE', #14784, 2.541999999999999371 ) ;
#21327 = CARTESIAN_POINT ( 'NONE',  ( 117.5045748109119756, 0.5811942927096110934, -14.16772938898807510 ) ) ;
#21328 = CARTESIAN_POINT ( 'NONE',  ( 136.3685138707383828, 0.4973853706319558143, -15.62000875385643184 ) ) ;
#21329 = CARTESIAN_POINT ( 'NONE',  ( 110.0658483795247804, -0.7896495226426338832, -9.318865927141430916 ) ) ;
#21330 = CARTESIAN_POINT ( 'NONE',  ( 60.49017502987946671, -14.58217554126384563, -8.627207235595617973 ) ) ;
#21331 = CARTESIAN_POINT ( 'NONE',  ( 126.2364674775771647, 0.1186143222450094931, -13.91482113796701547 ) ) ;
#21332 = CARTESIAN_POINT ( 'NONE',  ( 116.6638952545248031, -9.868328341294098749, -15.46607636864997204 ) ) ;
#21333 = CIRCLE ( 'NONE', #27176, 0.5000000000000044409 ) ;
#21334 = CARTESIAN_POINT ( 'NONE',  ( 115.7460481442453357, 0.9020085738987339008, -11.91225656197089222 ) ) ;
#21335 = CARTESIAN_POINT ( 'NONE',  ( 135.9690293846602458, -10.74668130430289814, -14.11119591414773566 ) ) ;
#21336 = CARTESIAN_POINT ( 'NONE',  ( 112.1722681442453222, -8.899110576539710493, -16.42337572283490132 ) ) ;
#21337 = CARTESIAN_POINT ( 'NONE',  ( 60.46773714784079345, -12.56592564749740148, -17.32492254961432820 ) ) ;
#21338 = CARTESIAN_POINT ( 'NONE',  ( 117.1074881442453233, 0.4262465694468589028, -12.03445270309934578 ) ) ;
#21339 = CARTESIAN_POINT ( 'NONE',  ( 116.6638952545248031, -9.868328341294098749, -15.46607636864997204 ) ) ;
#21340 = CARTESIAN_POINT ( 'NONE',  ( 112.9097148109120070, -9.565557343593413364, -10.61323700422348004 ) ) ;
#21341 =( LENGTH_UNIT ( ) NAMED_UNIT ( * ) SI_UNIT ( .MILLI., .METRE. ) );
#21342 = DIRECTION ( 'NONE',  ( 1.000000000000000000, 0.000000000000000000, 0.000000000000000000 ) ) ;
#21344 = CARTESIAN_POINT ( 'NONE',  ( 116.6536748109119941, 0.9020085738987339008, -11.91225656197089222 ) ) ;
#21343 = CARTESIAN_POINT ( 'NONE',  ( 118.4122014775786340, 0.5811942927096084288, -14.16772938898808931 ) ) ;
#21345 = CARTESIAN_POINT ( 'NONE',  ( 123.9146881442452894, -10.15424416112533912, -14.75197769757731336 ) ) ;
#21346 = CARTESIAN_POINT ( 'NONE',  ( 117.5045748109119756, -9.859900752359374465, -12.68260735090039404 ) ) ;
#21347 = VERTEX_POINT ( 'NONE', #2863 ) ;
#21348 = CARTESIAN_POINT ( 'NONE',  ( 136.5935259641815094, -7.096270167259992157, -8.139588474309226385 ) ) ;
#21349 = CARTESIAN_POINT ( 'NONE',  ( 123.6877814775786533, -3.383040157471821630, -19.15922257007629170 ) ) ;
#21350 = CARTESIAN_POINT ( 'NONE',  ( 113.8857702545248003, 0.1403307496149616695, -11.32035403202665336 ) ) ;
#21351 = CARTESIAN_POINT ( 'NONE',  ( 121.0216281442452981, -7.894159318335828068, -9.358103419637847864 ) ) ;
#21352 = CARTESIAN_POINT ( 'NONE',  ( 111.4348214775786801, -3.505236298600246325, -18.68346056562440793 ) ) ;
#21353 = CARTESIAN_POINT ( 'NONE',  ( 86.44458416315558225, -26.15744216582745452, -8.393215200338314474 ) ) ;
#21354 = CARTESIAN_POINT ( 'NONE',  ( 112.6356140045247827, -10.62599879583958717, -11.00651665394454604 ) ) ;
#21355 = CARTESIAN_POINT ( 'NONE',  ( 118.7525614775786380, -1.833838273342659253, -17.42832698103878286 ) ) ;
#21356 = VECTOR ( 'NONE', #38023, 1000.000000000000227 ) ;
#21357 = CARTESIAN_POINT ( 'NONE',  ( 121.7023481442452777, -0.8288870151387760510, -10.36305467784173118 ) ) ;
#21358 = CARTESIAN_POINT ( 'NONE',  ( 114.5547881442453217, -4.153390946401313677, -8.397313243818183892 ) ) ;
#21359 = CARTESIAN_POINT ( 'NONE',  ( 109.2294668341613288, -0.5633236648423508575, -10.20431573512175483 ) ) ;
#21360 = CARTESIAN_POINT ( 'NONE',  ( 121.1325173109119788, 0.2312338769422704887, -16.08380026872395874 ) ) ;
#21361 = CARTESIAN_POINT ( 'NONE',  ( 108.8851452545248151, -9.868328341294098749, -15.46607636864997204 ) ) ;
#21362 = CARTESIAN_POINT ( 'NONE',  ( 117.2190380802938137, 1.225124243697611526, -21.63543231393177280 ) ) ;
#21363 = CARTESIAN_POINT ( 'NONE',  ( 116.7671281442453335, -1.834011780172310813, -8.268836392978581529 ) ) ;
#21364 = CARTESIAN_POINT ( 'NONE',  ( 116.4267681442453153, -3.383040157471821630, -19.15922257007629170 ) ) ;
#21365 = CARTESIAN_POINT ( 'NONE',  ( 109.0935046295247872, -4.863998795839590272, -7.631215200338315796 ) ) ;
#21366 = CARTESIAN_POINT ( 'NONE',  ( 113.4202548109119846, -10.30919188438810075, -12.61870101168855918 ) ) ;
#21367 = ORIENTED_EDGE ( 'NONE', *, *, #13999, .T. ) ;
#21368 = CARTESIAN_POINT ( 'NONE',  ( 86.36631847702263087, -25.99489077589524300, -13.39321520033831447 ) ) ;
#21369 = CONICAL_SURFACE ( 'NONE', #245, 2.000000000000000444, 0.9599310885968830309 ) ;
#21370 = CARTESIAN_POINT ( 'NONE',  ( 122.6667014775786413, -7.893985811506177619, -18.51759400769804742 ) ) ;
#21371 = CARTESIAN_POINT ( 'NONE',  ( 115.2922348109119781, -10.63000616557722466, -14.87417383870573495 ) ) ;
#21372 = CARTESIAN_POINT ( 'NONE',  ( 121.8725281442453223, -6.222761293078241884, -8.102969835052219238 ) ) ;
#21373 = CARTESIAN_POINT ( 'NONE',  ( 111.4915481442453142, -1.833838273342658365, -17.42832698103878286 ) ) ;
#21374 = CARTESIAN_POINT ( 'NONE',  ( 122.6667014775786413, -7.893985811506177619, -18.51759400769804742 ) ) ;
#21375 = ADVANCED_FACE ( 'NONE', ( #44380 ), #19933, .T. ) ;
#21376 = CARTESIAN_POINT ( 'NONE',  ( 115.1359265045248605, -7.250697342233347165, -19.15521520033831138 ) ) ;
#21377 = CARTESIAN_POINT ( 'NONE',  ( 115.2922348109119781, 0.4262465694468514643, -12.03445270309931736 ) ) ;
#21378 = CARTESIAN_POINT ( 'NONE',  ( 87.68939540009954214, -25.99489077589524300, -13.39321520033831447 ) ) ;
#21379 = ORIENTED_EDGE ( 'NONE', *, *, #36438, .F. ) ;
#21380 = CARTESIAN_POINT ( 'NONE',  ( 123.2906948109119867, -8.166667518702819706, -8.995218007635861213 ) ) ;
#21381 = AXIS2_PLACEMENT_3D ( 'NONE', #12755, #41035, #40570 ) ;
#21382 = CARTESIAN_POINT ( 'NONE',  ( 123.2855641859119942, -0.8832429491016019485, -18.19431474523657855 ) ) ;
#21383 = CARTESIAN_POINT ( 'NONE',  ( 118.7525614775786380, -8.166667518702819706, -8.995218007635861213 ) ) ;
#21384 = ORIENTED_EDGE ( 'NONE', *, *, #44070, .F. ) ;
#21385 = CARTESIAN_POINT ( 'NONE',  ( 115.3442858795247759, -0.7896495226426338832, -17.46756447353520159 ) ) ;
#21386 = AXIS2_PLACEMENT_3D ( 'NONE', #22148, #35589, #18508 ) ;
#21387 = CARTESIAN_POINT ( 'NONE',  ( 123.6877814775786533, -3.383040157471821630, -19.15922257007629170 ) ) ;
#21388 = CARTESIAN_POINT ( 'NONE',  ( 120.0214764273310095, -2.236191541394345172, -18.14152338500401029 ) ) ;
#21389 = CARTESIAN_POINT ( 'NONE',  ( 116.1431348109119881, 0.1319031606808879209, -14.10382304977623669 ) ) ;
#21390 = ADVANCED_FACE ( 'NONE', ( #16793 ), #26366, .F. ) ;
#21391 = DIRECTION ( 'NONE',  ( 0.000000000000000000, 0.000000000000000000, 1.000000000000000000 ) ) ;
#21392 = CARTESIAN_POINT ( 'NONE',  ( 118.2987481442453088, -7.894159318335828068, -9.358103419637847864 ) ) ;
#21393 = EDGE_CURVE ( 'NONE', #12130, #8541, #5339, .T. ) ;
#21394 = ADVANCED_FACE ( 'NONE', ( #12692 ), #30559, .T. ) ;
#21395 = FACE_OUTER_BOUND ( 'NONE', #18748, .T. ) ;
#21396 = CARTESIAN_POINT ( 'NONE',  ( 119.8870948109119752, -0.8288870151387760510, -10.36305467784173118 ) ) ;
#21397 = AXIS2_PLACEMENT_3D ( 'NONE', #12435, #43659, #1476 ) ;
#21398 = CARTESIAN_POINT ( 'NONE',  ( 123.9584548109119737, -12.48189245497263755, -10.95032834292243074 ) ) ;
#21399 = CARTESIAN_POINT ( 'NONE',  ( 118.8092881442453290, -0.1624402480850797581, -16.17319339645315424 ) ) ;
#21400 = CARTESIAN_POINT ( 'NONE',  ( 121.0630641859119976, -0.8832429491016019485, -18.19431474523657855 ) ) ;
#21401 = CARTESIAN_POINT ( 'NONE',  ( 116.5969481442453031, 0.5811942927096154232, -14.16772938898807155 ) ) ;
#21402 = CARTESIAN_POINT ( 'NONE',  ( 113.2500748109119968, -6.344957434206662583, -7.627207830600332805 ) ) ;
#21403 = CARTESIAN_POINT ( 'NONE',  ( 78.69189222814998175, -82.08636712479707853, -32.64558696907351987 ) ) ;
#21404 = CARTESIAN_POINT ( 'NONE',  ( 120.1140014775786398, -7.894159318335828068, -9.358103419637847864 ) ) ;
#21405 = ORIENTED_EDGE ( 'NONE', *, *, #13329, .F. ) ;
#21406 = CARTESIAN_POINT ( 'NONE',  ( 116.5969481442453031, 0.5811942927096154232, -14.16772938898807155 ) ) ;
#21407 = CARTESIAN_POINT ( 'NONE',  ( 112.1494421295248003, -9.868328341294093420, -13.39321520033831447 ) ) ;
#21408 = DIRECTION ( 'NONE',  ( -0.000000000000000000, -0.9284778069183721172, -0.3713878862591650232 ) ) ;
#21409 = DIRECTION ( 'NONE',  ( -0.000000000000000000, -0.9284778069183721172, -0.3713878862591650232 ) ) ;
#21410 = CARTESIAN_POINT ( 'NONE',  ( 127.9644000028953030, -4.197576873768148253, -15.52951870415910207 ) ) ;
#21411 = CARTESIAN_POINT ( 'NONE',  ( 121.9859814775786333, 0.2603800115204892296, -16.42320221600525088 ) ) ;
#21412 = ORIENTED_EDGE ( 'NONE', *, *, #7719, .T. ) ;
#21413 = CARTESIAN_POINT ( 'NONE',  ( 87.44708369096657918, -21.99489077589588604, -7.893215200338315363 ) ) ;
#21414 = CARTESIAN_POINT ( 'NONE',  ( 122.3263414775786373, -3.505236298600246325, -18.68346056562440793 ) ) ;
#21415 = CARTESIAN_POINT ( 'NONE',  ( 59.24641515291911986, -13.72835195454734247, -19.39321520033831447 ) ) ;
#21416 = CARTESIAN_POINT ( 'NONE',  ( 125.4463081442452932, -5.638512984488999180, -18.83840828888717311 ) ) ;
#21417 = CARTESIAN_POINT ( 'NONE',  ( 112.9134265045247645, -2.791137627527939813, -8.388885654883777576 ) ) ;
#21418 = ADVANCED_FACE ( 'NONE', ( #35545 ), #8995, .T. ) ;
#21419 = EDGE_LOOP ( 'NONE', ( #9900, #21412, #5502, #29386, #37624 ) ) ;
#21420 = CARTESIAN_POINT ( 'NONE',  ( 116.3700414775786527, -5.638512984488999180, -18.83840828888717311 ) ) ;
#21421 = CARTESIAN_POINT ( 'NONE',  ( 125.8433948109119456, -7.643976991954077427, -18.09477374809248928 ) ) ;
#21422 = CARTESIAN_POINT ( 'NONE',  ( 124.1983214775786166, -8.166667518702819706, -8.995218007635861213 ) ) ;
#21423 = CARTESIAN_POINT ( 'NONE',  ( 121.7590748109119687, -2.084020599724406786, -8.691656652584148546 ) ) ;
#21424 = DIRECTION ( 'NONE',  ( 0.000000000000000000, 0.000000000000000000, -1.000000000000000000 ) ) ;
#21425 = PRESENTATION_STYLE_ASSIGNMENT (( #31456 ) ) ;
#21426 = CARTESIAN_POINT ( 'NONE',  ( 124.0281414775786146, -1.834011780172310813, -8.268836392978581529 ) ) ;
#21427 = CARTESIAN_POINT ( 'NONE',  ( 111.8991748109119868, -7.866424907533402511, -9.395035934245173692 ) ) ;
#21428 = DIRECTION ( 'NONE',  ( 0.9908103287288504424, -0.1352586133457950590, 0.000000000000000000 ) ) ;
#21429 = CARTESIAN_POINT ( 'NONE',  ( 84.49707967414211396, -25.99489077589524300, -13.39321520033831625 ) ) ;
#21430 = EDGE_CURVE ( 'NONE', #19108, #17596, #32578, .T. ) ;
#21431 = CARTESIAN_POINT ( 'NONE',  ( 125.2761281442453054, 0.4262465694468514643, -12.03445270309931736 ) ) ;
#21432 = ORIENTED_EDGE ( 'NONE', *, *, #41306, .T. ) ;
#21433 = MANIFOLD_SOLID_BREP ( 'NONE', #1747 ) ;
#21434 = ADVANCED_FACE ( 'NONE', ( #43080 ), #44560, .T. ) ;
#21435 = CARTESIAN_POINT ( 'NONE',  ( 116.2471765045247594, -2.791137627527939813, -8.388885654883777576 ) ) ;
#21436 = CARTESIAN_POINT ( 'NONE',  ( 120.2841814775786276, 0.9020085738987339008, -11.91225656197089222 ) ) ;
#21437 = CARTESIAN_POINT ( 'NONE',  ( 123.2339681442453241, -3.505236298600246325, -18.68346056562440793 ) ) ;
#21438 = EDGE_LOOP ( 'NONE', ( #14422, #11185, #40731, #33356 ) ) ;
#21439 = CARTESIAN_POINT ( 'NONE',  ( 76.69189222814998175, -50.16718729050181480, 3.106784799661685526 ) ) ;
#21440 = CARTESIAN_POINT ( 'NONE',  ( 123.2906948109119867, -8.166667518702819706, -8.995218007635861213 ) ) ;
#21441 = CARTESIAN_POINT ( 'NONE',  ( 106.8015515045248378, -2.477300249445798297, -7.631215200338321125 ) ) ;
#21442 = CARTESIAN_POINT ( 'NONE',  ( 122.2128881442453263, -7.643976991954077427, -18.09477374809248928 ) ) ;
#21443 = AXIS2_PLACEMENT_3D ( 'NONE', #28198, #38653, #24989 ) ;
#21444 = VERTEX_POINT ( 'NONE', #16 ) ;
#21445 = CARTESIAN_POINT ( 'NONE',  ( 115.2922348109119781, -10.63000616557722466, -14.87417383870573495 ) ) ;
#21446 = CARTESIAN_POINT ( 'NONE',  ( 90.45092582798827152, -25.23119213852205789, -15.24166438581092109 ) ) ;
#21447 = CARTESIAN_POINT ( 'NONE',  ( 86.75477599865929790, -25.99489077589524300, -13.39321520033831625 ) ) ;
#21448 = EDGE_CURVE ( 'NONE', #11237, #22820, #11641, .T. ) ;
#21449 = CARTESIAN_POINT ( 'NONE',  ( 135.9373687277988836, -5.586066061336491195, -7.503848139453651811 ) ) ;
#21450 = VECTOR ( 'NONE', #37881, 1000.000000000000227 ) ;
#21451 = CARTESIAN_POINT ( 'NONE',  ( 111.7184548109119788, -0.8288870151387760510, -10.36305467784173118 ) ) ;
#21452 = CARTESIAN_POINT ( 'NONE',  ( 69.69189222814998175, -41.76310523276723785, -20.39321520033831447 ) ) ;
#21453 = FACE_OUTER_BOUND ( 'NONE', #43644, .T. ) ;
#21454 = CARTESIAN_POINT ( 'NONE',  ( 122.0994348109119443, 0.9020085738987339008, -11.91225656197089222 ) ) ;
#21456 = CARTESIAN_POINT ( 'NONE',  ( 124.0281414775786146, -7.643976991954077427, -18.09477374809248928 ) ) ;
#21455 = CARTESIAN_POINT ( 'NONE',  ( 121.8725281442453223, -3.383040157471821630, -19.15922257007629170 ) ) ;
#21457 = CARTESIAN_POINT ( 'NONE',  ( 118.4122014775786340, -9.859900752359374465, -12.68260735090039404 ) ) ;
#21458 = CARTESIAN_POINT ( 'NONE',  ( 68.68839935636916039, -25.95913848132418522, -5.893215200338315363 ) ) ;
#21459 = CARTESIAN_POINT ( 'NONE',  ( 118.3554748109119998, 0.2603800115204892296, -16.42320221600525088 ) ) ;
#21460 = ORIENTED_EDGE ( 'NONE', *, *, #42866, .T. ) ;
#21461 = ORIENTED_EDGE ( 'NONE', *, *, #42966, .T. ) ;
#21462 = CARTESIAN_POINT ( 'NONE',  ( 113.2226630180080775, 0.7607806665038616689, -14.64321520033831447 ) ) ;
#21463 = CARTESIAN_POINT ( 'NONE',  ( 125.6164881442453094, -9.565557343593953377, -10.61323700422440197 ) ) ;
#21464 = CARTESIAN_POINT ( 'NONE',  ( 112.4967077545247633, -2.791137627527939813, -18.39754474579286025 ) ) ;
#21465 = CARTESIAN_POINT ( 'NONE',  ( 107.4960827545248350, -6.936859964151250502, -8.388885654883777576 ) ) ;
#21466 = CARTESIAN_POINT ( 'NONE',  ( 114.5108483795247878, -8.402594152722688392, -16.93181055722141792 ) ) ;
#21467 = CARTESIAN_POINT ( 'NONE',  ( 125.5597614775786326, -1.561330072975669392, -17.79121239304076951 ) ) ;
#21468 = CARTESIAN_POINT ( 'NONE',  ( 112.4559014775786494, -9.988377603198976828, -10.36322818467138340 ) ) ;
#21469 = VERTEX_POINT ( 'NONE', #18242 ) ;
#21470 = CARTESIAN_POINT ( 'NONE',  ( 112.7962614775786676, -6.222761293078241884, -8.102969835052219238 ) ) ;
#21471 = CARTESIAN_POINT ( 'NONE',  ( 110.4825671295247815, -10.62599879583958540, -13.39321520033831447 ) ) ;
#21472 = LINE ( 'NONE', #42228, #9599 ) ;
#21473 = CARTESIAN_POINT ( 'NONE',  ( 120.1028830209070293, -6.157706758239399392, -18.56290235964623392 ) ) ;
#21474 = CARTESIAN_POINT ( 'NONE',  ( 123.4041481442452834, -10.30919188438810075, -12.61870101168855918 ) ) ;
#21475 = FACE_OUTER_BOUND ( 'NONE', #31141, .T. ) ;
#21476 = CARTESIAN_POINT ( 'NONE',  ( 115.5191414775786569, -3.383040157471821630, -19.15922257007629170 ) ) ;
#21477 = CARTESIAN_POINT ( 'NONE',  ( 114.6497546295247929, -4.863998795839590272, -7.631215200338315796 ) ) ;
#21478 = CARTESIAN_POINT ( 'NONE',  ( 113.1217858795247935, -8.402594152722688392, -9.854619843455216355 ) ) ;
#21479 = ORIENTED_EDGE ( 'NONE', *, *, #31983, .T. ) ;
#21480 = CARTESIAN_POINT ( 'NONE',  ( -6.962123463324038752, -11.49046785505262669, -8.593215200338315540 ) ) ;
#21481 = CARTESIAN_POINT ( 'NONE',  ( 116.5402214775786405, -9.565557343593413364, -10.61323700422348004 ) ) ;
#21482 = CARTESIAN_POINT ( 'NONE',  ( 126.5241148109119393, -9.565557343593413364, -10.61323700422348004 ) ) ;
#21483 = CARTESIAN_POINT ( 'NONE',  ( 113.1366214775786432, -1.834011780172310813, -8.268836392978581529 ) ) ;
#21484 = FACE_OUTER_BOUND ( 'NONE', #22395, .T. ) ;
#21485 = CARTESIAN_POINT ( 'NONE',  ( 118.3554748109119998, -9.565557343593413364, -10.61323700422348004 ) ) ;
#21486 = CARTESIAN_POINT ( 'NONE',  ( 114.1009748109119784, -5.574606645277164318, -18.38911715685844683 ) ) ;
#21487 = ORIENTED_EDGE ( 'NONE', *, *, #41286, .T. ) ;
#21488 = AXIS2_PLACEMENT_3D ( 'NONE', #9012, #43216, #22682 ) ;
#21489 = CARTESIAN_POINT ( 'NONE',  ( 125.3328548109119964, -0.8288870151387760510, -10.36305467784173118 ) ) ;
#21490 = LINE ( 'NONE', #42696, #38240 ) ;
#21491 = CARTESIAN_POINT ( 'NONE',  ( 113.8740681442453138, -9.859900752359374465, -12.68260735090039404 ) ) ;
#21492 = ORIENTED_EDGE ( 'NONE', *, *, #25481, .F. ) ;
#21493 = CARTESIAN_POINT ( 'NONE',  ( 126.4852516627922085, -9.308055734194462971, -15.96268377075503153 ) ) ;
#21494 = EDGE_CURVE ( 'NONE', #23361, #19352, #19209, .T. ) ;
#21495 = CARTESIAN_POINT ( 'NONE',  ( 106.3848327545248651, -2.477300249445798297, -19.15521520033831138 ) ) ;
#21496 = CARTESIAN_POINT ( 'NONE',  ( 111.5243640045248412, 0.1403307496149616695, -15.46607636864997204 ) ) ;
#21497 = CARTESIAN_POINT ( 'NONE',  ( 122.8368814775786291, -7.894159318335828068, -9.358103419637847864 ) ) ;
#21498 = ORIENTED_EDGE ( 'NONE', *, *, #43714, .F. ) ;
#21499 = CARTESIAN_POINT ( 'NONE',  ( 118.8660148109119774, 0.1319031606808879209, -14.10382304977623669 ) ) ;
#21500 = CARTESIAN_POINT ( 'NONE',  ( 118.2420214775786320, -6.222761293078241884, -8.102969835052219238 ) ) ;
#21501 =( BOUNDED_SURFACE ( )  B_SPLINE_SURFACE ( 1, 2, ( 
 ( #33878, #12705, #37305, #8601, #43488, #6071, #22722, #5166, #19083, #8821, #32969, #41651, #10409, #24094, #38420, #38202, #41431, #41205, #20889, #45063, #34549, #9966, #3546, #27513, #6981, #44851, #24318, #132, #31359, #13822, #13604, #34333, #3107, #30924, #14044, #27737, #34110, #37533, #37988, #10188, #6764, #17461, #23877, #6306, #34767, #13388, #30474, #3331, #44394, #44622, #27962, #41869, #20224, #20673, #21099, #7191, #17252, #37763, #31140, #10629, #2880, #24533, #30702, #34977, #16579, #13158, #27060, #9736, #16809, #40980, #23646, #27292, #6532, #20450, #17034, #794, #7873, #3987, #21553, #11296, #32028, #35441, #11526, #7409, #35894, #1023, #21781, #18583, #24975, #38635, #14716, #38870, #32255, #10850, #21329, #35215, #17910, #11071, #35672, #28851, #42763, #17687, #28627, #25432, #31807, #39333, #7639, #28399, #8100, #4217, #24748, #42536, #25206, #31585, #18363, #18133, #39103, #4445, #22001, #4663, #579, #14488, #42090, #14940, #3764, #353, #14266, #28183, #42311, #6462, #44994, #34691, #3033, #37689, #34472, #3251, #41575, #10335, #34258, #17395, #56, #13970, #34903, #24672, #38131, #21030, #3479, #41796, #20813, #30848, #27882, #27662, #10554, #13753, #17833, #7120, #28107, #44541, #42011, #41360, #13304 ),
 ( #31283, #6686, #9889, #44771, #7335, #37908, #27211, #41129, #16954, #24238, #24452, #38343, #6902, #21254, #3692, #17614, #24020, #31506, #278, #14188, #20597, #10776, #38559, #35133, #3914, #23799, #20371, #13531, #27438, #10117, #17177, #31066, #948, #15307, #28998, #4138, #7564, #8016, #25357, #21923, #32626, #11224, #21478, #8244, #28554, #500, #4588, #14412, #14636, #29215, #1392, #35363, #11451, #36269, #22373, #5037, #39480, #43125, #31730, #11894, #42459, #28322, #11668, #35816, #42234, #24899, #10998, #38792, #18059, #31950, #14866, #25796, #18511, #32401, #22151, #39705, #28775, #36043, #32178, #8470, #4362, #35592, #25130, #4812, #1172, #42906, #715, #15087, #25576, #39025, #18733, #7796, #21705, #18282, #42683, #39251, #6081, #9290, #5851, #2656, #17042, #30710, #19773, #23198, #9744, #27070, #23656, #34341, #12944, #37077, #9975, #30257, #2202, #6314, #16130, #16355, #30936, #3117, #33655, #13167, #37997, #24104, #16589, #9511, #20233, #44859, #2431, #44403, #44183, #13614, #16818, #27523, #41439, #26614, #26842, #40992, #40528, #40754, #10197, #23428, #37313, #37542, #44633, #20002, #30482, #34120, #2889, #13398, #6772, #33886, #33424, #6543, #27300, #30033, #41215, #23886, #37770, #20459, #43947, #12714, #38430 ) ),
 .UNSPECIFIED., .F., .F., .F. ) 
 B_SPLINE_SURFACE_WITH_KNOTS ( ( 2, 2 ),
 ( 3, 2, 2, 2, 2, 2, 2, 2, 2, 2, 2, 2, 2, 2, 2, 2, 2, 2, 2, 2, 2, 2, 2, 2, 2, 2, 2, 2, 2, 2, 2, 2, 2, 2, 2, 2, 2, 2, 2, 2, 2, 2, 2, 2, 2, 2, 2, 2, 2, 2, 2, 2, 2, 2, 2, 2, 2, 2, 2, 2, 2, 2, 2, 2, 2, 2, 2, 2, 2, 2, 2, 2, 2, 2, 2, 2, 2, 2, 2, 2, 3 ),
 ( 0.000000000000000000, 1.000000000000000000 ),
 ( 0.000000000000000000, 0.01250000000000000069, 0.02500000000000000139, 0.03749999999999999861, 0.05000000000000000278, 0.06250000000000000000, 0.07499999999999999722, 0.08749999999999999445, 0.1000000000000000056, 0.1125000000000000028, 0.1250000000000000000, 0.1375000000000000111, 0.1499999999999999944, 0.1625000000000000056, 0.1749999999999999889, 0.1875000000000000000, 0.2000000000000000111, 0.2124999999999999944, 0.2250000000000000056, 0.2374999999999999889, 0.2500000000000000000, 0.2625000000000000111, 0.2750000000000000222, 0.2874999999999999778, 0.2999999999999999889, 0.3125000000000000000, 0.3250000000000000111, 0.3375000000000000222, 0.3499999999999999778, 0.3624999999999999889, 0.3750000000000000000, 0.3875000000000000111, 0.4000000000000000222, 0.4124999999999999778, 0.4249999999999999889, 0.4375000000000000000, 0.4500000000000000111, 0.4625000000000000222, 0.4749999999999999778, 0.4874999999999999889, 0.5000000000000000000, 0.5124999999999999556, 0.5250000000000000222, 0.5374999999999999778, 0.5500000000000000444, 0.5625000000000000000, 0.5749999999999999556, 0.5875000000000000222, 0.5999999999999999778, 0.6125000000000000444, 0.6250000000000000000, 0.6374999999999999556, 0.6500000000000000222, 0.6624999999999999778, 0.6750000000000000444, 0.6875000000000000000, 0.6999999999999999556, 0.7125000000000000222, 0.7249999999999999778, 0.7375000000000000444, 0.7500000000000000000, 0.7624999999999999556, 0.7750000000000000222, 0.7874999999999999778, 0.8000000000000000444, 0.8125000000000000000, 0.8249999999999999556, 0.8375000000000000222, 0.8499999999999999778, 0.8625000000000000444, 0.8750000000000000000, 0.8874999999999999556, 0.9000000000000000222, 0.9124999999999999778, 0.9250000000000000444, 0.9375000000000000000, 0.9499999999999999556, 0.9625000000000000222, 0.9749999999999999778, 0.9875000000000000444, 1.000000000000000000 ),
 .UNSPECIFIED. ) 
 GEOMETRIC_REPRESENTATION_ITEM ( )  RATIONAL_B_SPLINE_SURFACE ( (
 ( 1.000000000000000000, 0.9238795325112869605, 1.000000000000000000, 0.9238795325112869605, 1.000000000000000000, 0.9238795325112869605, 1.000000000000000000, 0.9238795325112869605, 1.000000000000000000, 0.9238795325112869605, 1.000000000000000000, 0.9238795325112869605, 1.000000000000000000, 0.9238795325112869605, 1.000000000000000000, 0.9238795325112869605, 1.000000000000000000, 0.9238795325112869605, 1.000000000000000000, 0.9238795325112869605, 1.000000000000000000, 0.9238795325112869605, 1.000000000000000000, 0.9238795325112869605, 1.000000000000000000, 0.9238795325112869605, 1.000000000000000000, 0.9238795325112869605, 1.000000000000000000, 0.9238795325112869605, 1.000000000000000000, 0.9238795325112869605, 1.000000000000000000, 0.9238795325112869605, 1.000000000000000000, 0.9238795325112869605, 1.000000000000000000, 0.9238795325112869605, 1.000000000000000000, 0.9238795325112869605, 1.000000000000000000, 0.9238795325112869605, 1.000000000000000000, 0.9238795325112869605, 1.000000000000000000, 0.9238795325112869605, 1.000000000000000000, 0.9238795325112869605, 1.000000000000000000, 0.9238795325112869605, 1.000000000000000000, 0.9238795325112869605, 1.000000000000000000, 0.9238795325112869605, 1.000000000000000000, 0.9238795325112869605, 1.000000000000000000, 0.9238795325112869605, 1.000000000000000000, 0.9238795325112869605, 1.000000000000000000, 0.9238795325112869605, 1.000000000000000000, 0.9238795325112869605, 1.000000000000000000, 0.9238795325112869605, 1.000000000000000000, 0.9238795325112869605, 1.000000000000000000, 0.9238795325112869605, 1.000000000000000000, 0.9238795325112869605, 1.000000000000000000, 0.9238795325112869605, 1.000000000000000000, 0.9238795325112869605, 1.000000000000000000, 0.9238795325112869605, 1.000000000000000000, 0.9238795325112869605, 1.000000000000000000, 0.9238795325112869605, 1.000000000000000000, 0.9238795325112869605, 1.000000000000000000, 0.9238795325112869605, 1.000000000000000000, 0.9238795325112869605, 1.000000000000000000, 0.9238795325112869605, 1.000000000000000000, 0.9238795325112869605, 1.000000000000000000, 0.9238795325112869605, 1.000000000000000000, 0.9238795325112869605, 1.000000000000000000, 0.9238795325112869605, 1.000000000000000000, 0.9238795325112869605, 1.000000000000000000, 0.9238795325112869605, 1.000000000000000000, 0.9238795325112869605, 1.000000000000000000, 0.9238795325112869605, 1.000000000000000000, 0.9238795325112869605, 1.000000000000000000, 0.9238795325112869605, 1.000000000000000000, 0.9238795325112869605, 1.000000000000000000, 0.9238795325112869605, 1.000000000000000000, 0.9238795325112869605, 1.000000000000000000, 0.9238795325112869605, 1.000000000000000000, 0.9238795325112869605, 1.000000000000000000, 0.9238795325112869605, 1.000000000000000000, 0.9238795325112869605, 1.000000000000000000, 0.9238795325112869605, 1.000000000000000000, 0.9238795325112869605, 1.000000000000000000, 0.9238795325112869605, 1.000000000000000000, 0.9238795325112869605, 1.000000000000000000, 0.9238795325112869605, 1.000000000000000000, 0.9238795325112869605, 1.000000000000000000, 0.9238795325112869605, 1.000000000000000000, 0.9238795325112869605, 1.000000000000000000, 0.9238795325112869605, 1.000000000000000000, 0.9238795325112869605, 1.000000000000000000, 0.9238795325112869605, 1.000000000000000000, 0.9238795325112869605, 1.000000000000000000, 0.9238795325112869605, 1.000000000000000000, 0.9238795325112869605, 1.000000000000000000, 0.9238795325112869605, 1.000000000000000000, 0.9238795325112869605, 1.000000000000000000, 0.9238795325112869605, 1.000000000000000000, 0.9238795325112869605, 1.000000000000000000),
 ( 1.000000000000000000, 0.9238795325112869605, 1.000000000000000000, 0.9238795325112869605, 1.000000000000000000, 0.9238795325112869605, 1.000000000000000000, 0.9238795325112869605, 1.000000000000000000, 0.9238795325112869605, 1.000000000000000000, 0.9238795325112869605, 1.000000000000000000, 0.9238795325112869605, 1.000000000000000000, 0.9238795325112869605, 1.000000000000000000, 0.9238795325112869605, 1.000000000000000000, 0.9238795325112869605, 1.000000000000000000, 0.9238795325112869605, 1.000000000000000000, 0.9238795325112869605, 1.000000000000000000, 0.9238795325112869605, 1.000000000000000000, 0.9238795325112869605, 1.000000000000000000, 0.9238795325112869605, 1.000000000000000000, 0.9238795325112869605, 1.000000000000000000, 0.9238795325112869605, 1.000000000000000000, 0.9238795325112869605, 1.000000000000000000, 0.9238795325112869605, 1.000000000000000000, 0.9238795325112869605, 1.000000000000000000, 0.9238795325112869605, 1.000000000000000000, 0.9238795325112869605, 1.000000000000000000, 0.9238795325112869605, 1.000000000000000000, 0.9238795325112869605, 1.000000000000000000, 0.9238795325112869605, 1.000000000000000000, 0.9238795325112869605, 1.000000000000000000, 0.9238795325112869605, 1.000000000000000000, 0.9238795325112869605, 1.000000000000000000, 0.9238795325112869605, 1.000000000000000000, 0.9238795325112869605, 1.000000000000000000, 0.9238795325112869605, 1.000000000000000000, 0.9238795325112869605, 1.000000000000000000, 0.9238795325112869605, 1.000000000000000000, 0.9238795325112869605, 1.000000000000000000, 0.9238795325112869605, 1.000000000000000000, 0.9238795325112869605, 1.000000000000000000, 0.9238795325112869605, 1.000000000000000000, 0.9238795325112869605, 1.000000000000000000, 0.9238795325112869605, 1.000000000000000000, 0.9238795325112869605, 1.000000000000000000, 0.9238795325112869605, 1.000000000000000000, 0.9238795325112869605, 1.000000000000000000, 0.9238795325112869605, 1.000000000000000000, 0.9238795325112869605, 1.000000000000000000, 0.9238795325112869605, 1.000000000000000000, 0.9238795325112869605, 1.000000000000000000, 0.9238795325112869605, 1.000000000000000000, 0.9238795325112869605, 1.000000000000000000, 0.9238795325112869605, 1.000000000000000000, 0.9238795325112869605, 1.000000000000000000, 0.9238795325112869605, 1.000000000000000000, 0.9238795325112869605, 1.000000000000000000, 0.9238795325112869605, 1.000000000000000000, 0.9238795325112869605, 1.000000000000000000, 0.9238795325112869605, 1.000000000000000000, 0.9238795325112869605, 1.000000000000000000, 0.9238795325112869605, 1.000000000000000000, 0.9238795325112869605, 1.000000000000000000, 0.9238795325112869605, 1.000000000000000000, 0.9238795325112869605, 1.000000000000000000, 0.9238795325112869605, 1.000000000000000000, 0.9238795325112869605, 1.000000000000000000, 0.9238795325112869605, 1.000000000000000000, 0.9238795325112869605, 1.000000000000000000, 0.9238795325112869605, 1.000000000000000000, 0.9238795325112869605, 1.000000000000000000, 0.9238795325112869605, 1.000000000000000000, 0.9238795325112869605, 1.000000000000000000, 0.9238795325112869605, 1.000000000000000000, 0.9238795325112869605, 1.000000000000000000, 0.9238795325112869605, 1.000000000000000000, 0.9238795325112869605, 1.000000000000000000, 0.9238795325112869605, 1.000000000000000000, 0.9238795325112869605, 1.000000000000000000, 0.9238795325112869605, 1.000000000000000000, 0.9238795325112869605, 1.000000000000000000, 0.9238795325112869605, 1.000000000000000000, 0.9238795325112869605, 1.000000000000000000, 0.9238795325112869605, 1.000000000000000000, 0.9238795325112869605, 1.000000000000000000) ) ) 
 REPRESENTATION_ITEM ( '' )  SURFACE ( )  );
#21502 = CARTESIAN_POINT ( 'NONE',  ( 124.5476740651314884, -9.860788299936581680, -13.18793303030140329 ) ) ;
#21503 = CARTESIAN_POINT ( 'NONE',  ( 122.9382985609119743, -10.36940331770106916, -15.09355782777062061 ) ) ;
#21504 = EDGE_LOOP ( 'NONE', ( #34870, #36556, #5537, #22541, #1196, #44251 ) ) ;
#21505 = LINE ( 'NONE', #305, #31757 ) ;
#21506 = CARTESIAN_POINT ( 'NONE',  ( 125.3296504289734798, -1.968006290854414697, -6.888848368006928347 ) ) ;
#21507 = VECTOR ( 'NONE', #5405, 1000.000000000000000 ) ;
#21508 = CARTESIAN_POINT ( 'NONE',  ( 112.2188952545247531, 0.8980012041604421569, -11.00651665394454071 ) ) ;
#21509 = CARTESIAN_POINT ( 'NONE',  ( 112.3991748109119868, -8.166667518702817929, -8.995218007635859436 ) ) ;
#21510 = ADVANCED_FACE ( 'NONE', ( #1571 ), #24432, .T. ) ;
#21511 = CARTESIAN_POINT ( 'NONE',  ( 116.6536748109119941, -10.15424416112533912, -14.75197769757731336 ) ) ;
#21512 = DIRECTION ( 'NONE',  ( 0.000000000000000000, 0.7996358532186281787, 0.6004852223388320587 ) ) ;
#21513 = ORIENTED_EDGE ( 'NONE', *, *, #35998, .T. ) ;
#21514 = VECTOR ( 'NONE', #14005, 1000.000000000000227 ) ;
#21515 = CARTESIAN_POINT ( 'NONE',  ( 116.5402214775786405, -9.565557343593413364, -10.61323700422348004 ) ) ;
#21516 = CYLINDRICAL_SURFACE ( 'NONE', #18981, 6.000000000000003553 ) ;
#21517 = CARTESIAN_POINT ( 'NONE',  ( 85.21058564945587932, -28.08891145889253593, -8.461176451080145711 ) ) ;
#21518 = CARTESIAN_POINT ( 'NONE',  ( 115.1359265045248605, -7.250697342233347165, -19.15521520033831138 ) ) ;
#21519 = CARTESIAN_POINT ( 'NONE',  ( 115.1220548109119761, -8.166667518702817929, -8.995218007635861213 ) ) ;
#21520 = ORIENTED_EDGE ( 'NONE', *, *, #30040, .F. ) ;
#21521 = CARTESIAN_POINT ( 'NONE',  ( 115.9729548109119861, -6.344957434206662583, -7.627207830600332805 ) ) ;
#21522 = CARTESIAN_POINT ( 'NONE',  ( 92.04708369096698561, -26.60966817898065884, -11.90521360603286816 ) ) ;
#21523 = CARTESIAN_POINT ( 'NONE',  ( 112.4272546295247821, -4.863998795839590272, -7.631215200338315796 ) ) ;
#21524 = CARTESIAN_POINT ( 'NONE',  ( 126.3539348109119800, -4.153390946401325223, -8.397313243818185668 ) ) ;
#21525 = CARTESIAN_POINT ( 'NONE',  ( 112.4559014775786494, -9.988377603198976828, -10.36322818467138340 ) ) ;
#21526 = CARTESIAN_POINT ( 'NONE',  ( 128.2184548109119930, -10.81584935473217080, -14.15181583611863303 ) ) ;
#21527 = CARTESIAN_POINT ( 'NONE',  ( 0.04488520489200759078, -6.166763362545027327, -19.39321520033831447 ) ) ;
#21528 = CARTESIAN_POINT ( 'NONE',  ( 110.0658483795247804, -8.402594152722688392, -16.93181055722141792 ) ) ;
#21529 = VERTEX_POINT ( 'NONE', #44225 ) ;
#21530 = CARTESIAN_POINT ( 'NONE',  ( 121.7663437114597258, -6.208002839291213881, -18.65814938918611077 ) ) ;
#21531 = CARTESIAN_POINT ( 'NONE',  ( 109.2295669185610194, -6.591008720997902692, -18.37361123771471227 ) ) ;
#21532 = CARTESIAN_POINT ( 'NONE',  ( 115.1220548109119761, -1.833838273342658809, -17.42832698103878286 ) ) ;
#21533 = CARTESIAN_POINT ( 'NONE',  ( 64.80575110624921820, -13.22907879418145249, -11.52632176784967655 ) ) ;
#21534 = CIRCLE ( 'NONE', #22282, 2.000000000000000444 ) ;
#21535 = CARTESIAN_POINT ( 'NONE',  ( 116.8722546295247895, -4.863998795839590272, -18.39754474579285315 ) ) ;
#21536 = CARTESIAN_POINT ( 'NONE',  ( 107.3571765045248299, -7.250697342233347165, -19.15521520033831138 ) ) ;
#21537 = LINE ( 'NONE', #24516, #33443 ) ;
#21538 = CARTESIAN_POINT ( 'NONE',  ( 114.3278814775786429, 0.1319031606808879209, -14.10382304977623669 ) ) ;
#21539 = DIRECTION ( 'NONE',  ( 0.000000000000000000, 0.4669533266896289669, 0.8842819633428516957 ) ) ;
#21540 = CARTESIAN_POINT ( 'NONE',  ( 124.6521348109119884, -1.561330072975668948, -17.79121239304076951 ) ) ;
#21541 = CARTESIAN_POINT ( 'NONE',  ( 114.9518748109119883, -1.834011780172310813, -8.268836392978581529 ) ) ;
#21542 = VERTEX_POINT ( 'NONE', #36452 ) ;
#21543 = CARTESIAN_POINT ( 'NONE',  ( 116.1998614775786507, 0.4262465694468514643, -12.03445270309931736 ) ) ;
#21544 = LINE ( 'NONE', #7630, #26183 ) ;
#21545 = CARTESIAN_POINT ( 'NONE',  ( 116.4834948109119779, -1.561330072975668504, -17.79121239304076951 ) ) ;
#21546 = CARTESIAN_POINT ( 'NONE',  ( 115.6893214775786447, -9.859900752359374465, -12.68260735090039404 ) ) ;
#21547 = ORIENTED_EDGE ( 'NONE', *, *, #36066, .F. ) ;
#21548 = CARTESIAN_POINT ( 'NONE',  ( 121.5888948109119809, 0.1319031606808879209, -14.10382304977623669 ) ) ;
#21549 = AXIS2_PLACEMENT_3D ( 'NONE', #11026, #24926, #3718 ) ;
#21550 = CARTESIAN_POINT ( 'NONE',  ( 116.8238548109119819, -4.089484607189486809, -7.948022111789456723 ) ) ;
#21551 = CIRCLE ( 'NONE', #29563, 10.00000000000000000 ) ;
#21552 = CARTESIAN_POINT ( 'NONE',  ( 136.0647682600814221, 0.5678772681889172613, -15.70378451066936698 ) ) ;
#21553 = CARTESIAN_POINT ( 'NONE',  ( 111.1770983795247787, -0.7896495226426338832, -9.318865927141430916 ) ) ;
#21554 = CYLINDRICAL_SURFACE ( 'NONE', #41025, 1.999999999999998890 ) ;
#21555 = CYLINDRICAL_SURFACE ( 'NONE', #28848, 1.999999999999998890 ) ;
#21556 = CARTESIAN_POINT ( 'NONE',  ( 113.6079577545248043, -2.791137627527939813, -18.39754474579286025 ) ) ;
#21557 = CARTESIAN_POINT ( 'NONE',  ( 115.3489614775786407, -9.261995988541697145, -16.69588392320189030 ) ) ;
#21558 = EDGE_CURVE ( 'NONE', #2441, #17646, #2246, .T. ) ;
#21559 = VECTOR ( 'NONE', #40901, 1000.000000000000000 ) ;
#21560 = CARTESIAN_POINT ( 'NONE',  ( 88.73939138327467901, -26.60966817898065884, -11.90521360603286816 ) ) ;
#21561 = CARTESIAN_POINT ( 'NONE',  ( 115.9729548109119861, -3.505236298600246325, -18.68346056562440793 ) ) ;
#21562 = CARTESIAN_POINT ( 'NONE',  ( 60.83824608292380987, -12.51476863122120520, -17.26777189981386229 ) ) ;
#21563 = CARTESIAN_POINT ( 'NONE',  ( 116.9582927111058552, -1.267766418764730840, -16.93314635290706605 ) ) ;
#21564 = CARTESIAN_POINT ( 'NONE',  ( 116.7333483795247844, -8.402594152722688392, -16.93181055722141792 ) ) ;
#21565 = CARTESIAN_POINT ( 'NONE',  ( 113.7606148109119886, -7.894159318335828068, -9.358103419637847864 ) ) ;
#21566 = CARTESIAN_POINT ( 'NONE',  ( 123.4244704359119709, -10.25716656981731489, -12.88942061488890545 ) ) ;
#21567 = AXIS2_PLACEMENT_3D ( 'NONE', #17975, #18201, #31650 ) ;
#21568 = CARTESIAN_POINT ( 'NONE',  ( 87.80477198183443477, -27.84333996136784961, -14.15691383771150136 ) ) ;
#21570 = CARTESIAN_POINT ( 'NONE',  ( 119.9438214775786378, -7.893985811506177619, -18.51759400769804742 ) ) ;
#21569 = CARTESIAN_POINT ( 'NONE',  ( 64.51132457273422460, -13.77492255257581277, -8.859678336860978831 ) ) ;
#21571 = CARTESIAN_POINT ( 'NONE',  ( 118.0718414775786442, -0.8288870151387760510, -10.36305467784173118 ) ) ;
#21572 = CARTESIAN_POINT ( 'NONE',  ( 125.1626748109119802, -9.988377603198980381, -10.36322818467138518 ) ) ;
#21573 = ORIENTED_EDGE ( 'NONE', *, *, #39829, .T. ) ;
#21574 = DIRECTION ( 'NONE',  ( -0.8636456077245086016, 0.5040994586965593660, 0.000000000000000000 ) ) ;
#21575 = CARTESIAN_POINT ( 'NONE',  ( 123.5743281442453139, -7.893985811506177619, -18.51759400769804742 ) ) ;
#21576 = CARTESIAN_POINT ( 'NONE',  ( 112.7050671295247923, 0.1403307496149613920, -13.39321520033831447 ) ) ;
#21577 = CARTESIAN_POINT ( 'NONE',  ( 119.7169148109119874, -0.1624402480850797581, -16.17319339645315424 ) ) ;
#21578 = AXIS2_PLACEMENT_3D ( 'NONE', #12316, #26444, #29632 ) ;
#21579 = CARTESIAN_POINT ( 'NONE',  ( 116.4834948109119779, -7.894159318335828068, -9.358103419637847864 ) ) ;
#21580 = CARTESIAN_POINT ( 'NONE',  ( -3.429934629567074733, -4.841764211284793618, -7.393215200338315363 ) ) ;
#21581 = CARTESIAN_POINT ( 'NONE',  ( 113.1912390045248031, 0.8980012041604421569, -15.77991374673208469 ) ) ;
#21582 = CARTESIAN_POINT ( 'NONE',  ( 121.5321681442453183, -0.1624402480850797581, -16.17319339645315424 ) ) ;
#21583 = CARTESIAN_POINT ( 'NONE',  ( 124.9924948109119924, -5.574606645277164318, -18.38911715685844683 ) ) ;
#21584 = CARTESIAN_POINT ( 'NONE',  ( 116.8689514802850198, -3.929494816604741203, -18.62311481910882804 ) ) ;
#21585 = CARTESIAN_POINT ( 'NONE',  ( 109.2295156139914383, -1.481211192124197051, -9.165827887151388964 ) ) ;
#21586 = CARTESIAN_POINT ( 'NONE',  ( 120.4379860609119675, -3.387241619883791355, -18.17469012370385073 ) ) ;
#21587 = CARTESIAN_POINT ( 'NONE',  ( 114.0941296295247867, -4.863998795839590272, -19.15521520033831493 ) ) ;
#21588 = SHAPE_REPRESENTATION ( 'Barrel Adjuster Screw', ( #12375 ), #14045 ) ;
#21589 = CYLINDRICAL_SURFACE ( 'NONE', #16041, 2.000000000000001776 ) ;
#21590 = CARTESIAN_POINT ( 'NONE',  ( 116.9373081442452929, -8.166667518702817929, -8.995218007635861213 ) ) ;
#21591 = CARTESIAN_POINT ( 'NONE',  ( 113.1933481442453058, -4.089484607189486809, -7.948022111789456723 ) ) ;
#21592 = CARTESIAN_POINT ( 'NONE',  ( 111.1076452545248259, 0.8980012041604421569, -11.00651665394454071 ) ) ;
#21593 = CARTESIAN_POINT ( 'NONE',  ( 114.6115148109119986, -3.383040157471821630, -19.15922257007629170 ) ) ;
#21594 = ORIENTED_EDGE ( 'NONE', *, *, #40451, .F. ) ;
#21595 = CARTESIAN_POINT ( 'NONE',  ( 88.22708560785949317, -3.622631779710408395, -9.893215200338316251 ) ) ;
#21596 = CARTESIAN_POINT ( 'NONE',  ( 124.4819548109119722, -7.893985811506177619, -18.51759400769804742 ) ) ;
#21597 = CARTESIAN_POINT ( 'NONE',  ( 115.4056881442453459, -7.893985811506177619, -18.51759400769804742 ) ) ;
#21598 = CARTESIAN_POINT ( 'NONE',  ( 120.7947214775786193, -0.8288870151387760510, -10.36305467784173118 ) ) ;
#21599 = APPLICATION_PROTOCOL_DEFINITION ( 'draft international standard', 'automotive_design', 1998, #35525 ) ;
#21600 = CARTESIAN_POINT ( 'NONE',  ( 125.2194014775786286, -10.30919188438810075, -12.61870101168855918 ) ) ;
#21601 = CARTESIAN_POINT ( 'NONE',  ( 122.8368814775786291, -1.561330072975668948, -17.79121239304076951 ) ) ;
#21602 = AXIS2_PLACEMENT_3D ( 'NONE', #21807, #14747, #22034 ) ;
#21603 = CARTESIAN_POINT ( 'NONE',  ( 114.7886608795247696, -8.938348069036489818, -9.318865927141430916 ) ) ;
#21604 = CARTESIAN_POINT ( 'NONE',  ( 117.2776681442452968, -4.153390946401325223, -8.397313243818185668 ) ) ;
#21605 = CARTESIAN_POINT ( 'NONE',  ( 122.5910329359119970, -4.283928203966213211, -7.183505701512925334 ) ) ;
#21606 = CARTESIAN_POINT ( 'NONE',  ( 67.30914723170953096, -53.23718887596189120, -35.39220701967414584 ) ) ;
#21607 = ORIENTED_EDGE ( 'NONE', *, *, #42473, .T. ) ;
#21608 = CARTESIAN_POINT ( 'NONE',  ( 121.7590748109119687, -7.893985811506177619, -18.51759400769804742 ) ) ;
#21609 = VECTOR ( 'NONE', #44234, 1000.000000000000000 ) ;
#21610 = CARTESIAN_POINT ( 'NONE',  ( 121.8965016859119856, -9.665098340737509730, -17.37397104707595474 ) ) ;
#21611 = CARTESIAN_POINT ( 'NONE',  ( 119.8303681442453126, -10.63000616557722466, -14.87417383870573495 ) ) ;
#21612 = ORIENTED_EDGE ( 'NONE', *, *, #12672, .F. ) ;
#21613 = CARTESIAN_POINT ( 'NONE',  ( 106.6626452545248611, -9.868328341294098749, -15.46607636864997204 ) ) ;
#21614 = CARTESIAN_POINT ( 'NONE',  ( -13.55413964183373743, -3.899881072927508185, -8.039791994638363803 ) ) ;
#21615 = CARTESIAN_POINT ( 'NONE',  ( 117.3911214775786505, -7.894159318335828068, -9.358103419637847864 ) ) ;
#21616 = CARTESIAN_POINT ( 'NONE',  ( 66.21962885992722647, -37.11159810974177731, -4.893215200338314474 ) ) ;
#21617 = CARTESIAN_POINT ( 'NONE',  ( 64.85649322025210495, -35.54674243456235416, -5.785566283887345840 ) ) ;
#21618 = CARTESIAN_POINT ( 'NONE',  ( 118.9794681442453026, -0.8288870151387760510, -10.36305467784173118 ) ) ;
#21619 = DIRECTION ( 'NONE',  ( -0.9908103287288504424, 0.1352586133457950590, 0.000000000000000000 ) ) ;
#21620 = CARTESIAN_POINT ( 'NONE',  ( 122.8368814775786291, -7.894159318335828068, -9.358103419637847864 ) ) ;
#21621 = DIRECTION ( 'NONE',  ( 1.000000000000000000, 0.000000000000000000, -0.000000000000000000 ) ) ;
#21622 = CIRCLE ( 'NONE', #37676, 2.999999999999999556 ) ;
#21623 = CARTESIAN_POINT ( 'NONE',  ( 119.6601881442453106, -1.833838273342659253, -17.42832698103878286 ) ) ;
#21624 = CARTESIAN_POINT ( 'NONE',  ( 114.4413348109119823, -9.261995988541697145, -16.69588392320189030 ) ) ;
#21625 = CARTESIAN_POINT ( 'NONE',  ( 118.4122014775786340, 0.5811942927096110934, -14.16772938898807510 ) ) ;
#21626 = CARTESIAN_POINT ( 'NONE',  ( 126.2404814775786264, -0.8288870151387760510, -10.36305467784173118 ) ) ;
#21627 = CARTESIAN_POINT ( 'NONE',  ( 126.2184548109105435, -4.159894987975746972, -8.443039665293909479 ) ) ;
#21628 = CARTESIAN_POINT ( 'NONE',  ( 121.9859814775786333, -9.565557343593413364, -10.61323700422348004 ) ) ;
#21629 = ORIENTED_EDGE ( 'NONE', *, *, #20658, .T. ) ;
#21630 = CARTESIAN_POINT ( 'NONE',  ( 121.0783548109119749, 0.2603800115204892296, -16.42320221600525088 ) ) ;
#21631 = CARTESIAN_POINT ( 'NONE',  ( 111.8021765045248372, -2.791137627527939813, -8.388885654883777576 ) ) ;
#21632 = AXIS2_PLACEMENT_3D ( 'NONE', #5406, #1982, #15909 ) ;
#21633 = CARTESIAN_POINT ( 'NONE',  ( 115.1904114748722492, -0.1020945015694959546, -15.74893487844866691 ) ) ;
#21634 = CARTESIAN_POINT ( 'NONE',  ( 114.3024890045248156, -9.868328341294150263, -11.32035403202669777 ) ) ;
#21635 = CARTESIAN_POINT ( 'NONE',  ( 123.5880035264548837, -8.247323210606174015, -17.08054893949881858 ) ) ;
#21636 = CARTESIAN_POINT ( 'NONE',  ( 125.9001214775786224, -4.089484607189486809, -7.948022111789456723 ) ) ;
#21637 = ORIENTED_EDGE ( 'NONE', *, *, #27287, .T. ) ;
#21638 = FACE_OUTER_BOUND ( 'NONE', #42147, .T. ) ;
#21639 = CARTESIAN_POINT ( 'NONE',  ( 123.0070614775786169, -10.15424416112533912, -14.75197769757731336 ) ) ;
#21640 = CARTESIAN_POINT ( 'NONE',  ( 61.95510581920947146, -14.46403044595587595, -19.00299887994344061 ) ) ;
#21641 = CARTESIAN_POINT ( 'NONE',  ( 126.0703014775786102, -9.988377603198980381, -10.36322818467138518 ) ) ;
#21642 = CARTESIAN_POINT ( 'NONE',  ( 110.3436608795247764, -1.325403438956436419, -16.93181055722141792 ) ) ;
#21643 = VERTEX_POINT ( 'NONE', #33932 ) ;
#21644 = CARTESIAN_POINT ( 'NONE',  ( 113.9307948109119906, 0.9020085738987339008, -11.91225656197089222 ) ) ;
#21645 = CARTESIAN_POINT ( 'NONE',  ( 113.0231681442453322, 0.9020085738987339008, -11.91225656197089222 ) ) ;
#21646 = CARTESIAN_POINT ( 'NONE',  ( 125.9568481442452850, -6.344957434206665248, -7.627207830600338134 ) ) ;
#21647 = CARTESIAN_POINT ( 'NONE',  ( 122.2696148109119889, -5.574606645277164318, -18.38911715685844683 ) ) ;
#21648 = CARTESIAN_POINT ( 'NONE',  ( 112.3991748109119868, -1.833838273342658809, -17.42832698103878286 ) ) ;
#21649 = DIRECTION ( 'NONE',  ( 0.000000000000000000, 0.000000000000000000, 1.000000000000000000 ) ) ;
#21650 = CARTESIAN_POINT ( 'NONE',  ( 123.4608748109119745, -10.63000616557722466, -14.87417383870573495 ) ) ;
#21651 = CARTESIAN_POINT ( 'NONE',  ( 111.4453614775786434, -1.861572684145083256, -17.39139446643145348 ) ) ;
#21652 = CARTESIAN_POINT ( 'NONE',  ( 78.69189222814998175, -50.16718729050182191, -6.893215200338315363 ) ) ;
#21653 = CARTESIAN_POINT ( 'NONE',  ( 110.1099666496844804, 0.5600166689815611054, -12.14321520033828428 ) ) ;
#21654 = CARTESIAN_POINT ( 'NONE',  ( 125.4463081442452932, -4.153390946401325223, -8.397313243818185668 ) ) ;
#21655 = ORIENTED_EDGE ( 'NONE', *, *, #21715, .T. ) ;
#21656 = EDGE_CURVE ( 'NONE', #31533, #23066, #12532, .T. ) ;
#21657 = MANIFOLD_SOLID_BREP ( 'NONE', #3933 ) ;
#21658 = CARTESIAN_POINT ( 'NONE',  ( 114.1635827545248389, -6.936859964151250502, -8.388885654883777576 ) ) ;
#21659 = CIRCLE ( 'NONE', #32581, 1.610000000000000986 ) ;
#21660 = CARTESIAN_POINT ( 'NONE',  ( 120.3976348109119812, -1.834011780172310813, -8.268836392978581529 ) ) ;
#21661 = CARTESIAN_POINT ( 'NONE',  ( 136.7860375664299966, -8.463374175688866075, -17.68495210800635675 ) ) ;
#21662 = ORIENTED_EDGE ( 'NONE', *, *, #15178, .T. ) ;
#21663 = CARTESIAN_POINT ( 'NONE',  ( 121.1589942721482771, -2.287189184988711155, -18.07361239780447448 ) ) ;
#21664 = CARTESIAN_POINT ( 'NONE',  ( 125.6164881442453094, 0.2603800115204892296, -16.42320221600525088 ) ) ;
#21665 = DIRECTION ( 'NONE',  ( -0.000000000000000000, -0.000000000000000000, 1.000000000000000000 ) ) ;
#21666 = CARTESIAN_POINT ( 'NONE',  ( 124.2550481442452792, -0.1624402480850797581, -16.17319339645315424 ) ) ;
#21667 = ORIENTED_EDGE ( 'NONE', *, *, #23077, .T. ) ;
#21668 = CARTESIAN_POINT ( 'NONE',  ( 119.1496481442453046, -3.383040157471821630, -19.15922257007629170 ) ) ;
#21669 = DIRECTION ( 'NONE',  ( 0.000000000000000000, 0.000000000000000000, 1.000000000000000000 ) ) ;
#21670 = CARTESIAN_POINT ( 'NONE',  ( 77.05532149770296257, 0.06670422450934243574, -18.64321520033831803 ) ) ;
#21671 = AXIS2_PLACEMENT_3D ( 'NONE', #11538, #12440, #19276 ) ;
#21672 = CARTESIAN_POINT ( 'NONE',  ( 136.0617147589328226, -5.568559906631047163, -7.532066164982730960 ) ) ;
#21673 = CARTESIAN_POINT ( 'NONE',  ( 125.9568481442452850, -6.344957434206665248, -7.627207830600338134 ) ) ;
#21674 = EDGE_CURVE ( 'NONE', #30998, #31663, #16630, .T. ) ;
#21675 = FACE_OUTER_BOUND ( 'NONE', #1647, .T. ) ;
#21676 = LINE ( 'NONE', #21229, #36109 ) ;
#21677 = CARTESIAN_POINT ( 'NONE',  ( 124.9357681442453014, -1.834011780172310813, -8.268836392978581529 ) ) ;
#21679 = CARTESIAN_POINT ( 'NONE',  ( 124.8223148109119762, -10.15424416112533912, -14.75197769757731336 ) ) ;
#21678 = CARTESIAN_POINT ( 'NONE',  ( 123.6310548109119765, -5.638512984488999180, -18.83840828888717311 ) ) ;
#21680 = FACE_OUTER_BOUND ( 'NONE', #10375, .T. ) ;
#21681 = CARTESIAN_POINT ( 'NONE',  ( 124.0848681442452772, -5.574606645277164318, -18.38911715685844683 ) ) ;
#21682 = CARTESIAN_POINT ( 'NONE',  ( 113.1933481442453058, -5.574606645277164318, -18.38911715685844683 ) ) ;
#21683 = CARTESIAN_POINT ( 'NONE',  ( 121.1350814775786233, 0.5811942927096110934, -14.16772938898807510 ) ) ;
#21684 = ADVANCED_FACE ( 'NONE', ( #36897 ), #24307, .T. ) ;
#21685 = EDGE_LOOP ( 'NONE', ( #29023, #21732, #17845, #8634, #14148, #40843 ) ) ;
#21686 = ORIENTED_EDGE ( 'NONE', *, *, #5520, .F. ) ;
#21687 = CARTESIAN_POINT ( 'NONE',  ( 122.5584604873411791, -2.348512537728041583, -17.99195118506215962 ) ) ;
#21688 = ADVANCED_FACE ( 'NONE', ( #44446 ), #40339, .T. ) ;
#21689 = CARTESIAN_POINT ( 'NONE',  ( 115.1359265045248605, -7.250697342233347165, -19.15521520033831138 ) ) ;
#21690 = CARTESIAN_POINT ( 'NONE',  ( 105.8986608795248401, -8.938348069036489818, -9.318865927141430916 ) ) ;
#21691 = CARTESIAN_POINT ( 'NONE',  ( 114.1635827545248389, -6.936859964151250502, -8.388885654883777576 ) ) ;
#21692 = VECTOR ( 'NONE', #25895, 1000.000000000000000 ) ;
#21693 = CARTESIAN_POINT ( 'NONE',  ( 86.36631847702263087, -25.99489077589524300, -13.39321520033831447 ) ) ;
#21694 = CARTESIAN_POINT ( 'NONE',  ( 112.3991748109119868, -8.166667518702817929, -8.995218007635859436 ) ) ;
#21695 = EDGE_LOOP ( 'NONE', ( #29239, #42967, #43508, #8259, #11467 ) ) ;
#21696 = CARTESIAN_POINT ( 'NONE',  ( 113.9875214775786532, -8.899110576539710493, -16.42337572283490132 ) ) ;
#21697 = CARTESIAN_POINT ( 'NONE',  ( 106.1070202545248407, -10.62599879583958717, -15.77991374673208469 ) ) ;
#21698 = DIRECTION ( 'NONE',  ( 0.000000000000000000, 0.000000000000000000, 1.000000000000000000 ) ) ;
#21699 = CARTESIAN_POINT ( 'NONE',  ( 90.93679655599923706, -18.80572346544368756, -6.893215200338315363 ) ) ;
#21700 = CARTESIAN_POINT ( 'NONE',  ( 109.2294759059926008, -0.3400322672942256985, -15.71119955778137545 ) ) ;
#21701 = CARTESIAN_POINT ( 'NONE',  ( 85.94012291206631460, -8.967540239925705592, -14.14321520033831625 ) ) ;
#21702 = CARTESIAN_POINT ( 'NONE',  ( 114.5547881442453217, -5.638512984488999180, -18.83840828888717311 ) ) ;
#21703 = ADVANCED_FACE ( 'NONE', ( #23238 ), #14832, .T. ) ;
#21704 = CARTESIAN_POINT ( 'NONE',  ( 112.9828796295247884, -4.863998795839590272, -19.15521520033831493 ) ) ;
#21705 = CARTESIAN_POINT ( 'NONE',  ( 109.6491296295247793, -4.863998795839590272, -8.388885654883775800 ) ) ;
#21706 = ORIENTED_EDGE ( 'NONE', *, *, #20892, .T. ) ;
#21707 = CARTESIAN_POINT ( 'NONE',  ( 67.84197459855160162, -50.86926263129819148, -34.27970990073318802 ) ) ;
#21708 = CARTESIAN_POINT ( 'NONE',  ( 114.6115148109119986, -6.222761293078241884, -8.102969835052219238 ) ) ;
#21709 = CARTESIAN_POINT ( 'NONE',  ( 117.4478481442453131, 0.2603800115204892296, -16.42320221600525088 ) ) ;
#21710 = DIRECTION ( 'NONE',  ( 0.000000000000000000, 0.3713878862591638574, -0.9284778069183724503 ) ) ;
#21711 = EDGE_CURVE ( 'NONE', #5648, #15833, #34474, .T. ) ;
#21712 = CARTESIAN_POINT ( 'NONE',  ( 119.3198281442452924, -9.859900752359374465, -12.68260735090039404 ) ) ;
#21713 = CARTESIAN_POINT ( 'NONE',  ( 114.2711548109119803, -0.1624402480850797581, -16.17319339645315424 ) ) ;
#21714 = ORIENTED_EDGE ( 'NONE', *, *, #10964, .T. ) ;
#21715 = EDGE_CURVE ( 'NONE', #14979, #41111, #40800, .T. ) ;
#21716 = EDGE_CURVE ( 'NONE', #22284, #20119, #2475, .T. ) ;
#21717 = CARTESIAN_POINT ( 'NONE',  ( 123.2161110609119703, -6.340755971794695078, -8.611740276972781771 ) ) ;
#21718 = DIRECTION ( 'NONE',  ( 0.000000000000000000, 0.6004852223388321697, -0.7996358532186279566 ) ) ;
#21719 = CARTESIAN_POINT ( 'NONE',  ( 118.9794681442453026, -0.8288870151387760510, -10.36305467784173118 ) ) ;
#21720 = EDGE_LOOP ( 'NONE', ( #45018, #16611 ) ) ;
#21721 = CARTESIAN_POINT ( 'NONE',  ( 65.41257106814472877, -15.47412461924279725, -10.39321520033831625 ) ) ;
#21722 = CARTESIAN_POINT ( 'NONE',  ( 116.8238548109119819, -4.089484607189486809, -7.948022111789456723 ) ) ;
#21723 = CARTESIAN_POINT ( 'NONE',  ( 114.9275671295247889, -10.62599879583958540, -13.39321520033831447 ) ) ;
#21724 = LINE ( 'NONE', #35611, #38985 ) ;
#21725 = ORIENTED_EDGE ( 'NONE', *, *, #10952, .F. ) ;
#21726 = ORIENTED_EDGE ( 'NONE', *, *, #14445, .F. ) ;
#21727 = CARTESIAN_POINT ( 'NONE',  ( 117.6180281442453150, -8.899110576539710493, -16.42337572283490132 ) ) ;
#21728 = B_SPLINE_CURVE_WITH_KNOTS ( 'NONE', 3,
 ( #13136, #34530, #9944, #45047 ),
 .UNSPECIFIED., .F., .F.,
 ( 4, 4 ),
 ( 0.000000000000000000, 1.000000000000000000 ),
 .UNSPECIFIED. ) ;
#21729 = CARTESIAN_POINT ( 'NONE',  ( 119.0929214775786278, -4.153390946401325223, -8.397313243818185668 ) ) ;
#21730 = CARTESIAN_POINT ( 'NONE',  ( 124.5402294140156698, -9.847276183098475855, -12.97714367041513839 ) ) ;
#21731 = CARTESIAN_POINT ( 'NONE',  ( 122.4521266859119635, -0.06289925094097943703, -9.412459353600674206 ) ) ;
#21732 = ORIENTED_EDGE ( 'NONE', *, *, #38095, .T. ) ;
#21733 = DIRECTION ( 'NONE',  ( -0.9659258262890687563, -0.2588190451025194627, 0.000000000000000000 ) ) ;
#21734 = CARTESIAN_POINT ( 'NONE',  ( 69.69189222815028018, -41.76310523276638520, -19.39321520033831447 ) ) ;
#21735 = CARTESIAN_POINT ( 'NONE',  ( 108.9545983795247821, -0.7896495226426338832, -9.318865927141430916 ) ) ;
#21736 = CARTESIAN_POINT ( 'NONE',  ( 113.5337081442453240, -9.261995988541697145, -16.69588392320189030 ) ) ;
#21737 = CARTESIAN_POINT ( 'NONE',  ( 112.7962614775786676, -3.383040157471821630, -19.15922257007629170 ) ) ;
#21738 = CARTESIAN_POINT ( 'NONE',  ( 117.5613014775786525, -10.15424416112533912, -14.75197769757731336 ) ) ;
#21739 = DIRECTION ( 'NONE',  ( 0.000000000000000000, 0.6004852223388321697, -0.7996358532186279566 ) ) ;
#21740 = VERTEX_POINT ( 'NONE', #26205 ) ;
#21741 = CARTESIAN_POINT ( 'NONE',  ( 114.9518748109119883, -7.643976991954077427, -18.09477374809248928 ) ) ;
#21742 = DIRECTION ( 'NONE',  ( 0.000000000000000000, -0.8069730661766900681, 0.5905882410490337353 ) ) ;
#21743 = CARTESIAN_POINT ( 'NONE',  ( 84.55230152525003007, -29.88260722510756651, -11.30949563633199162 ) ) ;
#21744 = CARTESIAN_POINT ( 'NONE',  ( 115.4137390045248566, 0.8980012041604421569, -15.77991374673208469 ) ) ;
#21745 = CARTESIAN_POINT ( 'NONE',  ( 116.4834948109119779, -1.561330072975668504, -17.79121239304076951 ) ) ;
#21746 = EDGE_LOOP ( 'NONE', ( #26683, #35881, #28954, #31471, #3628 ) ) ;
#21747 = CARTESIAN_POINT ( 'NONE',  ( 117.6180281442453150, -0.4660016031367893996, -10.09054647747474043 ) ) ;
#21748 = LINE ( 'NONE', #28366, #658 ) ;
#21749 = CARTESIAN_POINT ( 'NONE',  ( 113.9552233795247815, -8.938348069036489818, -17.46756447353520159 ) ) ;
#21750 = CARTESIAN_POINT ( 'NONE',  ( 115.3489614775786407, -9.261995988541697145, -16.69588392320189030 ) ) ;
#21751 = CARTESIAN_POINT ( 'NONE',  ( 114.8384214775786489, 0.9020085738987339008, -11.91225656197089222 ) ) ;
#21752 = CARTESIAN_POINT ( 'NONE',  ( 85.15861813568058380, -25.23119213852205789, -15.24166438581092109 ) ) ;
#21753 = LINE ( 'NONE', #31558, #5307 ) ;
#21754 = CARTESIAN_POINT ( 'NONE',  ( 106.9404577545248145, -2.791137627527939813, -18.39754474579286025 ) ) ;
#21755 = EDGE_CURVE ( 'NONE', #44682, #25810, #43210, .T. ) ;
#21756 = VERTEX_POINT ( 'NONE', #9556 ) ;
#21757 = CARTESIAN_POINT ( 'NONE',  ( 121.4551560953690483, -6.001247023715324147, -18.26661038929047010 ) ) ;
#21758 = CARTESIAN_POINT ( 'NONE',  ( 109.2295854867894320, -5.018741757313862628, -18.58799787790541558 ) ) ;
#21759 = CARTESIAN_POINT ( 'NONE',  ( 116.1998614775786507, 0.4262465694468514643, -12.03445270309931736 ) ) ;
#21760 = CARTESIAN_POINT ( 'NONE',  ( 63.53803937314328465, -12.73310566472691185, -10.53259732128069537 ) ) ;
#21761 = CARTESIAN_POINT ( 'NONE',  ( 118.2313338145250441, -3.807985514183284348, -19.09877912889400520 ) ) ;
#21762 = CARTESIAN_POINT ( 'NONE',  ( 114.3719421295247827, -9.868328341294093420, -13.39321520033831447 ) ) ;
#21763 = CARTESIAN_POINT ( 'NONE',  ( 126.5125895482226639, -4.782699052591321554, -8.246788084914983941 ) ) ;
#21764 = CARTESIAN_POINT ( 'NONE',  ( 115.1220548109119761, -1.833838273342658809, -17.42832698103878286 ) ) ;
#21765 = CARTESIAN_POINT ( 'NONE',  ( 121.9470836909669913, -27.84333996136784961, -14.15691383771150136 ) ) ;
#21766 = CARTESIAN_POINT ( 'NONE',  ( 124.8223148109119762, 0.9020085738987339008, -11.91225656197089222 ) ) ;
#21767 = CARTESIAN_POINT ( 'NONE',  ( 120.2841814775786276, 0.9020085738987339008, -11.91225656197089222 ) ) ;
#21768 = EDGE_LOOP ( 'NONE', ( #33638, #42476, #42442, #10226, #9090, #7840, #29166 ) ) ;
#21769 = ADVANCED_FACE ( 'NONE', ( #22774 ), #32998, .T. ) ;
#21770 = CARTESIAN_POINT ( 'NONE',  ( 118.9227414775786542, 0.4262465694468514643, -12.03445270309931736 ) ) ;
#21771 = CARTESIAN_POINT ( 'NONE',  ( 112.9097148109120070, 0.2603800115204892296, -16.42320221600525088 ) ) ;
#21772 = ADVANCED_FACE ( 'NONE', ( #23004 ), #19585, .T. ) ;
#21773 = CARTESIAN_POINT ( 'NONE',  ( 118.6958348109119754, -6.344957434206665248, -7.627207830600338134 ) ) ;
#21774 = CARTESIAN_POINT ( 'NONE',  ( 118.2420214775786320, -6.222761293078241884, -8.102969835052219238 ) ) ;
#21775 = ORIENTED_EDGE ( 'NONE', *, *, #27880, .F. ) ;
#21776 = ADVANCED_FACE ( 'NONE', ( #24583, #27566 ), #6584, .T. ) ;
#21777 = CARTESIAN_POINT ( 'NONE',  ( 123.0070614775786169, -10.15424416112533912, -14.75197769757731336 ) ) ;
#21778 =( BOUNDED_CURVE ( )  B_SPLINE_CURVE ( 2, ( #13200, #27330, #40785, #9543, #27100, #10006, #9776, #23915, #23690, #20490, #34369, #17072, #27774, #34588, #3372, #17291, #31184 ),
 .UNSPECIFIED., .F., .F. ) 
 B_SPLINE_CURVE_WITH_KNOTS ( ( 3, 2, 2, 2, 2, 2, 2, 2, 3 ),
 ( 0.2035091206787220108, 0.2124999999999999944, 0.2250000000000000056, 0.2374999999999999889, 0.2500000000000000000, 0.2625000000000000111, 0.2750000000000000222, 0.2874999999999999778, 0.2964908793212779892 ),
 .UNSPECIFIED. ) 
 CURVE ( )  GEOMETRIC_REPRESENTATION_ITEM ( )  RATIONAL_B_SPLINE_CURVE ( ( 0.9692594319298230010, 0.9452488050343769155, 1.000000000000000000, 0.9238795325112869605, 1.000000000000000000, 0.9238795325112869605, 1.000000000000000000, 0.9238795325112869605, 1.000000000000000000, 0.9238795325112869605, 1.000000000000000000, 0.9238795325112869605, 1.000000000000000000, 0.9238795325112869605, 1.000000000000000000, 0.9452488050343769155, 0.9692594319298220018 ) ) 
 REPRESENTATION_ITEM ( '' )  );
#21779 = CARTESIAN_POINT ( 'NONE',  ( 120.9081748109119872, -5.638512984488999180, -18.83840828888717311 ) ) ;
#21780 = CARTESIAN_POINT ( 'NONE',  ( 135.7500233008185830, 0.6216732964927550453, -15.76311964996550685 ) ) ;
#21781 = CARTESIAN_POINT ( 'NONE',  ( 110.6214733795247867, -8.938348069036489818, -17.46756447353520159 ) ) ;
#21782 = CARTESIAN_POINT ( 'NONE',  ( 114.3801926359456331, -1.179503403430479658, -17.05068175419387799 ) ) ;
#21783 = CARTESIAN_POINT ( 'NONE',  ( 126.6479178317288188, 0.3508773515938530818, -13.34825603011022466 ) ) ;
#21784 = CARTESIAN_POINT ( 'NONE',  ( 114.3719421295247827, -9.868328341294093420, -13.39321520033831447 ) ) ;
#21785 = CARTESIAN_POINT ( 'NONE',  ( 118.9227414775786400, -10.63000616557722466, -14.87417383870573495 ) ) ;
#21786 = CARTESIAN_POINT ( 'NONE',  ( -13.56828337869051104, -4.779084862086333985, -17.89321520033831447 ) ) ;
#21787 = CARTESIAN_POINT ( 'NONE',  ( 114.9518748109119883, -7.643976991954077427, -18.09477374809248928 ) ) ;
#21788 = CARTESIAN_POINT ( 'NONE',  ( 64.17925045615415058, -12.94885914896418377, -15.80747231013753940 ) ) ;
#21789 = CARTESIAN_POINT ( 'NONE',  ( -12.55610316477683241, -4.307149106694457608, -7.393215200338315363 ) ) ;
#21790 = CARTESIAN_POINT ( 'NONE',  ( 110.2047546295247855, -4.863998795839590272, -18.39754474579285315 ) ) ;
#21791 = DIRECTION ( 'NONE',  ( 0.000000000000000000, -0.9242245927363028635, -0.3818493186865927758 ) ) ;
#21792 = CARTESIAN_POINT ( 'NONE',  ( 42.36021970110777346, -12.73296999994090584, -17.89321520033831447 ) ) ;
#21793 = CARTESIAN_POINT ( 'NONE',  ( 120.5110881442453206, -6.344957434206665248, -7.627207830600338134 ) ) ;
#21794 = CARTESIAN_POINT ( 'NONE',  ( 118.7525614775786380, -1.833838273342659253, -17.42832698103878286 ) ) ;
#21795 = CARTESIAN_POINT ( 'NONE',  ( 111.7184548109119788, -0.8288870151387760510, -10.36305467784173118 ) ) ;
#21796 = VERTEX_POINT ( 'NONE', #30753 ) ;
#21797 = CARTESIAN_POINT ( 'NONE',  ( 137.3527759848290373, -7.390398384115297148, -8.885999701577917520 ) ) ;
#21798 = CARTESIAN_POINT ( 'NONE',  ( 122.9503348109119827, 0.5811942927096110934, -14.16772938898807510 ) ) ;
#21799 = CARTESIAN_POINT ( 'NONE',  ( 113.3301452545248083, -9.868328341294098749, -15.46607636864997204 ) ) ;
#21800 = CARTESIAN_POINT ( 'NONE',  ( 119.0361948109119652, -2.084020599724406786, -8.691656652584148546 ) ) ;
#21801 = EDGE_CURVE ( 'NONE', #2299, #6072, #29089, .T. ) ;
#21802 = CARTESIAN_POINT ( 'NONE',  ( 118.0718414775786442, -0.8288870151387760510, -10.36305467784173118 ) ) ;
#21803 = CARTESIAN_POINT ( 'NONE',  ( 85.34650993476388692, -28.81703154067693617, -9.558501715626988471 ) ) ;
#21804 = CARTESIAN_POINT ( 'NONE',  ( 109.7880358795247986, -0.7896495226426338832, -17.46756447353520159 ) ) ;
#21805 = CARTESIAN_POINT ( 'NONE',  ( 121.9859814775786333, -9.565557343593413364, -10.61323700422348004 ) ) ;
#21806 = CARTESIAN_POINT ( 'NONE',  ( 123.1772414775786189, -5.574606645277164318, -18.38911715685844683 ) ) ;
#21807 = CARTESIAN_POINT ( 'NONE',  ( 94.20708369096698220, -25.99489077589524300, -13.39321520033831447 ) ) ;
#21808 = CARTESIAN_POINT ( 'NONE',  ( 109.2294421292701543, -7.690995191147263377, -8.440827004729632321 ) ) ;
#21809 = CARTESIAN_POINT ( 'NONE',  ( 119.7434548109119703, -2.527210466738041728, -8.967976844669124148 ) ) ;
#21810 = CARTESIAN_POINT ( 'NONE',  ( 115.9693640045247776, -10.62599879583958717, -11.00651665394454604 ) ) ;
#21811 = DIRECTION ( 'NONE',  ( -0.1352586133457954198, -0.9908103287288503314, 0.000000000000000000 ) ) ;
#21812 = CARTESIAN_POINT ( 'NONE',  ( 117.2294421295248270, 0.7813447578650477565, -21.83687654715277304 ) ) ;
#21813 = CARTESIAN_POINT ( 'NONE',  ( 117.4478481442453131, 0.2603800115204892296, -16.42320221600525088 ) ) ;
#21814 = CARTESIAN_POINT ( 'NONE',  ( 119.7736414775786358, -10.30919188438810075, -12.61870101168855918 ) ) ;
#21815 = CARTESIAN_POINT ( 'NONE',  ( 112.4967077545247633, -7.250697342233347165, -7.631215200338321125 ) ) ;
#21816 = CARTESIAN_POINT ( 'NONE',  ( 113.3068014775786594, -8.166667518702817929, -8.995218007635859436 ) ) ;
#21817 = ORIENTED_EDGE ( 'NONE', *, *, #37297, .T. ) ;
#21818 = CARTESIAN_POINT ( 'NONE',  ( 117.2928937256648965, -1.063912429576147511, -17.20460841810472985 ) ) ;
#21819 = CARTESIAN_POINT ( 'NONE',  ( 116.0864081442453113, -9.988377603198976828, -10.36322818467138340 ) ) ;
#21820 = EDGE_CURVE ( 'NONE', #9155, #14958, #19195, .T. ) ;
#21821 = AXIS2_PLACEMENT_3D ( 'NONE', #942, #14861, #15525 ) ;
#21822 = CARTESIAN_POINT ( 'NONE',  ( 122.5532481442453019, 0.4262465694468514643, -12.03445270309931736 ) ) ;
#21823 = B_SPLINE_CURVE_WITH_KNOTS ( 'NONE', 3,
 ( #22368, #15301, #35356, #11889 ),
 .UNSPECIFIED., .F., .F.,
 ( 4, 4 ),
 ( 0.000000000000000000, 1.000000000000000000 ),
 .UNSPECIFIED. ) ;
#21824 = CARTESIAN_POINT ( 'NONE',  ( 0.000000000000000000, 0.000000000000000000, 0.000000000000000000 ) ) ;
#21825 = CARTESIAN_POINT ( 'NONE',  ( 124.1415948109119540, -6.344957434206665248, -7.627207830600338134 ) ) ;
#21826 = CARTESIAN_POINT ( 'NONE',  ( 123.2906948109119867, -8.166667518702819706, -8.995218007635861213 ) ) ;
#21827 = CARTESIAN_POINT ( 'NONE',  ( 114.0246765045248196, -7.250697342233347165, -19.15521520033831138 ) ) ;
#21828 = CARTESIAN_POINT ( 'NONE',  ( 117.8449348109119938, -1.833838273342659253, -17.42832698103878286 ) ) ;
#21829 = CARTESIAN_POINT ( 'NONE',  ( 122.3826735609119680, 0.6414057260225851653, -11.69287257290600657 ) ) ;
#21830 = CARTESIAN_POINT ( 'NONE',  ( 119.7434548109119703, -9.722663502801697888, -19.87444018218530317 ) ) ;
#21831 = VERTEX_POINT ( 'NONE', #3385 ) ;
#21832 = CIRCLE ( 'NONE', #29122, 2.000000000000000444 ) ;
#21833 = CARTESIAN_POINT ( 'NONE',  ( 122.3826735609119680, 0.6414057260225851653, -11.69287257290600657 ) ) ;
#21834 = CARTESIAN_POINT ( 'NONE',  ( 119.3198281442452924, 0.5811942927096110934, -14.16772938898807510 ) ) ;
#21835 = ORIENTED_EDGE ( 'NONE', *, *, #21934, .T. ) ;
#21836 = CARTESIAN_POINT ( 'NONE',  ( 124.9819548109120291, -7.618532446444633344, -18.05174138884769874 ) ) ;
#21837 = CARTESIAN_POINT ( 'NONE',  ( 127.8924691488517453, -7.120506250460368669, -18.77659918890763890 ) ) ;
#21838 = CARTESIAN_POINT ( 'NONE',  ( 119.7963009221557513, -2.372251574601201174, -17.96033910819751611 ) ) ;
#21839 = CARTESIAN_POINT ( 'NONE',  ( 116.1998614775786507, 0.4262465694468514643, -12.03445270309931736 ) ) ;
#21840 = CARTESIAN_POINT ( 'NONE',  ( 77.59349808546981819, -56.93324028847530371, -1.549987343799404726 ) ) ;
#21841 = CARTESIAN_POINT ( 'NONE',  ( 64.06704089363852006, -35.12954632779501907, -5.893215200338315363 ) ) ;
#21842 = CARTESIAN_POINT ( 'NONE',  ( 119.0929214775786278, -4.153390946401325223, -8.397313243818185668 ) ) ;
#21843 = CARTESIAN_POINT ( 'NONE',  ( 121.4754414775786131, -8.166667518702800166, -8.995218007635847002 ) ) ;
#21844 = CARTESIAN_POINT ( 'NONE',  ( 121.8158014775786171, -4.153390946401325223, -8.397313243818185668 ) ) ;
#21845 = CIRCLE ( 'NONE', #23319, 2.999999999999999556 ) ;
#21846 = CARTESIAN_POINT ( 'NONE',  ( 124.1685108350158515, -12.47056798417068180, -10.95034471803594833 ) ) ;
#21847 = CARTESIAN_POINT ( 'NONE',  ( 123.8012348109119642, -9.565557343593413364, -10.61323700422348004 ) ) ;
#21848 = CARTESIAN_POINT ( 'NONE',  ( 113.0798948109119948, -0.4660016031367893996, -10.09054647747474043 ) ) ;
#21849 = CARTESIAN_POINT ( 'NONE',  ( 120.0572748109119772, -3.383040157471821630, -19.15922257007629170 ) ) ;
#21850 = CARTESIAN_POINT ( 'NONE',  ( 112.8529881442453302, -1.561330072975668060, -17.79121239304076596 ) ) ;
#21851 = LINE ( 'NONE', #3837, #28605 ) ;
#21852 = CARTESIAN_POINT ( 'NONE',  ( 119.8870948109119752, -0.8288870151387760510, -10.36305467784173118 ) ) ;
#21853 = VERTEX_POINT ( 'NONE', #13658 ) ;
#21854 = CARTESIAN_POINT ( 'NONE',  ( 120.5110881442453206, -6.344957434206665248, -7.627207830600338134 ) ) ;
#21855 = CARTESIAN_POINT ( 'NONE',  ( 112.0105358795248804, -8.402594152722688392, -9.854619843455216355 ) ) ;
#21856 = DIRECTION ( 'NONE',  ( 0.9609149988134837450, -0.1028163501681639419, 0.2570431154366518145 ) ) ;
#21857 = CARTESIAN_POINT ( 'NONE',  ( 114.0246765045248196, -2.791137627527939813, -8.388885654883754484 ) ) ;
#21858 = CIRCLE ( 'NONE', #3660, 3.249999999999996003 ) ;
#21859 = DIRECTION ( 'NONE',  ( 0.9609149988134837450, -0.1028163501681639419, 0.2570431154366518145 ) ) ;
#21860 = CARTESIAN_POINT ( 'NONE',  ( 73.07463722459043254, -56.63952039772598823, -34.96411198583172819 ) ) ;
#21861 = ORIENTED_EDGE ( 'NONE', *, *, #24038, .F. ) ;
#21862 = CIRCLE ( 'NONE', #22610, 2.999999999999999556 ) ;
#21863 = CARTESIAN_POINT ( 'NONE',  ( 2.181596283295915484, -11.50482699009217669, -17.89321520033831447 ) ) ;
#21864 = CARTESIAN_POINT ( 'NONE',  ( 123.2339681442453241, -3.505236298600246325, -18.68346056562440793 ) ) ;
#21865 = FACE_OUTER_BOUND ( 'NONE', #40, .T. ) ;
#21866 = CARTESIAN_POINT ( 'NONE',  ( 62.31167178596560774, -14.51130963312466626, -17.61767033193244103 ) ) ;
#21867 = CARTESIAN_POINT ( 'NONE',  ( 125.5597614775786326, -1.561330072975669392, -17.79121239304076951 ) ) ;
#21868 = CARTESIAN_POINT ( 'NONE',  ( 105.8986608795248401, -1.325403438956436419, -16.93181055722141792 ) ) ;
#21869 = ORIENTED_EDGE ( 'NONE', *, *, #23779, .F. ) ;
#21870 = CARTESIAN_POINT ( 'NONE',  ( 114.2144281442453178, -8.166667518702817929, -8.995218007635859436 ) ) ;
#21871 = CARTESIAN_POINT ( 'NONE',  ( 113.3635281442453504, -9.988377603198976828, -10.36322818467138340 ) ) ;
#21872 = CARTESIAN_POINT ( 'NONE',  ( 126.0703014775786102, -9.988377603198980381, -10.36322818467138518 ) ) ;
#21873 = CARTESIAN_POINT ( 'NONE',  ( 121.8158014775786171, -4.153390946401325223, -8.397313243818185668 ) ) ;
#21874 = EDGE_CURVE ( 'NONE', #30236, #25264, #24146, .T. ) ;
#21875 = DIRECTION ( 'NONE',  ( 1.000000000000000000, 0.000000000000000000, -0.000000000000000000 ) ) ;
#21876 = CARTESIAN_POINT ( 'NONE',  ( 122.5532481442453019, -10.63000616557722466, -14.87417383870573495 ) ) ;
#21877 = CARTESIAN_POINT ( 'NONE',  ( 96.54708369096698561, -24.69793907545987466, -15.18364567559777178 ) ) ;
#21878 = FACE_OUTER_BOUND ( 'NONE', #37850, .T. ) ;
#21879 = CARTESIAN_POINT ( 'NONE',  ( 67.30914723170953096, -59.73653352439050934, -37.99192222348830938 ) ) ;
#21880 = ORIENTED_EDGE ( 'NONE', *, *, #25317, .T. ) ;
#21881 = CIRCLE ( 'NONE', #41564, 5.999999999999997335 ) ;
#21882 = CARTESIAN_POINT ( 'NONE',  ( 120.7379948109119709, -10.63000616557722466, -14.87417383870573495 ) ) ;
#21883 = CARTESIAN_POINT ( 'NONE',  ( 66.83265463627490988, 0.3322498524448982415, -17.83539872533922122 ) ) ;
#21884 = VERTEX_POINT ( 'NONE', #45115 ) ;
#21885 = CARTESIAN_POINT ( 'NONE',  ( 112.0588148109119828, 0.5811942927096154232, -14.16772938898807155 ) ) ;
#21886 = CARTESIAN_POINT ( 'NONE',  ( 124.5954081442453116, -3.383040157471821630, -19.15922257007629170 ) ) ;
#21887 = CARTESIAN_POINT ( 'NONE',  ( 127.4620922276975818, -4.355667135866661432, -18.99210946691642832 ) ) ;
#21888 = CARTESIAN_POINT ( 'NONE',  ( 123.9714148109119805, -8.899110576539710493, -16.42337572283490132 ) ) ;
#21889 = VERTEX_POINT ( 'NONE', #17736 ) ;
#21890 = VECTOR ( 'NONE', #6514, 1000.000000000000000 ) ;
#21891 = CARTESIAN_POINT ( 'NONE',  ( 119.3765548109119834, 0.9020085738987339008, -11.91225656197089222 ) ) ;
#21892 = CARTESIAN_POINT ( 'NONE',  ( 123.9584548109119737, -4.863998795839242995, -13.39321520033831447 ) ) ;
#21893 = VECTOR ( 'NONE', #10439, 1000.000000000000000 ) ;
#21894 = FACE_OUTER_BOUND ( 'NONE', #28313, .T. ) ;
#21895 = CARTESIAN_POINT ( 'NONE',  ( 137.5098831408921001, -4.032236636546677744, -8.461637928299781564 ) ) ;
#21896 = CARTESIAN_POINT ( 'NONE',  ( 123.8579614775786126, 0.5811942927096110934, -14.16772938898807510 ) ) ;
#21897 = CARTESIAN_POINT ( 'NONE',  ( 89.01247232317646763, -25.99489077589524300, -13.39321520033831447 ) ) ;
#21898 = DIRECTION ( 'NONE',  ( 1.000000000000000000, 0.000000000000000000, 0.000000000000000000 ) ) ;
#21899 = CARTESIAN_POINT ( 'NONE',  ( 125.3328548109119964, -9.261995988541697145, -16.69588392320189030 ) ) ;
#21900 = CARTESIAN_POINT ( 'NONE',  ( 123.8579614775786126, -9.859900752359378018, -12.68260735090039759 ) ) ;
#21901 = CARTESIAN_POINT ( 'NONE',  ( 116.6387481731040481, -9.478760661942724042, -15.43013221979977700 ) ) ;
#21902 = CARTESIAN_POINT ( 'NONE',  ( 125.1626748109119802, -0.1624402480850797581, -16.17319339645315424 ) ) ;
#21903 = CYLINDRICAL_SURFACE ( 'NONE', #5831, 0.9999999999999952260 ) ;
#21904 = CARTESIAN_POINT ( 'NONE',  ( 119.4900081442453086, -1.834011780172310813, -8.268836392978581529 ) ) ;
#21905 = VERTEX_POINT ( 'NONE', #21156 ) ;
#21906 = ORIENTED_EDGE ( 'NONE', *, *, #45118, .F. ) ;
#21907 = CARTESIAN_POINT ( 'NONE',  ( 127.9806007748781838, -8.501439814973640097, -18.01472541506584335 ) ) ;
#21908 = CARTESIAN_POINT ( 'NONE',  ( 85.43169907558235820, -25.38011337280982715, -14.88121679464376257 ) ) ;
#21909 = CARTESIAN_POINT ( 'NONE',  ( 105.7597546295248350, -4.863998795839590272, -7.631215200338315796 ) ) ;
#21910 = CARTESIAN_POINT ( 'NONE',  ( 112.9828796295247884, -4.863998795839590272, -8.388885654883775800 ) ) ;
#21911 = CONICAL_SURFACE ( 'NONE', #12456, 2.445500000000004448, 0.9599310885968757034 ) ;
#21912 = CARTESIAN_POINT ( 'NONE',  ( 126.2184548109108420, -9.810113536895345376, -12.66056213194485558 ) ) ;
#21913 = CARTESIAN_POINT ( 'NONE',  ( 114.5547881442453217, -5.638512984488999180, -18.83840828888717311 ) ) ;
#21914 = ORIENTED_EDGE ( 'NONE', *, *, #8067, .T. ) ;
#21915 = CARTESIAN_POINT ( 'NONE',  ( 112.4559014775786778, -0.1624402480850797581, -16.17319339645315424 ) ) ;
#21916 = CARTESIAN_POINT ( 'NONE',  ( 106.3153796295248412, -4.863998795839590272, -19.15521520033831493 ) ) ;
#21917 = CARTESIAN_POINT ( 'NONE',  ( 70.19691569158496236, 3.834886253390165756, -4.893215200338314474 ) ) ;
#21918 = CARTESIAN_POINT ( 'NONE',  ( 112.2857214775786474, -5.574606645277164318, -18.38911715685844683 ) ) ;
#21919 = DIRECTION ( 'NONE',  ( -0.9387755102040816757, 0.3445294493088600918, 0.000000000000000000 ) ) ;
#21920 = CARTESIAN_POINT ( 'NONE',  ( 61.93156847455979630, -13.30602482174417034, -19.05359815343103236 ) ) ;
#21921 = CARTESIAN_POINT ( 'NONE',  ( 116.2565881442452991, -9.261995988541697145, -16.69588392320189030 ) ) ;
#21922 = CARTESIAN_POINT ( 'NONE',  ( 114.9970202545248412, -10.62599879583958717, -15.77991374673208469 ) ) ;
#21923 = CARTESIAN_POINT ( 'NONE',  ( 113.3301452545248083, -9.868328341294098749, -15.46607636864997204 ) ) ;
#21924 = VERTEX_POINT ( 'NONE', #35031 ) ;
#21925 = CARTESIAN_POINT ( 'NONE',  ( 126.3999550322324410, -7.499531571443311506, -9.037731752716881672 ) ) ;
#21926 = CARTESIAN_POINT ( 'NONE',  ( 119.9438214775786378, -2.084020599724406786, -8.691656652584148546 ) ) ;
#21927 = CARTESIAN_POINT ( 'NONE',  ( 115.7460481442453357, 0.9020085738987339008, -11.91225656197089222 ) ) ;
#21928 = CARTESIAN_POINT ( 'NONE',  ( 113.4769814775786330, -10.63000616557722466, -14.87417383870573495 ) ) ;
#21929 = CIRCLE ( 'NONE', #8101, 5.000000000000000000 ) ;
#21930 = CARTESIAN_POINT ( 'NONE',  ( 118.1285681442452926, -2.084020599724404121, -8.691656652584155651 ) ) ;
#21931 = CARTESIAN_POINT ( 'NONE',  ( 119.1496481442453046, -6.222761293078241884, -8.102969835052219238 ) ) ;
#21932 = CARTESIAN_POINT ( 'NONE',  ( 114.3846081442453197, 0.4262465694468514643, -12.03445270309931736 ) ) ;
#21933 = ORIENTED_EDGE ( 'NONE', *, *, #17126, .T. ) ;
#21934 = EDGE_CURVE ( 'NONE', #32179, #38238, #20669, .T. ) ;
#21935 = CARTESIAN_POINT ( 'NONE',  ( 124.6746266859119743, -9.033780868592240054, -16.85052413769862056 ) ) ;
#21936 = CARTESIAN_POINT ( 'NONE',  ( 94.86797725101187950, -25.11844467255894031, -13.58832973634262409 ) ) ;
#21937 = CARTESIAN_POINT ( 'NONE',  ( 116.7104014775786425, -8.899110576539710493, -16.42337572283490132 ) ) ;
#21938 = VERTEX_POINT ( 'NONE', #44900 ) ;
#21939 = CARTESIAN_POINT ( 'NONE',  ( 110.7640389883689807, 0.3193521225029610777, -12.14321520033833224 ) ) ;
#21940 = CARTESIAN_POINT ( 'NONE',  ( 115.1220548109119761, -8.166667518702817929, -8.995218007635861213 ) ) ;
#21941 = EDGE_CURVE ( 'NONE', #39054, #34542, #23575, .T. ) ;
#21942 = CARTESIAN_POINT ( 'NONE',  ( 107.8433483795247838, -8.402594152722688392, -16.93181055722141792 ) ) ;
#21943 = CARTESIAN_POINT ( 'NONE',  ( 113.4202548109119846, 0.1319031606808879209, -14.10382304977623669 ) ) ;
#21944 = ORIENTED_EDGE ( 'NONE', *, *, #16655, .F. ) ;
#21945 = EDGE_LOOP ( 'NONE', ( #5302, #20773 ) ) ;
#21946 = CIRCLE ( 'NONE', #33581, 2.999999999999999556 ) ;
#21947 = CARTESIAN_POINT ( 'NONE',  ( 122.2696148109119889, -5.574606645277164318, -18.38911715685844683 ) ) ;
#21948 = CARTESIAN_POINT ( 'NONE',  ( 118.5823814775786360, -7.643976991954077427, -18.09477374809248928 ) ) ;
#21949 = CARTESIAN_POINT ( 'NONE',  ( 124.5787747700264276, -9.818244482720213995, -14.09103721618573601 ) ) ;
#21950 = CARTESIAN_POINT ( 'NONE',  ( 120.9241579359119925, -5.444069387712269226, -19.60292469916370450 ) ) ;
#21951 = ORIENTED_EDGE ( 'NONE', *, *, #18619, .F. ) ;
#21952 = CARTESIAN_POINT ( 'NONE',  ( 74.43213512091445239, -36.61236768192972590, -7.393215200338315363 ) ) ;
#21953 = CARTESIAN_POINT ( 'NONE',  ( 71.67504600870660170, -26.72445618319088823, -4.893215200338314474 ) ) ;
#21954 = CARTESIAN_POINT ( 'NONE',  ( 113.0523327545247838, -2.477300249445798297, -19.15521520033831138 ) ) ;
#21955 = CIRCLE ( 'NONE', #5218, 2.999999999999999556 ) ;
#21956 = CARTESIAN_POINT ( 'NONE',  ( 113.7606148109119886, -1.561330072975668060, -17.79121239304076596 ) ) ;
#21957 = PRODUCT ( 'Cable Anchor', 'Cable Anchor', '', ( #2639 ) ) ;
#21958 = ADVANCED_FACE ( 'NONE', ( #31410 ), #41262, .F. ) ;
#21959 = CARTESIAN_POINT ( 'NONE',  ( 112.4559014775786494, -9.988377603198976828, -10.36322818467138340 ) ) ;
#21960 = CARTESIAN_POINT ( 'NONE',  ( 119.8870948109119752, -0.8288870151387760510, -10.36305467784173118 ) ) ;
#21961 = DIRECTION ( 'NONE',  ( -0.000000000000000000, -0.9284778069183721172, -0.3713878862591650232 ) ) ;
#21962 = EDGE_CURVE ( 'NONE', #12848, #30236, #16273, .T. ) ;
#21963 = EDGE_CURVE ( 'NONE', #15771, #41059, #22832, .T. ) ;
#21964 = EDGE_LOOP ( 'NONE', ( #6571, #12288, #31025, #22609, #36979 ) ) ;
#21965 = CARTESIAN_POINT ( 'NONE',  ( 120.0572748109119772, -6.222761293078241884, -8.102969835052219238 ) ) ;
#21966 = CARTESIAN_POINT ( 'NONE',  ( 111.7184548109119788, -8.862178061932382889, -16.39564131203247399 ) ) ;
#21967 = DIRECTION ( 'NONE',  ( -0.000000000000000000, -0.9284778069183721172, -0.3713878862591650232 ) ) ;
#21968 = CARTESIAN_POINT ( 'NONE',  ( 117.0174177730625900, 0.4131681913238580139, -12.14321520033831625 ) ) ;
#21969 = CARTESIAN_POINT ( 'NONE',  ( 117.5613014775786525, 0.9020085738987339008, -11.91225656197089222 ) ) ;
#21970 = EDGE_LOOP ( 'NONE', ( #1842, #11916, #26469, #42665, #43164, #31572 ) ) ;
#21971 = CARTESIAN_POINT ( 'NONE',  ( 118.6391081442452986, -4.089484607189486809, -7.948022111789456723 ) ) ;
#21972 = CARTESIAN_POINT ( 'NONE',  ( 70.19189222814998175, -62.62292920857806422, -38.25196254438899501 ) ) ;
#21973 = CARTESIAN_POINT ( 'NONE',  ( 113.7468640045248236, -10.62599879583958717, -11.00651665394454604 ) ) ;
#21974 = CARTESIAN_POINT ( 'NONE',  ( 115.9162281442453235, -4.089484607189486809, -7.948022111789456723 ) ) ;
#21975 = CARTESIAN_POINT ( 'NONE',  ( 116.5969481442453031, 0.5811942927096154232, -14.16772938898807155 ) ) ;
#21976 = CARTESIAN_POINT ( 'NONE',  ( 127.1653849502121858, -10.32489337370534166, -13.76497012726351876 ) ) ;
#21977 = CARTESIAN_POINT ( 'NONE',  ( 62.36331481589586900, -14.51968798477179412, -17.59173035813085662 ) ) ;
#21978 = CARTESIAN_POINT ( 'NONE',  ( 105.3430358795248338, -8.402594152722688392, -9.854619843455216355 ) ) ;
#21979 = EDGE_LOOP ( 'NONE', ( #44332, #31897, #31005, #15218, #24914 ) ) ;
#21980 = CARTESIAN_POINT ( 'NONE',  ( 116.5564130180080866, 0.7607806665037644134, -14.64321520033833401 ) ) ;
#21981 = CARTESIAN_POINT ( 'NONE',  ( 109.2294421291983184, -10.01537527712310549, -11.01699420138576180 ) ) ;
#21982 = CIRCLE ( 'NONE', #2311, 2.000000000000000444 ) ;
#21983 = CARTESIAN_POINT ( 'NONE',  ( 120.0572748109119772, -6.222761293078241884, -8.102969835052219238 ) ) ;
#21984 = CARTESIAN_POINT ( 'NONE',  ( 111.5938171295247940, 0.1403307496149613920, -13.39321520033831447 ) ) ;
#21985 = CARTESIAN_POINT ( 'NONE',  ( 115.4137390045248566, -9.868328341294098749, -11.32035403202665869 ) ) ;
#21986 = CARTESIAN_POINT ( 'NONE',  ( 121.6412059692789427, -1.179503403430468333, -17.05068175419387089 ) ) ;
#21987 = CARTESIAN_POINT ( 'NONE',  ( 112.5693548109119888, 0.4262465694468514643, -12.03445270309931736 ) ) ;
#21988 = CYLINDRICAL_SURFACE ( 'NONE', #37202, 1.999999999999998890 ) ;
#21989 = CARTESIAN_POINT ( 'NONE',  ( 123.2906948109119867, -8.166667518702819706, -8.995218007635861213 ) ) ;
#21990 = CARTESIAN_POINT ( 'NONE',  ( 119.8870948109119752, -9.261995988541697145, -16.69588392320189030 ) ) ;
#21991 = ORIENTED_EDGE ( 'NONE', *, *, #20384, .F. ) ;
#21992 = ADVANCED_FACE ( 'NONE', ( #14092 ), #20274, .F. ) ;
#21993 = CARTESIAN_POINT ( 'NONE',  ( 117.1642148109119859, -0.8288870151387760510, -10.36305467784173118 ) ) ;
#21994 = CARTESIAN_POINT ( 'NONE',  ( 112.1722681442453222, -0.4660016031367893996, -10.09054647747474043 ) ) ;
#21995 = CARTESIAN_POINT ( 'NONE',  ( 119.4900081442453086, -1.834011780172310813, -8.268836392978581529 ) ) ;
#21996 = CARTESIAN_POINT ( 'NONE',  ( 118.8660148109119774, 0.1319031606808879209, -14.10382304977623669 ) ) ;
#21997 = VERTEX_POINT ( 'NONE', #34600 ) ;
#21998 = CARTESIAN_POINT ( 'NONE',  ( 116.3461286830089989, -1.087735405160625834, -17.17288456429612964 ) ) ;
#21999 = CARTESIAN_POINT ( 'NONE',  ( 121.0783548109119749, 0.2603800115204892296, -16.42320221600525088 ) ) ;
#22000 = CARTESIAN_POINT ( 'NONE',  ( 113.1366214775786432, -7.643976991954077427, -18.09477374809248928 ) ) ;
#22001 = CARTESIAN_POINT ( 'NONE',  ( 108.3989733795248753, -8.938348069036489818, -17.46756447353520159 ) ) ;
#22002 = DIRECTION ( 'NONE',  ( 0.000000000000000000, -0.9242245927363028635, -0.3818493186865930533 ) ) ;
#22003 = CYLINDRICAL_SURFACE ( 'NONE', #30270, 8.000000000000000000 ) ;
#22004 = CARTESIAN_POINT ( 'NONE',  ( 112.5661608795247872, -1.325403438956436419, -16.93181055722141792 ) ) ;
#22005 = AXIS2_PLACEMENT_3D ( 'NONE', #30950, #17278, #27987 ) ;
#22006 = CARTESIAN_POINT ( 'NONE',  ( 119.7736414775786358, -10.30919188438810075, -12.61870101168855918 ) ) ;
#22007 = DIRECTION ( 'NONE',  ( -0.9908103287288504424, 0.1352586133457951423, 0.000000000000000000 ) ) ;
#22008 = CARTESIAN_POINT ( 'NONE',  ( 116.5969481442453031, -9.859900752359374465, -12.68260735090039404 ) ) ;
#22009 = CARTESIAN_POINT ( 'NONE',  ( 126.0703014775786102, -9.988377603198980381, -10.36322818467138518 ) ) ;
#22010 = CARTESIAN_POINT ( 'NONE',  ( 126.2758031835797254, -0.6776192674585240772, -10.60718350710181035 ) ) ;
#22011 = EDGE_CURVE ( 'NONE', #29903, #32851, #13385, .T. ) ;
#22012 = CARTESIAN_POINT ( 'NONE',  ( 35.90261398037149121, 14.17005867477686820, -18.19321520033831519 ) ) ;
#22013 = CARTESIAN_POINT ( 'NONE',  ( 110.4131140045248287, 0.1403307496149616695, -15.46607636864997204 ) ) ;
#22014 = CARTESIAN_POINT ( 'NONE',  ( 113.5904348109119866, -2.084020599724406786, -8.691656652584148546 ) ) ;
#22015 = CARTESIAN_POINT ( 'NONE',  ( 115.1037688976800268, -1.244021962887382315, -16.96476564598603787 ) ) ;
#22016 = AXIS2_PLACEMENT_3D ( 'NONE', #5227, #43998, #19141 ) ;
#22017 = CARTESIAN_POINT ( 'NONE',  ( 123.0385396737536752, -8.611453504372539314, -17.77011218421760574 ) ) ;
#22019 = CARTESIAN_POINT ( 'NONE',  ( 120.0572748109119772, -3.383040157471821630, -19.15922257007629170 ) ) ;
#22018 = CARTESIAN_POINT ( 'NONE',  ( 63.48716809568579578, -14.78506867088062471, -8.380858988663437259 ) ) ;
#22020 = CARTESIAN_POINT ( 'NONE',  ( 119.9438214775786378, -2.084020599724406786, -8.691656652584148546 ) ) ;
#22021 = CARTESIAN_POINT ( 'NONE',  ( 113.9307948109119764, -10.15424416112533912, -14.75197769757731336 ) ) ;
#22022 = VERTEX_POINT ( 'NONE', #13438 ) ;
#22023 = CARTESIAN_POINT ( 'NONE',  ( 137.0134976903368340, -7.178400362679481006, -8.454421406160578911 ) ) ;
#22024 = EDGE_CURVE ( 'NONE', #41199, #424, #24280, .T. ) ;
#22025 = CARTESIAN_POINT ( 'NONE',  ( 121.5888948109119809, -10.30919188438810075, -12.61870101168855918 ) ) ;
#22026 = CARTESIAN_POINT ( 'NONE',  ( 115.2053796295247849, -4.863998795839590272, -8.388885654883775800 ) ) ;
#22027 = CARTESIAN_POINT ( 'NONE',  ( 120.0005481442453146, -4.153390946401325223, -8.397313243818185668 ) ) ;
#22028 = CARTESIAN_POINT ( 'NONE',  ( 122.3830681442452857, -1.833838273342659697, -17.42832698103878286 ) ) ;
#22029 = CARTESIAN_POINT ( 'NONE',  ( 115.9729548109119861, -3.505236298600246325, -18.68346056562440793 ) ) ;
#22030 = CARTESIAN_POINT ( 'NONE',  ( 124.0650380271193995, 2.753853830864835484, -15.83610243082555691 ) ) ;
#22031 = CARTESIAN_POINT ( 'NONE',  ( 109.9269421295247753, 0.8980012041604618078, -13.39321520033831447 ) ) ;
#22032 = CARTESIAN_POINT ( 'NONE',  ( 122.2696148109119889, -5.574606645277164318, -18.38911715685844683 ) ) ;
#22033 = CARTESIAN_POINT ( 'NONE',  ( 122.6667014775786413, -2.084020599724406786, -8.691656652584148546 ) ) ;
#22034 = DIRECTION ( 'NONE',  ( 0.000000000000000000, -0.9242245927363029745, -0.3818493186865927758 ) ) ;
#22035 = DIRECTION ( 'NONE',  ( -0.000000000000000000, -0.9284778069183721172, -0.3713878862591650232 ) ) ;
#22036 = CARTESIAN_POINT ( 'NONE',  ( 121.8270485609119760, -0.08252387247370887580, -11.91645802438286417 ) ) ;
#22037 = CARTESIAN_POINT ( 'NONE',  ( 115.2748327545248657, -2.477300249445798297, -19.15521520033831138 ) ) ;
#22038 = CARTESIAN_POINT ( 'NONE',  ( 117.1512660175612126, 1.479770359400331747, -21.46523989841215396 ) ) ;
#22039 = CARTESIAN_POINT ( 'NONE',  ( 83.83011982744213242, -31.85041140898378487, -20.99942768933297543 ) ) ;
#22040 = CARTESIAN_POINT ( 'NONE',  ( 116.5402214775786405, 0.2603800115204892296, -16.42320221600525088 ) ) ;
#22041 = CARTESIAN_POINT ( 'NONE',  ( 118.8660148109119774, -10.30919188438810075, -12.61870101168855918 ) ) ;
#22042 = DIRECTION ( 'NONE',  ( 0.9609149988134843001, -0.1028163501681632064, 0.2570431154366505933 ) ) ;
#22043 =( BOUNDED_CURVE ( )  B_SPLINE_CURVE ( 3, ( #9291, #23200, #9976, #13615 ),
 .UNSPECIFIED., .F., .F. ) 
 B_SPLINE_CURVE_WITH_KNOTS ( ( 4, 4 ),
 ( 0.6164973811836809148, 1.570796326794899889 ),
 .UNSPECIFIED. ) 
 CURVE ( )  GEOMETRIC_REPRESENTATION_ITEM ( )  RATIONAL_B_SPLINE_CURVE ( ( 1.000000000000000000, 0.9255384209705479481, 0.9255384209705479481, 1.000000000000000000 ) ) 
 REPRESENTATION_ITEM ( '' )  );
#22044 = CARTESIAN_POINT ( 'NONE',  ( 113.9875214775786532, -0.4660016031367893996, -10.09054647747474043 ) ) ;
#22045 = DIRECTION ( 'NONE',  ( 0.8636456077245089347, -0.5040994586965590329, 0.000000000000000000 ) ) ;
#22046 = ORIENTED_EDGE ( 'NONE', *, *, #6157, .F. ) ;
#22047 = LINE ( 'NONE', #1958, #10153 ) ;
#22048 = VECTOR ( 'NONE', #42954, 1000.000000000000000 ) ;
#22049 = CARTESIAN_POINT ( 'NONE',  ( 117.9016614775786280, -9.988377603198976828, -10.36322818467138340 ) ) ;
#22050 = CARTESIAN_POINT ( 'NONE',  ( 121.2485348109119769, -8.899110576539710493, -16.42337572283490132 ) ) ;
#22051 = DIRECTION ( 'NONE',  ( 1.000000000000000000, 0.000000000000000000, 0.000000000000000000 ) ) ;
#22052 = CARTESIAN_POINT ( 'NONE',  ( 113.2500748109119968, -3.505236298600246325, -18.68346056562440793 ) ) ;
#22053 = CARTESIAN_POINT ( 'NONE',  ( 122.6099748109119929, -9.261995988541697145, -16.69588392320189030 ) ) ;
#22054 = CARTESIAN_POINT ( 'NONE',  ( 115.3442858795247759, -0.7896495226426338832, -17.46756447353520159 ) ) ;
#22055 = CIRCLE ( 'NONE', #38807, 2.999999999999999556 ) ;
#22056 = CARTESIAN_POINT ( 'NONE',  ( 114.7816948109119863, -9.859900752359374465, -12.68260735090039404 ) ) ;
#22057 = CARTESIAN_POINT ( 'NONE',  ( 122.7993923109119692, -9.959231468620755479, -10.70263013195267199 ) ) ;
#22058 = DIRECTION ( 'NONE',  ( 0.000000000000000000, 0.3818493186865927203, -0.9242245927363029745 ) ) ;
#22059 = VERTEX_POINT ( 'NONE', #10020 ) ;
#22060 = EDGE_CURVE ( 'NONE', #11967, #30697, #4040, .T. ) ;
#22061 = CARTESIAN_POINT ( 'NONE',  ( 122.7299391859119737, -8.844754642576884152, -8.592115655440050404 ) ) ;
#22062 = CARTESIAN_POINT ( 'NONE',  ( 118.2420214775786320, -3.383040157471821630, -19.15922257007629170 ) ) ;
#22063 = ORIENTED_EDGE ( 'NONE', *, *, #30909, .T. ) ;
#22064 = LINE ( 'NONE', #15447, #13123 ) ;
#22065 = CARTESIAN_POINT ( 'NONE',  ( -13.40759878756898260, -4.990576376016446325, -7.482946478807211754 ) ) ;
#22066 = CARTESIAN_POINT ( 'NONE',  ( 115.2566360982116862, 0.3867979994853637526, -12.14321520033831625 ) ) ;
#22067 = B_SPLINE_CURVE_WITH_KNOTS ( 'NONE', 3,
 ( #22546, #15714, #16170, #29616, #12300, #9325, #43760, #30074, #26426, #26650 ),
 .UNSPECIFIED., .F., .F.,
 ( 4, 3, 3, 4 ),
 ( 0.000000000000000000, 0.0001671877548681249956, 0.0003343755096277635291, 0.0006463528481650629171 ),
 .UNSPECIFIED. ) ;
#22068 = CARTESIAN_POINT ( 'NONE',  ( 114.2711548109119803, -0.1624402480850797581, -16.17319339645315424 ) ) ;
#22069 = DIRECTION ( 'NONE',  ( 1.000000000000000000, 0.000000000000000000, -0.000000000000000000 ) ) ;
#22070 = CARTESIAN_POINT ( 'NONE',  ( 124.5079745746482871, -9.690323912439273712, -12.08684339900582749 ) ) ;
#22071 = CARTESIAN_POINT ( 'NONE',  ( 121.8725281442453223, -6.222761293078241884, -8.102969835052219238 ) ) ;
#22072 = DIRECTION ( 'NONE',  ( -0.7071067811865475727, -0.4246071727180998345, 0.5654279342907827521 ) ) ;
#22073 = CIRCLE ( 'NONE', #38084, 2.999999999999998224 ) ;
#22074 = CARTESIAN_POINT ( 'NONE',  ( 125.1626748109119802, -0.1624402480850797581, -16.17319339645315424 ) ) ;
#22075 = AXIS2_PLACEMENT_3D ( 'NONE', #6799, #3370, #17289 ) ;
#22076 = ADVANCED_FACE ( 'NONE', ( #23929 ), #17031, .T. ) ;
#22077 = CARTESIAN_POINT ( 'NONE',  ( 124.3692356341927336, -12.42554980965305766, -10.94897534285865426 ) ) ;
#22078 = EDGE_CURVE ( 'NONE', #9582, #2844, #31547, .T. ) ;
#22079 = CARTESIAN_POINT ( 'NONE',  ( 124.3685014775786328, 0.4262465694468514643, -12.03445270309931736 ) ) ;
#22080 = CARTESIAN_POINT ( 'NONE',  ( 113.1933481442453058, -4.089484607189486809, -7.948022111789456723 ) ) ;
#22081 = CARTESIAN_POINT ( 'NONE',  ( 120.5678148109119832, -8.166667518702819706, -8.995218007635861213 ) ) ;
#22082 = CARTESIAN_POINT ( 'NONE',  ( 113.8173414775786512, 0.2603800115204892296, -16.42320221600525088 ) ) ;
#22083 = CARTESIAN_POINT ( 'NONE',  ( 59.90552009294157898, -2.897503654462289191, -17.89321520033831447 ) ) ;
#22084 = CARTESIAN_POINT ( 'NONE',  ( 122.1561614775786353, -8.899110576539710493, -16.42337572283490132 ) ) ;
#22085 = EDGE_LOOP ( 'NONE', ( #22417, #24803, #26269 ) ) ;
#22086 = CARTESIAN_POINT ( 'NONE',  ( 120.5678148109119832, -8.166667518702819706, -8.995218007635861213 ) ) ;
#22087 = CARTESIAN_POINT ( 'NONE',  ( 113.8857702545248003, 0.1403307496149616695, -11.32035403202665336 ) ) ;
#22088 = CARTESIAN_POINT ( 'NONE',  ( 82.53726425729240646, -31.76580277050288004, -22.96761734921603448 ) ) ;
#22089 = AXIS2_PLACEMENT_3D ( 'NONE', #29622, #22552, #33020 ) ;
#22090 = CARTESIAN_POINT ( 'NONE',  ( 112.9097148109120070, -9.565557343593413364, -10.61323700422348004 ) ) ;
#22091 = CARTESIAN_POINT ( 'NONE',  ( 138.0748658142820204, -3.091679250359711695, -17.00231359494076955 ) ) ;
#22092 = CARTESIAN_POINT ( 'NONE',  ( 115.8999108795247821, -1.325403438956436419, -16.93181055722141792 ) ) ;
#22093 = EDGE_LOOP ( 'NONE', ( #27102, #9495, #16052, #41426, #11895 ) ) ;
#22094 = CARTESIAN_POINT ( 'NONE',  ( 120.6245414775786458, -0.1624402480850797581, -16.17319339645315424 ) ) ;
#22095 = DIRECTION ( 'NONE',  ( -0.7071067811865481278, -0.5654279342906992634, -0.4246071727182101907 ) ) ;
#22096 = CARTESIAN_POINT ( 'NONE',  ( 122.9382985609119743, -10.36940331770106916, -15.09355782777062061 ) ) ;
#22097 = CARTESIAN_POINT ( 'NONE',  ( 126.1837548109119211, -10.63000616557722466, -14.87417383870573495 ) ) ;
#22098 = CARTESIAN_POINT ( 'NONE',  ( 107.4266296295248821, -4.863998795839590272, -8.388885654883775800 ) ) ;
#22099 = VERTEX_POINT ( 'NONE', #28904 ) ;
#22100 = CARTESIAN_POINT ( 'NONE',  ( 113.7606148109119886, -1.561330072975668060, -17.79121239304076596 ) ) ;
#22101 = LINE ( 'NONE', #25972, #7269 ) ;
#22102 = CARTESIAN_POINT ( 'NONE',  ( 122.2128881442453263, -7.643976991954077427, -18.09477374809248928 ) ) ;
#22103 = CARTESIAN_POINT ( 'NONE',  ( 112.8529881442453302, -7.894159318335828068, -9.358103419637847864 ) ) ;
#22104 =( NAMED_UNIT ( * ) SI_UNIT ( $, .STERADIAN. ) SOLID_ANGLE_UNIT ( ) );
#22105 = CARTESIAN_POINT ( 'NONE',  ( 111.8319081442453182, -4.153390946401321671, -8.397313243818183892 ) ) ;
#22106 = FACE_OUTER_BOUND ( 'NONE', #34860, .T. ) ;
#22107 = ORIENTED_EDGE ( 'NONE', *, *, #41910, .F. ) ;
#22108 =( GEOMETRIC_REPRESENTATION_CONTEXT ( 3 ) GLOBAL_UNCERTAINTY_ASSIGNED_CONTEXT ( ( #38801 ) ) GLOBAL_UNIT_ASSIGNED_CONTEXT ( ( #15721, #33251, #16176 ) ) REPRESENTATION_CONTEXT ( 'NONE', 'WORKASPACE' ) );
#22109 = CARTESIAN_POINT ( 'NONE',  ( 115.1359265045248605, -2.791137627527939813, -8.388885654883777576 ) ) ;
#22110 = AXIS2_PLACEMENT_3D ( 'NONE', #41309, #41742, #24190 ) ;
#22111 = CARTESIAN_POINT ( 'NONE',  ( 122.3263414775786373, -6.344957434206665248, -7.627207830600338134 ) ) ;
#22112 = CARTESIAN_POINT ( 'NONE',  ( 136.4173705901596350, -10.20608232061555576, -15.61275821664342978 ) ) ;
#22113 = ORIENTED_EDGE ( 'NONE', *, *, #35208, .F. ) ;
#22114 = DIRECTION ( 'NONE',  ( -0.000000000000000000, -0.9284778069183721172, -0.3713878862591650232 ) ) ;
#22115 = CARTESIAN_POINT ( 'NONE',  ( 125.7299414775786346, 0.9020085738987339008, -11.91225656197089222 ) ) ;
#22116 = CARTESIAN_POINT ( 'NONE',  ( 105.6208483795248299, -0.7896495226426338832, -9.318865927141430916 ) ) ;
#22117 = CARTESIAN_POINT ( 'NONE',  ( 123.4608748109119745, 0.4262465694468514643, -12.03445270309931736 ) ) ;
#22118 = ORIENTED_EDGE ( 'NONE', *, *, #5344, .T. ) ;
#22119 = CARTESIAN_POINT ( 'NONE',  ( 119.6034614775786196, -6.344957434206665248, -7.627207830600338134 ) ) ;
#22120 = FACE_OUTER_BOUND ( 'NONE', #244, .T. ) ;
#22121 = SPHERICAL_SURFACE ( 'NONE', #3625, 6.500000000000000000 ) ;
#22122 = CARTESIAN_POINT ( 'NONE',  ( 124.1546421904525346, -1.211725351588312183, -20.50025038867522653 ) ) ;
#22123 = FACE_OUTER_BOUND ( 'NONE', #26230, .T. ) ;
#22124 = CARTESIAN_POINT ( 'NONE',  ( 112.2289948109119848, -7.643976991954077427, -18.09477374809248928 ) ) ;
#22125 = DIRECTION ( 'NONE',  ( -0.000000000000000000, -0.9284778069183718952, -0.3713878862591649677 ) ) ;
#22126 = EDGE_CURVE ( 'NONE', #29422, #10447, #848, .T. ) ;
#22127 = DIRECTION ( 'NONE',  ( 1.000000000000000000, 0.000000000000000000, -0.000000000000000000 ) ) ;
#22128 = CARTESIAN_POINT ( 'NONE',  ( 112.3424481442453384, -3.505236298600246325, -18.68346056562440793 ) ) ;
#22129 = CARTESIAN_POINT ( 'NONE',  ( 125.2761281442453054, 0.4262465694468514643, -12.03445270309931736 ) ) ;
#22130 = CARTESIAN_POINT ( 'NONE',  ( 116.6466789632009835, -9.331272246221795186, -15.78281339210872680 ) ) ;
#22131 = CARTESIAN_POINT ( 'NONE',  ( 122.2128881442453263, -7.643976991954077427, -18.09477374809248928 ) ) ;
#22132 = CARTESIAN_POINT ( 'NONE',  ( 113.0231681442453180, -10.15424416112533912, -14.75197769757731336 ) ) ;
#22133 = CARTESIAN_POINT ( 'NONE',  ( 118.0718414775786300, -9.261995988541697145, -16.69588392320189030 ) ) ;
#22134 = CIRCLE ( 'NONE', #31597, 2.000000000000000444 ) ;
#22135 = EDGE_LOOP ( 'NONE', ( #40537, #19493, #11233, #30816, #27532 ) ) ;
#22136 = CARTESIAN_POINT ( 'NONE',  ( 126.4536383592497231, -8.582534964477776640, -16.90949643156282889 ) ) ;
#22137 = CARTESIAN_POINT ( 'NONE',  ( 70.19189222814998175, -40.46710316615127567, -32.62080435916936239 ) ) ;
#22138 = CARTESIAN_POINT ( 'NONE',  ( 109.7880358795247986, -8.402594152722688392, -9.854619843455216355 ) ) ;
#22139 = CARTESIAN_POINT ( 'NONE',  ( 113.8857702545248003, 0.1403307496149616695, -11.32035403202665336 ) ) ;
#22140 = CARTESIAN_POINT ( 'NONE',  ( 125.5597614775786326, -7.894159318336616771, -9.358103419638441167 ) ) ;
#22141 = CARTESIAN_POINT ( 'NONE',  ( 115.8027748109119841, -0.4660016031367893996, -10.09054647747474043 ) ) ;
#22142 = ORIENTED_EDGE ( 'NONE', *, *, #39514, .T. ) ;
#22143 = CARTESIAN_POINT ( 'NONE',  ( 115.0086014775786509, -5.574606645277164318, -18.38911715685844683 ) ) ;
#22144 = CARTESIAN_POINT ( 'NONE',  ( 109.0935046295247872, -4.863998795839590272, -7.631215200338315796 ) ) ;
#22145 = DIRECTION ( 'NONE',  ( 0.000000000000000000, -0.9242245927363028635, -0.3818493186865930533 ) ) ;
#22146 = CARTESIAN_POINT ( 'NONE',  ( 119.9638582044368320, -6.247802574075781656, -18.73351920797576042 ) ) ;
#22147 = CARTESIAN_POINT ( 'NONE',  ( 125.4584548109119737, -12.49632558250451986, -9.362893955355607645 ) ) ;
#22148 = CARTESIAN_POINT ( 'NONE',  ( 87.44708369096657918, -25.99489077589588604, -12.39321520033831447 ) ) ;
#22149 = CARTESIAN_POINT ( 'NONE',  ( 115.2922348109119781, -10.63000616557722466, -14.87417383870573495 ) ) ;
#22150 = CARTESIAN_POINT ( 'NONE',  ( 112.1494421295248003, 0.8980012041604618078, -13.39321520033831447 ) ) ;
#22151 = CARTESIAN_POINT ( 'NONE',  ( 110.8992858795247827, -8.402594152722688392, -9.854619843455216355 ) ) ;
#22152 = ORIENTED_EDGE ( 'NONE', *, *, #27340, .F. ) ;
#22153 = CARTESIAN_POINT ( 'NONE',  ( -1.145390592550938669, -14.88589425535891841, -19.39321520033831447 ) ) ;
#22154 = CARTESIAN_POINT ( 'NONE',  ( 119.6601881442453106, -1.833838273342659253, -17.42832698103878286 ) ) ;
#22155 = CARTESIAN_POINT ( 'NONE',  ( 116.0296814775786345, -8.166667518702817929, -8.995218007635861213 ) ) ;
#22156 = CARTESIAN_POINT ( 'NONE',  ( 113.0798948109119948, -0.4660016031367893996, -10.09054647747474043 ) ) ;
#22157 = CARTESIAN_POINT ( 'NONE',  ( 124.7088614775786226, -9.565557343593413364, -10.61323700422348004 ) ) ;
#22158 = CARTESIAN_POINT ( 'NONE',  ( 122.1561614775786353, -8.899110576539710493, -16.42337572283490132 ) ) ;
#22159 = CARTESIAN_POINT ( 'NONE',  ( 116.3133148109120043, -2.084020599724406786, -8.691656652584148546 ) ) ;
#22160 = ORIENTED_EDGE ( 'NONE', *, *, #33064, .F. ) ;
#22161 = CARTESIAN_POINT ( 'NONE',  ( 120.1601735609119856, 0.6414057260225851653, -11.69287257290600657 ) ) ;
#22162 = CARTESIAN_POINT ( 'NONE',  ( 64.84865456828643460, -21.86021636429758530, -5.893215200338315363 ) ) ;
#22163 = CARTESIAN_POINT ( 'NONE',  ( 117.2776681442452968, -4.153390946401325223, -8.397313243818185668 ) ) ;
#22164 = ORIENTED_EDGE ( 'NONE', *, *, #24471, .F. ) ;
#22165 = CARTESIAN_POINT ( 'NONE',  ( 116.1998614775786507, -10.63000616557722466, -14.87417383870573495 ) ) ;
#22166 = AXIS2_PLACEMENT_3D ( 'NONE', #10251, #28023, #34171 ) ;
#22167 = CARTESIAN_POINT ( 'NONE',  ( 108.1906140045248037, 0.1403307496149616695, -15.46607636864997204 ) ) ;
#22168 = CARTESIAN_POINT ( 'NONE',  ( 112.6828081442453282, -2.084020599724406786, -8.691656652584148546 ) ) ;
#22169 = VERTEX_POINT ( 'NONE', #21606 ) ;
#22170 = ORIENTED_EDGE ( 'NONE', *, *, #24486, .T. ) ;
#22171 = CARTESIAN_POINT ( 'NONE',  ( 121.3052614775786111, -7.643976991954077427, -18.09477374809248928 ) ) ;
#22172 = CARTESIAN_POINT ( 'NONE',  ( 116.8805814775786445, -3.505236298600246325, -18.68346056562440793 ) ) ;
#22173 = CARTESIAN_POINT ( 'NONE',  ( 124.5933994731490202, -9.737703366526362814, -14.52892336661181005 ) ) ;
#22174 = CARTESIAN_POINT ( 'NONE',  ( 116.6536748109119941, -10.15424416112534267, -14.75197769757730804 ) ) ;
#22175 = ORIENTED_EDGE ( 'NONE', *, *, #35777, .T. ) ;
#22176 = CARTESIAN_POINT ( 'NONE',  ( 112.1708206037811948, -8.908198244330842286, -16.40957177738907191 ) ) ;
#22177 = CARTESIAN_POINT ( 'NONE',  ( 62.56519830863885545, -64.88825862050514104, -45.66019302834368432 ) ) ;
#22178 = CARTESIAN_POINT ( 'NONE',  ( 109.8574890045247940, 0.8980012041604421569, -15.77991374673208469 ) ) ;
#22179 = CARTESIAN_POINT ( 'NONE',  ( 116.4267681442453153, -3.383040157471821630, -19.15922257007629170 ) ) ;
#22181 = CARTESIAN_POINT ( 'NONE',  ( 115.9729548109119861, -3.505236298600246325, -18.68346056562440793 ) ) ;
#22180 = CARTESIAN_POINT ( 'NONE',  ( 125.5030348109119558, -6.222761293078241884, -8.102969835052219238 ) ) ;
#22182 = CARTESIAN_POINT ( 'NONE',  ( 122.3830681442452857, -1.833838273342659697, -17.42832698103878286 ) ) ;
#22183 = DIRECTION ( 'NONE',  ( 0.000000000000000000, -0.7876185884367603585, 0.6161630946014904353 ) ) ;
#22184 = EDGE_LOOP ( 'NONE', ( #29938, #6493, #22374, #36422 ) ) ;
#22185 = CARTESIAN_POINT ( 'NONE',  ( 119.0929214775786278, -4.153390946401325223, -8.397313243818185668 ) ) ;
#22186 = DIRECTION ( 'NONE',  ( 0.000000000000000000, -0.6004852223388321697, 0.7996358532186280677 ) ) ;
#22187 = CONICAL_SURFACE ( 'NONE', #22901, 1.610000000000000986, 0.9599310885968765916 ) ;
#22188 = DIRECTION ( 'NONE',  ( 0.000000000000000000, -0.9242245927363028635, -0.3818493186865930533 ) ) ;
#22189 = CARTESIAN_POINT ( 'NONE',  ( 116.7333483795247844, -8.402594152722688392, -16.93181055722141792 ) ) ;
#22190 = CARTESIAN_POINT ( 'NONE',  ( 114.2330358795247776, -0.7896495226426338832, -17.46756447353520159 ) ) ;
#22191 = CARTESIAN_POINT ( 'NONE',  ( 119.8870948109119752, -9.261995988541697145, -16.69588392320189030 ) ) ;
#22192 = ORIENTED_EDGE ( 'NONE', *, *, #26163, .T. ) ;
#22193 = CARTESIAN_POINT ( 'NONE',  ( 117.1642148109119859, -9.261995988541697145, -16.69588392320189030 ) ) ;
#22194 = CARTESIAN_POINT ( 'NONE',  ( 115.1403407241439396, -2.443475742715333965, -17.86549347949429389 ) ) ;
#22195 = CARTESIAN_POINT ( 'NONE',  ( 106.0375671295248310, -10.62599879583958540, -13.39321520033831447 ) ) ;
#22196 = CARTESIAN_POINT ( 'NONE',  ( 115.9729548109119861, -6.344957434206662583, -7.627207830600332805 ) ) ;
#22197 = CARTESIAN_POINT ( 'NONE',  ( 116.7104014775786425, -0.4660016031367893996, -10.09054647747474043 ) ) ;
#22199 = CIRCLE ( 'NONE', #22912, 2.445500000000004448 ) ;
#22198 = CARTESIAN_POINT ( 'NONE',  ( 127.0400190879688012, -10.26619878979528799, -13.69785579496253014 ) ) ;
#22200 = LINE ( 'NONE', #8522, #41011 ) ;
#22201 = FACE_OUTER_BOUND ( 'NONE', #34473, .T. ) ;
#22202 = VERTEX_POINT ( 'NONE', #32312 ) ;
#22203 = CARTESIAN_POINT ( 'NONE',  ( 121.7187960087704113, -6.176492496456559955, -18.59847741292036716 ) ) ;
#22204 = CARTESIAN_POINT ( 'NONE',  ( 109.2294476533355692, -10.02000977116478708, -15.26446378573822038 ) ) ;
#22205 = CARTESIAN_POINT ( 'NONE',  ( 121.9292548109119849, -7.894159318335828068, -9.358103419637847864 ) ) ;
#22206 = CARTESIAN_POINT ( 'NONE',  ( 110.7603796295247918, -4.863998795839590272, -8.388885654883775800 ) ) ;
#22207 = CARTESIAN_POINT ( 'NONE',  ( 115.0664733795247798, -1.325403438956436419, -9.854619843455211026 ) ) ;
#22208 = CARTESIAN_POINT ( 'NONE',  ( 115.8595014775786609, -7.643976991954077427, -18.09477374809248928 ) ) ;
#22209 = CARTESIAN_POINT ( 'NONE',  ( 89.67401078471493747, -26.75858941326842810, -11.54476601486570964 ) ) ;
#22210 = CARTESIAN_POINT ( 'NONE',  ( 113.9307948109119764, -10.15424416112533912, -14.75197769757731336 ) ) ;
#22211 = CARTESIAN_POINT ( 'NONE',  ( 120.0005481442453146, -5.638512984488999180, -18.83840828888717311 ) ) ;
#22212 = ORIENTED_EDGE ( 'NONE', *, *, #8181, .F. ) ;
#22213 = CARTESIAN_POINT ( 'NONE',  ( 120.0572748109119772, -6.222761293078241884, -8.102969835052219238 ) ) ;
#22214 = CARTESIAN_POINT ( 'NONE',  ( 115.9729548109119861, -6.344957434206662583, -7.627207830600332805 ) ) ;
#22215 = CARTESIAN_POINT ( 'NONE',  ( 120.6812681442452941, -10.30919188438810075, -12.61870101168855918 ) ) ;
#22216 = B_SPLINE_CURVE_WITH_KNOTS ( 'NONE', 3,
 ( #21210, #2983, #38085, #27835, #41314, #41748, #10509, #13488, #14369, #24410, #28283, #24634, #38300 ),
 .UNSPECIFIED., .F., .F.,
 ( 4, 3, 3, 3, 4 ),
 ( 2.934973642780345169E-16, 1.132108791046253874E-05, 5.660632326038089941E-05, 0.0001397594989357112019, 0.0002229354582960460030 ),
 .UNSPECIFIED. ) ;
#22217 = CARTESIAN_POINT ( 'NONE',  ( 120.1707281442453166, -9.565557343593413364, -10.61323700422348004 ) ) ;
#22218 = VERTEX_POINT ( 'NONE', #28683 ) ;
#22219 = CARTESIAN_POINT ( 'NONE',  ( 124.7655881442452852, -9.859900752359378018, -12.68260735090039759 ) ) ;
#22220 = EDGE_CURVE ( 'NONE', #31523, #39064, #4722, .T. ) ;
#22221 = CIRCLE ( 'NONE', #28059, 5.000000000000004441 ) ;
#22222 = CARTESIAN_POINT ( 'NONE',  ( 121.8158014775786171, -5.638512984488999180, -18.83840828888717311 ) ) ;
#22223 = LINE ( 'NONE', #8099, #20922 ) ;
#22224 = VECTOR ( 'NONE', #18746, 1000.000000000000000 ) ;
#22225 = LINE ( 'NONE', #17911, #37346 ) ;
#22226 = LINE ( 'NONE', #40003, #7706 ) ;
#22227 = CARTESIAN_POINT ( 'NONE',  ( 112.0105358795247810, -8.402594152722688392, -9.854619843455216355 ) ) ;
#22228 = DIRECTION ( 'NONE',  ( 0.000000000000000000, 0.000000000000000000, 1.000000000000000000 ) ) ;
#22229 = CARTESIAN_POINT ( 'NONE',  ( 117.5045748109119756, -9.859900752359374465, -12.68260735090039404 ) ) ;
#22230 = CARTESIAN_POINT ( 'NONE',  ( 111.8319081442453182, -4.153390946401321671, -8.397313243818183892 ) ) ;
#22231 = CARTESIAN_POINT ( 'NONE',  ( 64.59716620846640467, -13.12735690504239017, -15.45707635952990344 ) ) ;
#22232 = CARTESIAN_POINT ( 'NONE',  ( 117.0111608795247946, -1.325403438956436419, -16.93181055722141792 ) ) ;
#22233 = CARTESIAN_POINT ( 'NONE',  ( 111.8716296295247901, -4.863998795839590272, -8.388885654883775800 ) ) ;
#22234 = CARTESIAN_POINT ( 'NONE',  ( 115.0086014775786509, -5.574606645277164318, -18.38911715685844683 ) ) ;
#22235 = CARTESIAN_POINT ( 'NONE',  ( 114.7607665278262630, -1.036737761566196570, -17.24079555149560505 ) ) ;
#22236 = EDGE_CURVE ( 'NONE', #29748, #44499, #35901, .T. ) ;
#22237 = CARTESIAN_POINT ( 'NONE',  ( -1.813282010071980421, -6.828405667812914359, -18.61931990332739062 ) ) ;
#22239 = CARTESIAN_POINT ( 'NONE',  ( 118.9794681442453026, -9.261995988541697145, -16.69588392320189030 ) ) ;
#22238 = CARTESIAN_POINT ( 'NONE',  ( 65.01231714173856346, -15.66127537904516132, -9.355441156750886833 ) ) ;
#22240 = VECTOR ( 'NONE', #32937, 1000.000000000000000 ) ;
#22241 = CARTESIAN_POINT ( 'NONE',  ( 121.1918081442452859, -10.15424416112533912, -14.75197769757731336 ) ) ;
#22242 = ORIENTED_EDGE ( 'NONE', *, *, #6637, .T. ) ;
#22243 = CARTESIAN_POINT ( 'NONE',  ( 137.3019930433568447, -8.583162301624891910, -9.736487546999564202 ) ) ;
#22244 = CARTESIAN_POINT ( 'NONE',  ( 125.7299414775786346, 0.9020085738987339008, -11.91225656197089222 ) ) ;
#22245 = CARTESIAN_POINT ( 'NONE',  ( 108.8851452545248151, -9.868328341294098749, -15.46607636864997204 ) ) ;
#22246 = CARTESIAN_POINT ( 'NONE',  ( 119.3198281442452924, -9.859900752359374465, -12.68260735090039404 ) ) ;
#22247 = ADVANCED_FACE ( 'NONE', ( #7921 ), #21369, .T. ) ;
#22248 = CARTESIAN_POINT ( 'NONE',  ( 123.2339681442453241, -3.505236298600246325, -18.68346056562440793 ) ) ;
#22249 = CARTESIAN_POINT ( 'NONE',  ( 116.1998614775786507, 0.4262465694468514643, -12.03445270309931736 ) ) ;
#22250 = EDGE_CURVE ( 'NONE', #20329, #34274, #40287, .T. ) ;
#22251 = CARTESIAN_POINT ( 'NONE',  ( 125.1433143116076394, 2.106814825465578522, -15.97349185543337668 ) ) ;
#22252 = CARTESIAN_POINT ( 'NONE',  ( 107.2877233795247776, -8.938348069036489818, -17.46756447353520159 ) ) ;
#22253 = TOROIDAL_SURFACE ( 'NONE', #30981, 26.50000000000000000, 1.500000000000000000 ) ;
#22254 = CARTESIAN_POINT ( 'NONE',  ( 124.5954081442453116, -6.222761293078241884, -8.102969835052219238 ) ) ;
#22255 = CARTESIAN_POINT ( 'NONE',  ( 124.7655881442452852, -9.859900752359378018, -12.68260735090039759 ) ) ;
#22256 = CARTESIAN_POINT ( 'NONE',  ( 109.2294421295247844, 7.836001204160461420, -12.14321520033831625 ) ) ;
#22257 = CARTESIAN_POINT ( 'NONE',  ( 68.89072742534011695, -72.01748991317985826, -37.14555542905099372 ) ) ;
#22258 = CARTESIAN_POINT ( 'NONE',  ( 121.2019704359119743, -10.25716656981731489, -12.88942061488890545 ) ) ;
#22259 = CARTESIAN_POINT ( 'NONE',  ( 116.3166296295247832, -4.863998795839590272, -19.15521520033831493 ) ) ;
#22260 = CARTESIAN_POINT ( 'NONE',  ( -13.82150966199706588, -4.445790862645441877, -18.50085597516207514 ) ) ;
#22261 = CARTESIAN_POINT ( 'NONE',  ( 83.86185565543740950, -31.76393747133379009, -22.76090678561018521 ) ) ;
#22262 = CARTESIAN_POINT ( 'NONE',  ( 121.6456214775786293, -10.63000616557722466, -14.87417383870573495 ) ) ;
#22263 = CARTESIAN_POINT ( 'NONE',  ( 118.4689281442453392, 0.9020085738987339008, -11.91225656197089222 ) ) ;
#22264 = CARTESIAN_POINT ( 'NONE',  ( 105.9681140045248355, -10.62599879583958717, -11.00651665394454604 ) ) ;
#22265 = CARTESIAN_POINT ( 'NONE',  ( 112.9664414775786412, 0.5811942927096154232, -14.16772938898807155 ) ) ;
#22266 = DIRECTION ( 'NONE',  ( -1.000000000000000000, 0.000000000000000000, 0.000000000000000000 ) ) ;
#22267 = ORIENTED_EDGE ( 'NONE', *, *, #40464, .F. ) ;
#22268 = DIRECTION ( 'NONE',  ( 1.000000000000000000, 0.000000000000000000, 0.000000000000000000 ) ) ;
#22269 = CONICAL_SURFACE ( 'NONE', #42680, 2.445500000000004448, 0.9599310885968757034 ) ;
#22270 = EDGE_CURVE ( 'NONE', #27865, #35613, #31859, .T. ) ;
#22271 = CARTESIAN_POINT ( 'NONE',  ( 118.2987481442453088, -1.561330072975668504, -17.79121239304076951 ) ) ;
#22272 = CARTESIAN_POINT ( 'NONE',  ( 125.6732148109119862, -9.859900752359378018, -12.68260735090039759 ) ) ;
#22273 = SHAPE_DEFINITION_REPRESENTATION ( #25240, #21588 ) ;
#22274 = EDGE_CURVE ( 'NONE', #31284, #17364, #8256, .T. ) ;
#22275 = CARTESIAN_POINT ( 'NONE',  ( 114.1577014775786552, -3.505236298600246325, -18.68346056562440793 ) ) ;
#22276 = CARTESIAN_POINT ( 'NONE',  ( 125.1626748109119802, -9.988377603198980381, -10.36322818467138518 ) ) ;
#22277 = EDGE_CURVE ( 'NONE', #35171, #36351, #11576, .T. ) ;
#22278 = EDGE_CURVE ( 'NONE', #2517, #1411, #10053, .T. ) ;
#22279 = CARTESIAN_POINT ( 'NONE',  ( 113.0523327545247838, -2.477300249445798297, -19.15521520033831138 ) ) ;
#22280 = CARTESIAN_POINT ( 'NONE',  ( 119.7736414775786358, 0.1319031606808879209, -14.10382304977623669 ) ) ;
#22281 = FACE_OUTER_BOUND ( 'NONE', #21720, .T. ) ;
#22282 = AXIS2_PLACEMENT_3D ( 'NONE', #37275, #29997, #36820 ) ;
#22283 = DIRECTION ( 'NONE',  ( 0.000000000000000000, -0.3818493186865936084, 0.9242245927363024194 ) ) ;
#22284 = VERTEX_POINT ( 'NONE', #7691 ) ;
#22285 = CARTESIAN_POINT ( 'NONE',  ( 121.7575954359119805, -11.07370829466463569, -12.81314460846529002 ) ) ;
#22286 = CARTESIAN_POINT ( 'NONE',  ( 119.7169148109119874, -9.988377603198976828, -10.36322818467138340 ) ) ;
#22287 = ORIENTED_EDGE ( 'NONE', *, *, #35051, .T. ) ;
#22288 = CARTESIAN_POINT ( 'NONE',  ( 122.5664060953690466, -6.001247023715324147, -18.26661038929047010 ) ) ;
#22289 = CARTESIAN_POINT ( 'NONE',  ( 67.69801799180082469, -1.521560346498090022, -9.966191704370915616 ) ) ;
#22290 = DIRECTION ( 'NONE',  ( -1.000000000000000000, 0.000000000000000000, 0.000000000000000000 ) ) ;
#22291 = CARTESIAN_POINT ( 'NONE',  ( 118.0151148109119816, 0.4262465694468514643, -12.03445270309931736 ) ) ;
#22292 = CARTESIAN_POINT ( 'NONE',  ( 70.19189222814998175, -100.0979043305785581, -53.24182196210380624 ) ) ;
#22293 = CARTESIAN_POINT ( 'NONE',  ( 124.5262951945957042, -9.799039402788389808, -12.58795091330891580 ) ) ;
#22294 = CARTESIAN_POINT ( 'NONE',  ( 124.4252281442452812, -0.8288870151387760510, -10.36305467784173118 ) ) ;
#22295 = CARTESIAN_POINT ( 'NONE',  ( 89.78938736644981589, -25.99489077589524300, -13.39321520033831625 ) ) ;
#22296 = CARTESIAN_POINT ( 'NONE',  ( 124.7088614775786226, -9.565557343593413364, -10.61323700422348004 ) ) ;
#22297 = CARTESIAN_POINT ( 'NONE',  ( 125.2382274389888295, -12.00999942234432538, -14.79627280731742012 ) ) ;
#22298 = CARTESIAN_POINT ( 'NONE',  ( 116.5402214775786405, -9.565557343593413364, -10.61323700422348004 ) ) ;
#22299 = CARTESIAN_POINT ( 'NONE',  ( 121.4754414775786131, -1.833838273342659697, -17.42832698103878286 ) ) ;
#22300 = CARTESIAN_POINT ( 'NONE',  ( 112.0588148109119828, 0.5811942927096154232, -14.16772938898807155 ) ) ;
#22301 = CARTESIAN_POINT ( 'NONE',  ( 118.0718414775786300, -9.261995988541697145, -16.69588392320189030 ) ) ;
#22302 = CARTESIAN_POINT ( 'NONE',  ( 117.0507614775786465, -10.30919188438810075, -12.61870101168855918 ) ) ;
#22303 = DIRECTION ( 'NONE',  ( 0.000000000000000000, 0.000000000000000000, -1.000000000000000000 ) ) ;
#22304 =( BOUNDED_SURFACE ( )  B_SPLINE_SURFACE ( 1, 2, ( 
 ( #40013, #32926, #36128, #29529, #2377, #40476, #5356, #1927, #19272, #16307, #5123, #12665, #8778, #33151, #1478, #1702, #40701 ),
 ( #16075, #15853, #22232, #15399, #19494, #8557, #43661, #22458, #36352, #26336, #40243, #22909, #43896, #36802, #5570, #3066, #17426 ) ),
 .UNSPECIFIED., .F., .F., .T. ) 
 B_SPLINE_SURFACE_WITH_KNOTS ( ( 2, 2 ),
 ( 3, 2, 2, 2, 2, 2, 2, 2, 3 ),
 ( 0.000000000000000000, 1.000000000000000000 ),
 ( 0.000000000000000000, 0.1250000000000000000, 0.2500000000000000000, 0.3750000000000000000, 0.5000000000000000000, 0.6250000000000000000, 0.7500000000000000000, 0.8750000000000000000, 1.000000000000000000 ),
 .UNSPECIFIED. ) 
 GEOMETRIC_REPRESENTATION_ITEM ( )  RATIONAL_B_SPLINE_SURFACE ( (
 ( 1.000000000000000000, 0.9238795325112869605, 1.000000000000000000, 0.9238795325112869605, 1.000000000000000000, 0.9238795325112869605, 1.000000000000000000, 0.9238795325112869605, 1.000000000000000000, 0.9238795325112869605, 1.000000000000000000, 0.9238795325112869605, 1.000000000000000000, 0.9238795325112869605, 1.000000000000000000, 0.9238795325112869605, 1.000000000000000000),
 ( 1.000000000000000000, 0.9238795325112869605, 1.000000000000000000, 0.9238795325112869605, 1.000000000000000000, 0.9238795325112869605, 1.000000000000000000, 0.9238795325112869605, 1.000000000000000000, 0.9238795325112869605, 1.000000000000000000, 0.9238795325112869605, 1.000000000000000000, 0.9238795325112869605, 1.000000000000000000, 0.9238795325112869605, 1.000000000000000000) ) ) 
 REPRESENTATION_ITEM ( '' )  SURFACE ( )  );
#22305 = CARTESIAN_POINT ( 'NONE',  ( 125.5597614775786326, -7.894159318335828068, -9.358103419637847864 ) ) ;
#22306 = ORIENTED_EDGE ( 'NONE', *, *, #21116, .F. ) ;
#22307 = CARTESIAN_POINT ( 'NONE',  ( 120.8514481442452961, -7.893985811506177619, -18.51759400769804742 ) ) ;
#22308 = CARTESIAN_POINT ( 'NONE',  ( 106.6626452545248611, -9.868328341294098749, -15.46607636864997204 ) ) ;
#22309 = CARTESIAN_POINT ( 'NONE',  ( 112.9828796295247884, -4.863998795839590272, -8.388885654883775800 ) ) ;
#22310 = FACE_OUTER_BOUND ( 'NONE', #41131, .T. ) ;
#22311 = CARTESIAN_POINT ( 'NONE',  ( 112.3991748109119868, -1.833838273342658809, -17.42832698103878286 ) ) ;
#22312 = CARTESIAN_POINT ( 'NONE',  ( 67.30914723170953096, -50.45175545520677929, -34.27804336089664616 ) ) ;
#22313 = AXIS2_PLACEMENT_3D ( 'NONE', #5759, #8525, #12174 ) ;
#22314 = CARTESIAN_POINT ( 'NONE',  ( 126.1837548109119211, -10.63000616557722466, -14.87417383870573495 ) ) ;
#22315 = ORIENTED_EDGE ( 'NONE', *, *, #14542, .F. ) ;
#22316 = CARTESIAN_POINT ( 'NONE',  ( 122.8936081442453059, -9.565557343593413364, -10.61323700422348004 ) ) ;
#22317 = CARTESIAN_POINT ( 'NONE',  ( 70.19189222814998175, -60.97346038181336070, -37.59218076343751136 ) ) ;
#22318 = CARTESIAN_POINT ( 'NONE',  ( 123.7717360609119623, -6.564341423271550902, -7.887810678476487425 ) ) ;
#22319 = CARTESIAN_POINT ( 'NONE',  ( 68.56885555382550024, -20.41671115022302274, -19.39321520033831447 ) ) ;
#22320 = CARTESIAN_POINT ( 'NONE',  ( 105.7597546295248350, -4.863998795839590272, -18.39754474579285315 ) ) ;
#22321 = AXIS2_PLACEMENT_3D ( 'NONE', #38710, #1093, #28699 ) ;
#22322 = VERTEX_POINT ( 'NONE', #39156 ) ;
#22323 = CARTESIAN_POINT ( 'NONE',  ( 114.0442481442453300, -1.834011780172310813, -8.268836392978581529 ) ) ;
#22324 = DIRECTION ( 'NONE',  ( -0.2407039305251456596, 0.3604685577742790525, -0.9011792478113757054 ) ) ;
#22325 = CARTESIAN_POINT ( 'NONE',  ( 119.6601881442453106, -1.833838273342659253, -17.42832698103878286 ) ) ;
#22326 = CARTESIAN_POINT ( 'NONE',  ( 113.0798948109119948, -8.899110576539710493, -16.42337572283490132 ) ) ;
#22327 = DIRECTION ( 'NONE',  ( 0.000000000000000000, 0.9284778069183720062, 0.3713878862591650232 ) ) ;
#22328 = CARTESIAN_POINT ( 'NONE',  ( 115.1010702440515558, -2.467220198592777525, -17.83387418641524391 ) ) ;
#22329 = CARTESIAN_POINT ( 'NONE',  ( 125.6164881442453094, -9.565557343593413364, -10.61323700422348004 ) ) ;
#22330 = VERTEX_POINT ( 'NONE', #18185 ) ;
#22331 = CONICAL_SURFACE ( 'NONE', #6317, 2.000000000000000444, 0.9599310885968830309 ) ;
#22332 = CARTESIAN_POINT ( 'NONE',  ( 117.0806140045248185, 0.1403307496149616695, -15.46607636864997204 ) ) ;
#22333 = CARTESIAN_POINT ( 'NONE',  ( 118.7525614775786380, -8.166667518702819706, -8.995218007635861213 ) ) ;
#22334 = CARTESIAN_POINT ( 'NONE',  ( 135.8497638153270373, -10.40529151342853709, -15.59585623059315651 ) ) ;
#22335 = ORIENTED_EDGE ( 'NONE', *, *, #29791, .T. ) ;
#22336 = EDGE_CURVE ( 'NONE', #13270, #24335, #4497, .T. ) ;
#22337 = CARTESIAN_POINT ( 'NONE',  ( 112.7395348109119766, -5.638512984488999180, -18.83840828888717311 ) ) ;
#22338 = CARTESIAN_POINT ( 'NONE',  ( 125.8433948109119456, -1.834011780172310813, -8.268836392978581529 ) ) ;
#22339 = CARTESIAN_POINT ( 'NONE',  ( 135.3184548109119874, -4.863998795839242995, -13.39321520033831447 ) ) ;
#22340 = CARTESIAN_POINT ( 'NONE',  ( 124.9357681442453014, -7.643976991954077427, -18.09477374809248928 ) ) ;
#22341 = VERTEX_POINT ( 'NONE', #10902 ) ;
#22342 = CARTESIAN_POINT ( 'NONE',  ( 118.4122014775786340, 0.5811942927096110934, -14.16772938898807510 ) ) ;
#22344 = DIRECTION ( 'NONE',  ( 0.000000000000000000, -0.3818493186865927203, 0.9242245927363029745 ) ) ;
#22343 = AXIS2_PLACEMENT_3D ( 'NONE', #5777, #19474, #30418 ) ;
#22345 = CARTESIAN_POINT ( 'NONE',  ( 75.95778847736514194, -3.256761025687008537, -14.39321520033831625 ) ) ;
#22346 = CARTESIAN_POINT ( 'NONE',  ( 115.0646051332721811, 0.2334052082820642360, -14.64321520033831447 ) ) ;
#22347 = CARTESIAN_POINT ( 'NONE',  ( 135.3184548109119874, -5.622599431619523358, -7.441364641445410655 ) ) ;
#22348 = CARTESIAN_POINT ( 'NONE',  ( 114.0442481442453300, -7.643976991954077427, -18.09477374809248928 ) ) ;
#22349 = CARTESIAN_POINT ( 'NONE',  ( 70.19189222814998175, -53.90613343638955968, -34.76527462071035046 ) ) ;
#22350 = CARTESIAN_POINT ( 'NONE',  ( 125.3086838498437317, -2.252769241038413472, -20.05322569067225658 ) ) ;
#22351 = CARTESIAN_POINT ( 'NONE',  ( 112.4559014775786778, -0.1624402480850797581, -16.17319339645315424 ) ) ;
#22352 = CARTESIAN_POINT ( 'NONE',  ( 112.5693548109119888, -10.63000616557722466, -14.87417383870573495 ) ) ;
#22353 = CARTESIAN_POINT ( 'NONE',  ( 116.6382829425946284, -9.487340216247861946, -15.40942383360363799 ) ) ;
#22354 = CARTESIAN_POINT ( 'NONE',  ( 124.7655881442452852, -9.859900752359378018, -12.68260735090039759 ) ) ;
#22355 = CARTESIAN_POINT ( 'NONE',  ( 112.5693548109119888, 0.4262465694468514643, -12.03445270309931736 ) ) ;
#22356 = CARTESIAN_POINT ( 'NONE',  ( 120.2274548109119934, 0.5811942927096110934, -14.16772938898807510 ) ) ;
#22357 = VECTOR ( 'NONE', #8828, 1000.000000000000000 ) ;
#22358 = CARTESIAN_POINT ( 'NONE',  ( 120.3976348109119812, -1.834011780172310813, -8.268836392978581529 ) ) ;
#22359 = ORIENTED_EDGE ( 'NONE', *, *, #5500, .F. ) ;
#22360 = CARTESIAN_POINT ( 'NONE',  ( 75.95778847736514194, -3.256761025687008537, -10.89321520033831447 ) ) ;
#22361 = CARTESIAN_POINT ( 'NONE',  ( 109.1629577545248395, -2.791137627527939813, -18.39754474579286025 ) ) ;
#22362 = CARTESIAN_POINT ( 'NONE',  ( 107.9822546295247889, -4.863998795839590272, -18.39754474579285315 ) ) ;
#22363 = CARTESIAN_POINT ( 'NONE',  ( 126.4599182912947413, -9.818254414970132515, -12.09804486832614856 ) ) ;
#22364 = CARTESIAN_POINT ( 'NONE',  ( 115.5191414775786569, -3.383040157471821630, -19.15922257007629170 ) ) ;
#22365 = ORIENTED_EDGE ( 'NONE', *, *, #22503, .F. ) ;
#22366 = CARTESIAN_POINT ( 'NONE',  ( 106.8015515045248378, -2.477300249445798297, -7.631215200338321125 ) ) ;
#22367 = DIRECTION ( 'NONE',  ( 0.000000000000000000, 0.9284778069183720062, 0.3713878862591650232 ) ) ;
#22368 = CARTESIAN_POINT ( 'NONE',  ( 111.2646414775786496, -8.899110576539710493, -16.42337572283490132 ) ) ;
#22369 = CARTESIAN_POINT ( 'NONE',  ( 109.2294421295247844, 0.1210096558822565393, -14.64321520034217805 ) ) ;
#22370 = CARTESIAN_POINT ( 'NONE',  ( 122.9351092294923831, -2.263366209404226392, -18.10533625161308180 ) ) ;
#22371 = CARTESIAN_POINT ( 'NONE',  ( 119.1496481442453046, -3.383040157471821630, -19.15922257007629170 ) ) ;
#22372 = CARTESIAN_POINT ( 'NONE',  ( 108.9545983795247821, -0.7896495226426338832, -9.318865927141430916 ) ) ;
#22373 = CARTESIAN_POINT ( 'NONE',  ( 112.2883483795247770, -8.402594152722688392, -16.93181055722141792 ) ) ;
#22374 = ORIENTED_EDGE ( 'NONE', *, *, #32613, .T. ) ;
#22375 = CARTESIAN_POINT ( 'NONE',  ( 118.6958348109119754, -3.505236298600246325, -18.68346056562440793 ) ) ;
#22376 = CARTESIAN_POINT ( 'NONE',  ( 115.9162281442453235, -4.089484607189486809, -7.948022111789456723 ) ) ;
#22377 = VECTOR ( 'NONE', #24414, 1000.000000000000114 ) ;
#22378 = CARTESIAN_POINT ( 'NONE',  ( 46.84966980880212617, -19.07391775237791620, -19.39321520033831447 ) ) ;
#22379 = CARTESIAN_POINT ( 'NONE',  ( 123.4608748109119745, 0.4262465694468514643, -12.03445270309931736 ) ) ;
#22380 = UNCERTAINTY_MEASURE_WITH_UNIT (LENGTH_MEASURE( 1.000000000000000082E-05 ), #29392, 'distance_accuracy_value', 'NONE');
#22381 = CARTESIAN_POINT ( 'NONE',  ( 123.6310548109119765, -4.153390946401325223, -8.397313243818185668 ) ) ;
#22382 = CARTESIAN_POINT ( 'NONE',  ( 113.9875214775786532, -8.899110576539710493, -16.42337572283490132 ) ) ;
#22383 = ORIENTED_EDGE ( 'NONE', *, *, #30360, .F. ) ;
#22384 = CARTESIAN_POINT ( 'NONE',  ( 122.2437673109119629, -9.289237151508434209, -11.05642687123711276 ) ) ;
#22385 = EDGE_CURVE ( 'NONE', #16955, #22059, #35724, .T. ) ;
#22386 = CARTESIAN_POINT ( 'NONE',  ( 113.6298959279789784, 0.1843591316377651834, -14.64321520033831447 ) ) ;
#22387 = CARTESIAN_POINT ( 'NONE',  ( 117.0507614775786465, 0.1319031606808879209, -14.10382304977623669 ) ) ;
#22388 = VERTEX_POINT ( 'NONE', #43032 ) ;
#22389 = DIRECTION ( 'NONE',  ( 0.000000000000000000, 0.000000000000000000, 1.000000000000000000 ) ) ;
#22390 = CARTESIAN_POINT ( 'NONE',  ( 115.2922348109119781, -10.63000616557722466, -14.87417383870573495 ) ) ;
#22391 = CIRCLE ( 'NONE', #4298, 2.000000000000000444 ) ;
#22392 = CARTESIAN_POINT ( 'NONE',  ( 115.8304577545247582, -7.250697342233347165, -7.631215200338321125 ) ) ;
#22393 = CARTESIAN_POINT ( 'NONE',  ( 112.7962614775786676, -6.222761293078241884, -8.102969835052219238 ) ) ;
#22394 = VERTEX_POINT ( 'NONE', #25708 ) ;
#22395 = EDGE_LOOP ( 'NONE', ( #31067, #12953, #7744, #41468, #27789, #41140 ) ) ;
#22396 = CARTESIAN_POINT ( 'NONE',  ( 122.1561614775786353, -8.899110576539710493, -16.42337572283490132 ) ) ;
#22397 = CARTESIAN_POINT ( 'NONE',  ( 117.8449348109119938, -1.833838273342659253, -17.42832698103878286 ) ) ;
#22398 = CARTESIAN_POINT ( 'NONE',  ( 67.30914723170953096, -61.59348913822725535, -38.73469799600663777 ) ) ;
#22399 = ORIENTED_EDGE ( 'NONE', *, *, #33100, .F. ) ;
#22400 = DIRECTION ( 'NONE',  ( 0.000000000000000000, 0.000000000000000000, 1.000000000000000000 ) ) ;
#22401 = CARTESIAN_POINT ( 'NONE',  ( 71.79922130029189020, -25.12209812792223929, -4.893215200338314474 ) ) ;
#22402 = CARTESIAN_POINT ( 'NONE',  ( 112.0799890045248475, 0.8980012041604421569, -15.77991374673208469 ) ) ;
#22403 = ADVANCED_FACE ( 'NONE', ( #36175 ), #5349, .T. ) ;
#22404 = AXIS2_PLACEMENT_3D ( 'NONE', #44585, #19720, #23609 ) ;
#22405 = CARTESIAN_POINT ( 'NONE',  ( 115.9729548109119861, -6.344957434206662583, -7.627207830600332805 ) ) ;
#22407 = CARTESIAN_POINT ( 'NONE',  ( 114.3846081442453197, 0.4262465694468514643, -12.03445270309931736 ) ) ;
#22406 = CARTESIAN_POINT ( 'NONE',  ( 115.1220548109119761, -8.166667518702817929, -8.995218007635861213 ) ) ;
#22408 = CARTESIAN_POINT ( 'NONE',  ( 120.1707281442453166, -9.565557343593413364, -10.61323700422348004 ) ) ;
#22409 = DIRECTION ( 'NONE',  ( 0.000000000000000000, 1.000000000000000000, 0.000000000000000000 ) ) ;
#22410 = ORIENTED_EDGE ( 'NONE', *, *, #11706, .F. ) ;
#22411 = CARTESIAN_POINT ( 'NONE',  ( 120.3976348109119812, -7.643976991954077427, -18.09477374809248928 ) ) ;
#22412 = CARTESIAN_POINT ( 'NONE',  ( 124.8790414775786246, -8.899110576539710493, -16.42337572283490132 ) ) ;
#22413 = CARTESIAN_POINT ( 'NONE',  ( 111.3160046295247838, -4.863998795839590272, -7.631215200338315796 ) ) ;
#22414 = LINE ( 'NONE', #39293, #43504 ) ;
#22415 = CARTESIAN_POINT ( 'NONE',  ( 110.9687390045248350, 0.8980012041604421569, -15.77991374673208469 ) ) ;
#22416 = CARTESIAN_POINT ( 'NONE',  ( 116.8805814775786445, -6.344957434206662583, -7.627207830600332805 ) ) ;
#22417 = ORIENTED_EDGE ( 'NONE', *, *, #38681, .F. ) ;
#22418 = CARTESIAN_POINT ( 'NONE',  ( 119.6601881442453106, -8.166667518702819706, -8.995218007635861213 ) ) ;
#22419 = DIRECTION ( 'NONE',  ( 0.000000000000000000, 0.6004852223388321697, -0.7996358532186279566 ) ) ;
#22420 = CARTESIAN_POINT ( 'NONE',  ( 109.0240515045248202, -2.477300249445798297, -7.631215200338321125 ) ) ;
#22421 = CARTESIAN_POINT ( 'NONE',  ( 118.0151148109119816, -10.63000616557722466, -14.87417383870573495 ) ) ;
#22422 = B_SPLINE_CURVE_WITH_KNOTS ( 'NONE', 3,
 ( #30095, #33035, #1810, #29639, #44011, #26220, #34173, #41714, #10478, #6602 ),
 .UNSPECIFIED., .F., .F.,
 ( 4, 3, 3, 4 ),
 ( 8.545274078289149956E-18, 0.0002476486541971030086, 0.0004952973025691040062, 0.0009610892161188130988 ),
 .UNSPECIFIED. ) ;
#22423 = CARTESIAN_POINT ( 'NONE',  ( 118.8092881442453290, -9.988377603198976828, -10.36322818467138340 ) ) ;
#22424 = CARTESIAN_POINT ( 'NONE',  ( 46.22412376146323965, -17.17426195654049437, -19.39321520033831447 ) ) ;
#22425 = DIRECTION ( 'NONE',  ( 0.000000000000000000, 0.000000000000000000, 1.000000000000000000 ) ) ;
#22426 = ORIENTED_EDGE ( 'NONE', *, *, #23688, .T. ) ;
#22427 = CARTESIAN_POINT ( 'NONE',  ( 90.48265143217095385, -25.66130191030491758, -14.20063063452593255 ) ) ;
#22428 = CARTESIAN_POINT ( 'NONE',  ( 109.2294419231370597, -10.34583128743581426, -14.16414405063035531 ) ) ;
#22429 = CARTESIAN_POINT ( 'NONE',  ( 120.0005481442453146, -4.153390946401325223, -8.397313243818185668 ) ) ;
#22430 = CARTESIAN_POINT ( 'NONE',  ( 112.1494421295248003, -9.868328341294093420, -13.39321520033831447 ) ) ;
#22431 = CARTESIAN_POINT ( 'NONE',  ( 106.3848327545248651, -2.477300249445798297, -19.15521520033831138 ) ) ;
#22432 = CARTESIAN_POINT ( 'NONE',  ( 113.0798948109119948, -8.899110576539710493, -16.42337572283490132 ) ) ;
#22433 = LINE ( 'NONE', #32683, #41578 ) ;
#22434 = CARTESIAN_POINT ( 'NONE',  ( 68.96715889846213088, -25.99505776776173960, -5.893215200338315363 ) ) ;
#22435 = CARTESIAN_POINT ( 'NONE',  ( 112.6828081442453282, -2.084020599724406786, -8.691656652584148546 ) ) ;
#22436 = CARTESIAN_POINT ( 'NONE',  ( 119.0361948109119652, -7.893985811506177619, -18.51759400769804742 ) ) ;
#22437 = ORIENTED_EDGE ( 'NONE', *, *, #3000, .T. ) ;
#22438 = CARTESIAN_POINT ( 'NONE',  ( 116.8238548109119819, -5.574606645277164318, -18.38911715685844683 ) ) ;
#22439 = CARTESIAN_POINT ( 'NONE',  ( 114.0442481442453300, -1.834011780172310813, -8.268836392978581529 ) ) ;
#22440 = CARTESIAN_POINT ( 'NONE',  ( 122.4397948109119767, -9.988377603198976828, -10.36322818467138340 ) ) ;
#22441 = VECTOR ( 'NONE', #25297, 1000.000000000000114 ) ;
#22442 = CARTESIAN_POINT ( 'NONE',  ( 119.8303681442453126, 0.4262465694468514643, -12.03445270309931736 ) ) ;
#22443 = ORIENTED_EDGE ( 'NONE', *, *, #2184, .T. ) ;
#22444 = CARTESIAN_POINT ( 'NONE',  ( 125.1626748109119802, -0.1624402480850797581, -16.17319339645315424 ) ) ;
#22445 = CARTESIAN_POINT ( 'NONE',  ( 119.6601881442453106, -8.166667518702819706, -8.995218007635861213 ) ) ;
#22446 = CARTESIAN_POINT ( 'NONE',  ( 124.6574308310800916, -5.898449491513396481, -5.630628696673196210 ) ) ;
#22447 = CARTESIAN_POINT ( 'NONE',  ( 122.0994348109119443, 0.9020085738987339008, -11.91225656197089222 ) ) ;
#22448 = CARTESIAN_POINT ( 'NONE',  ( 151.2860562277021472, -1.295815253274133161, -16.89579513612386563 ) ) ;
#22449 = DIRECTION ( 'NONE',  ( -0.000000000000000000, -0.9284778069183721172, -0.3713878862591650232 ) ) ;
#22450 = CARTESIAN_POINT ( 'NONE',  ( 128.0347018188450932, -2.863786252703732771, -14.80791975478640587 ) ) ;
#22451 = CARTESIAN_POINT ( 'NONE',  ( 114.5803015045248117, -6.936859964151250502, -18.39754474579286025 ) ) ;
#22452 = DIRECTION ( 'NONE',  ( -0.000000000000000000, -0.9284778069183721172, -0.3713878862591650232 ) ) ;
#22453 = FACE_OUTER_BOUND ( 'NONE', #26799, .T. ) ;
#22454 = CARTESIAN_POINT ( 'NONE',  ( 116.1431348109119881, 0.1319031606808879209, -14.10382304977623669 ) ) ;
#22455 = CARTESIAN_POINT ( 'NONE',  ( 112.1722681442453222, -8.899110576539710493, -16.42337572283490132 ) ) ;
#22456 = CARTESIAN_POINT ( 'NONE',  ( 95.28169473643895060, -29.55631648666738087, -14.86464107658013845 ) ) ;
#22457 = ORIENTED_EDGE ( 'NONE', *, *, #21430, .T. ) ;
#22458 = CARTESIAN_POINT ( 'NONE',  ( 116.6638952545248031, -9.868328341294098749, -15.46607636864997204 ) ) ;
#22459 = CARTESIAN_POINT ( 'NONE',  ( 111.8021765045248372, -2.791137627527939813, -8.388885654883777576 ) ) ;
#22460 = CARTESIAN_POINT ( 'NONE',  ( 116.5402214775786405, -9.565557343593413364, -10.61323700422348004 ) ) ;
#22461 = CARTESIAN_POINT ( 'NONE',  ( 113.6680897606643441, -2.236191541394345172, -18.14152338500401029 ) ) ;
#22462 = CARTESIAN_POINT ( 'NONE',  ( 119.1871698793805194, -2.191907684172563986, -18.20049396185734025 ) ) ;
#22463 = DIRECTION ( 'NONE',  ( 0.000000000000000000, -0.9242245927363041957, -0.3818493186865896671 ) ) ;
#22465 = CARTESIAN_POINT ( 'NONE',  ( 124.2550481442452792, -9.988377603198980381, -10.36322818467138518 ) ) ;
#22464 = CARTESIAN_POINT ( 'NONE',  ( 66.21645592411296377, -14.64013927798640502, -10.27431999848409028 ) ) ;
#22466 = CARTESIAN_POINT ( 'NONE',  ( 122.5532481442453019, 0.4262465694468514643, -12.03445270309931736 ) ) ;
#22467 = ORIENTED_EDGE ( 'NONE', *, *, #44574, .F. ) ;
#22468 = DIRECTION ( 'NONE',  ( -0.1352586133457950590, -0.9908103287288504424, 0.000000000000000000 ) ) ;
#22469 = LINE ( 'NONE', #12448, #19495 ) ;
#22470 = CARTESIAN_POINT ( 'NONE',  ( 107.9822546295247889, -4.863998795839590272, -18.39754474579285315 ) ) ;
#22471 = CARTESIAN_POINT ( 'NONE',  ( 124.2550481442452792, -0.1624402480850797581, -16.17319339645315424 ) ) ;
#22472 = EDGE_CURVE ( 'NONE', #41351, #13898, #33720, .T. ) ;
#22473 = CARTESIAN_POINT ( 'NONE',  ( 121.5321681442453183, -0.1624402480850797581, -16.17319339645315424 ) ) ;
#22474 = CARTESIAN_POINT ( 'NONE',  ( 114.6682414775786469, -7.894159318335828068, -9.358103419637847864 ) ) ;
#22475 = FACE_OUTER_BOUND ( 'NONE', #40176, .T. ) ;
#22476 = CARTESIAN_POINT ( 'NONE',  ( 107.4266296295248821, -4.863998795839590272, -19.15521520033831493 ) ) ;
#22477 = CARTESIAN_POINT ( 'NONE',  ( 123.2906948109119867, -1.833838273342659697, -17.42832698103878286 ) ) ;
#22478 = CARTESIAN_POINT ( 'NONE',  ( 122.7801548109119665, -6.222761293078241884, -8.102969835052219238 ) ) ;
#22479 = DIRECTION ( 'NONE',  ( 0.000000000000000000, 0.000000000000000000, -1.000000000000000000 ) ) ;
#22480 = DIRECTION ( 'NONE',  ( 0.000000000000000000, 0.9284778069183718952, 0.3713878862591650232 ) ) ;
#22481 = CARTESIAN_POINT ( 'NONE',  ( 114.2330358795247776, -0.7896495226426338832, -17.46756447353520159 ) ) ;
#22482 = DIRECTION ( 'NONE',  ( 0.8636456077245092677, -0.5040994586965584778, 0.000000000000000000 ) ) ;
#22483 = CARTESIAN_POINT ( 'NONE',  ( 83.86641712191145359, -31.75150836541887145, -22.59176852388810630 ) ) ;
#22484 = CARTESIAN_POINT ( 'NONE',  ( 119.7736414775786358, -10.30919188438810075, -12.61870101168855918 ) ) ;
#22485 = CARTESIAN_POINT ( 'NONE',  ( 118.6958348109119754, -6.344957434206665248, -7.627207830600338134 ) ) ;
#22486 = CARTESIAN_POINT ( 'NONE',  ( 106.5931921295248372, 0.8980012041604618078, -13.39321520033831447 ) ) ;
#22487 = CARTESIAN_POINT ( 'NONE',  ( 116.9940348109119839, -9.988377603198976828, -10.36322818467138340 ) ) ;
#22488 = FACE_BOUND ( 'NONE', #788, .T. ) ;
#22489 = ORIENTED_EDGE ( 'NONE', *, *, #16802, .F. ) ;
#22490 = CARTESIAN_POINT ( 'NONE',  ( 116.3892577545247491, -6.935066607705044461, -8.393215200338321580 ) ) ;
#22491 = CARTESIAN_POINT ( 'NONE',  ( 120.3409081442453044, -0.4660016031367893996, -10.09054647747474043 ) ) ;
#22492 = CARTESIAN_POINT ( 'NONE',  ( 124.8223148109119762, -10.15424416112533912, -14.75197769757731336 ) ) ;
#22493 = DIRECTION ( 'NONE',  ( 0.000000000000000000, 0.000000000000000000, 1.000000000000000000 ) ) ;
#22494 = CARTESIAN_POINT ( 'NONE',  ( 114.5547881442453217, -4.153390946401321671, -8.397313243818183892 ) ) ;
#22495 = CARTESIAN_POINT ( 'NONE',  ( 111.9453614775786434, -7.894159318335828068, -9.358103419637847864 ) ) ;
#22496 = EDGE_CURVE ( 'NONE', #19765, #45054, #961, .T. ) ;
#22497 = CARTESIAN_POINT ( 'NONE',  ( 109.3713171295247832, -10.62599879583958540, -13.39321520033831447 ) ) ;
#22498 = VECTOR ( 'NONE', #11337, 1000.000000000000000 ) ;
#22499 = CARTESIAN_POINT ( 'NONE',  ( 119.6601881442453106, -1.833838273342659253, -17.42832698103878286 ) ) ;
#22500 = CARTESIAN_POINT ( 'NONE',  ( 116.7819514645520940, -3.568899806858861101, -18.41715839113304298 ) ) ;
#22501 = DIRECTION ( 'NONE',  ( 0.000000000000000000, -0.3818493186865927203, 0.9242245927363029745 ) ) ;
#22502 = ORIENTED_EDGE ( 'NONE', *, *, #29788, .F. ) ;
#22503 = EDGE_CURVE ( 'NONE', #28262, #24082, #12480, .T. ) ;
#22504 = CARTESIAN_POINT ( 'NONE',  ( 67.30914723170953096, -53.02970208888985582, -35.30921302810730111 ) ) ;
#22505 = ADVANCED_FACE ( 'NONE', ( #40055 ), #12257, .T. ) ;
#22506 = CARTESIAN_POINT ( 'NONE',  ( 122.8368814775786291, -1.561330072975668948, -17.79121239304076951 ) ) ;
#22507 = DIRECTION ( 'NONE',  ( 0.000000000000000000, 0.000000000000000000, 1.000000000000000000 ) ) ;
#22508 = CARTESIAN_POINT ( 'NONE',  ( 64.97240540738540915, -2.563123825349247209, -8.300243185318032957 ) ) ;
#22509 = CARTESIAN_POINT ( 'NONE',  ( 117.6747548109119919, -7.643976991954077427, -18.09477374809248928 ) ) ;
#22510 = CARTESIAN_POINT ( 'NONE',  ( 112.1722681442453222, -0.4660016031367893996, -10.09054647747474043 ) ) ;
#22511 = CARTESIAN_POINT ( 'NONE',  ( 64.18561586838816879, -35.08338226378547375, -5.893215200338315363 ) ) ;
#22512 = CARTESIAN_POINT ( 'NONE',  ( 122.2696148109119889, -5.574606645277164318, -18.38911715685844683 ) ) ;
#22513 = CARTESIAN_POINT ( 'NONE',  ( 109.5990301496069748, 0.3591747506842615789, -14.64321520033828605 ) ) ;
#22514 = CARTESIAN_POINT ( 'NONE',  ( 124.5954081442453116, -6.222761293078241884, -8.102969835052219238 ) ) ;
#22515 = CARTESIAN_POINT ( 'NONE',  ( 125.3282169345246189, -11.52192247331090158, -15.89464684586357279 ) ) ;
#22516 = CARTESIAN_POINT ( 'NONE',  ( 121.7590748109119687, -7.893985811506177619, -18.51759400769804742 ) ) ;
#22517 = CARTESIAN_POINT ( 'NONE',  ( 118.4689281442453250, -10.15424416112533912, -14.75197769757731336 ) ) ;
#22518 = CARTESIAN_POINT ( 'NONE',  ( 124.7655881442452852, -9.859900752359378018, -12.68260735090039759 ) ) ;
#22519 = ADVANCED_FACE ( 'NONE', ( #40745 ), #18449, .T. ) ;
#22520 = CARTESIAN_POINT ( 'NONE',  ( 118.1852948109119836, -5.638512984488999180, -18.83840828888717311 ) ) ;
#22521 = CARTESIAN_POINT ( 'NONE',  ( 115.4056881442453459, -7.893985811506177619, -18.51759400769804742 ) ) ;
#22522 = CARTESIAN_POINT ( 'NONE',  ( 115.8304577545247582, -2.791137627527939813, -18.39754474579286025 ) ) ;
#22523 = EDGE_CURVE ( 'NONE', #3446, #21884, #39838, .T. ) ;
#22524 = EDGE_CURVE ( 'NONE', #20631, #29947, #2861, .T. ) ;
#22525 = CARTESIAN_POINT ( 'NONE',  ( 123.5176014775786228, -0.8288870151387760510, -10.36305467784173118 ) ) ;
#22526 = ORIENTED_EDGE ( 'NONE', *, *, #37026, .F. ) ;
#22527 = CARTESIAN_POINT ( 'NONE',  ( 119.3198281442452924, 0.5811942927096110934, -14.16772938898807510 ) ) ;
#22528 = CARTESIAN_POINT ( 'NONE',  ( 116.5944421295247793, 0.8980012041604618078, -13.39321520033831447 ) ) ;
#22529 = CARTESIAN_POINT ( 'NONE',  ( 108.1211608795247798, -1.325403438956436419, -16.93181055722141792 ) ) ;
#22530 = DIRECTION ( 'NONE',  ( 0.000000000000000000, -0.6004852223388319477, 0.7996358532186282897 ) ) ;
#22531 = CARTESIAN_POINT ( 'NONE',  ( 114.0442481442453300, -7.643976991954077427, -18.09477374809248928 ) ) ;
#22532 = CARTESIAN_POINT ( 'NONE',  ( 69.36136150295220659, -101.1685209014307674, -50.56525720990386219 ) ) ;
#22533 = CARTESIAN_POINT ( 'NONE',  ( 124.3117748109119844, -10.30919188438810075, -12.61870101168855918 ) ) ;
#22534 = ORIENTED_EDGE ( 'NONE', *, *, #41606, .F. ) ;
#22535 = CIRCLE ( 'NONE', #1406, 1.610000000000000986 ) ;
#22536 = CARTESIAN_POINT ( 'NONE',  ( 123.5176014775786228, -0.8288870151387760510, -10.36305467784173118 ) ) ;
#22537 = CARTESIAN_POINT ( 'NONE',  ( 123.1466579359119891, -5.444069387712269226, -19.60292469916370450 ) ) ;
#22538 = CARTESIAN_POINT ( 'NONE',  ( 120.2990798109119766, -2.173413727453600508, -8.297982527556802879 ) ) ;
#22539 = CARTESIAN_POINT ( 'NONE',  ( 112.0126281442453120, -9.814174330883659536, -12.68911139247490105 ) ) ;
#22540 = CARTESIAN_POINT ( 'NONE',  ( 109.5796765045248122, -2.791137627527939813, -8.388885654883777576 ) ) ;
#22541 = ORIENTED_EDGE ( 'NONE', *, *, #43404, .F. ) ;
#22542 = CARTESIAN_POINT ( 'NONE',  ( 113.2500748109119968, -6.344957434206662583, -7.627207830600332805 ) ) ;
#22543 = CARTESIAN_POINT ( 'NONE',  ( 88.56442385468598388, -11.33890518539517522, -13.97496118938472698 ) ) ;
#22544 = CARTESIAN_POINT ( 'NONE',  ( 122.8368814775786291, -7.894159318335828068, -9.358103419637847864 ) ) ;
#22545 = CARTESIAN_POINT ( 'NONE',  ( 115.0086014775786509, -5.574606645277164318, -18.38911715685844683 ) ) ;
#22546 = CARTESIAN_POINT ( 'NONE',  ( 116.0086969107182142, -2.467220198592777525, -17.83387418641524391 ) ) ;
#22547 = LINE ( 'NONE', #8869, #6258 ) ;
#22548 = CARTESIAN_POINT ( 'NONE',  ( 115.7460481442453357, 0.9020085738987339008, -11.91225656197089222 ) ) ;
#22549 = CARTESIAN_POINT ( 'NONE',  ( 111.4549108795247747, -1.325403438956436419, -16.93181055722141792 ) ) ;
#22550 = CARTESIAN_POINT ( 'NONE',  ( 124.0848681442452772, -4.089484607189486809, -7.948022111789456723 ) ) ;
#22551 = B_SPLINE_CURVE_WITH_KNOTS ( 'NONE', 3,
 ( #35503, #38703, #18193, #7470, #21838, #10471, #13882, #35270, #21388, #27793 ),
 .UNSPECIFIED., .F., .F.,
 ( 4, 3, 3, 4 ),
 ( 0.000000000000000000, 0.0001671877548681299829, 0.0003343755096277750216, 0.0006463528481650629171 ),
 .UNSPECIFIED. ) ;
#22552 = DIRECTION ( 'NONE',  ( -1.000000000000000000, 0.000000000000000000, 0.000000000000000000 ) ) ;
#22553 = ORIENTED_EDGE ( 'NONE', *, *, #9845, .F. ) ;
#22554 = CARTESIAN_POINT ( 'NONE',  ( 115.2922348109119781, -10.63000616557722466, -14.87417383870573495 ) ) ;
#22555 = CARTESIAN_POINT ( 'NONE',  ( 111.9453614775786434, -7.894159318335828068, -9.358103419637847864 ) ) ;
#22556 = CARTESIAN_POINT ( 'NONE',  ( 68.07789357685331311, -68.58957386525776201, -38.44539312525988350 ) ) ;
#22557 = CARTESIAN_POINT ( 'NONE',  ( 112.0020881442453344, 0.2603800115204892296, -16.42320221600525088 ) ) ;
#22558 = ORIENTED_EDGE ( 'NONE', *, *, #36467, .F. ) ;
#22559 = CARTESIAN_POINT ( 'NONE',  ( 118.5256548109119876, -0.4660016031367893996, -10.09054647747474043 ) ) ;
#22560 = AXIS2_PLACEMENT_3D ( 'NONE', #13959, #20801, #487 ) ;
#22561 = FACE_OUTER_BOUND ( 'NONE', #44956, .T. ) ;
#22562 = CARTESIAN_POINT ( 'NONE',  ( 109.4644545411903209, -0.3595008806742185925, -10.82052240173742419 ) ) ;
#22563 = CARTESIAN_POINT ( 'NONE',  ( 111.6050014775786536, 0.1319031606808879209, -14.10382304977624379 ) ) ;
#22564 = CARTESIAN_POINT ( 'NONE',  ( 136.1673833308556993, -2.578395149234233852, -7.983002144439000247 ) ) ;
#22565 = CARTESIAN_POINT ( 'NONE',  ( 113.8740681442453138, -9.859900752359374465, -12.68260735090039404 ) ) ;
#22566 = DIRECTION ( 'NONE',  ( 0.000000000000000000, 0.000000000000000000, 1.000000000000000000 ) ) ;
#22567 = VECTOR ( 'NONE', #35476, 1000.000000000000000 ) ;
#22568 = CARTESIAN_POINT ( 'NONE',  ( 125.2180320564445282, -1.939873832223439898, -20.09786755395826674 ) ) ;
#22569 = CARTESIAN_POINT ( 'NONE',  ( 113.9307948109119764, -10.15424416112533912, -14.75197769757731336 ) ) ;
#22570 = AXIS2_PLACEMENT_3D ( 'NONE', #22630, #21961, #42497 ) ;
#22571 = CARTESIAN_POINT ( 'NONE',  ( 113.4769814775786330, -10.63000616557722466, -14.87417383870573495 ) ) ;
#22572 = CARTESIAN_POINT ( 'NONE',  ( 116.6670768749042821, -8.779456523914790367, -16.62141271327601899 ) ) ;
#22573 = CARTESIAN_POINT ( 'NONE',  ( 123.4041481442452834, 0.1319031606808879209, -14.10382304977623669 ) ) ;
#22574 = CARTESIAN_POINT ( 'NONE',  ( 112.1722681442453222, -8.899110576539710493, -16.42337572283490132 ) ) ;
#22575 = CARTESIAN_POINT ( 'NONE',  ( 122.4397948109119767, -9.988377603198976828, -10.36322818467138340 ) ) ;
#22576 = EDGE_CURVE ( 'NONE', #12871, #10499, #38133, .T. ) ;
#22577 = CARTESIAN_POINT ( 'NONE',  ( 122.3263414775786373, -6.344957434206665248, -7.627207830600338134 ) ) ;
#22578 = EDGE_LOOP ( 'NONE', ( #5708, #29007, #14123, #2597, #29451 ) ) ;
#22579 = CARTESIAN_POINT ( 'NONE',  ( 127.2313854076963509, -8.461403773221835678, -17.56217400450200472 ) ) ;
#22580 = CARTESIAN_POINT ( 'NONE',  ( 110.2047546295247855, -4.863998795839590272, -7.631215200338315796 ) ) ;
#22581 = CARTESIAN_POINT ( 'NONE',  ( 109.5102233795247884, -1.325403438956436419, -9.854619843455211026 ) ) ;
#22582 = CARTESIAN_POINT ( 'NONE',  ( 109.5102233795247884, -1.325403438956436419, -9.854619843455211026 ) ) ;
#22583 = EDGE_CURVE ( 'NONE', #10303, #30977, #24173, .T. ) ;
#22584 = CARTESIAN_POINT ( 'NONE',  ( 126.9276200068699723, -9.934318824270198078, -11.67164607367653417 ) ) ;
#22585 = CARTESIAN_POINT ( 'NONE',  ( 116.7104014775786425, -0.4660016031367893996, -10.09054647747474043 ) ) ;
#22586 = ORIENTED_EDGE ( 'NONE', *, *, #26511, .F. ) ;
#22587 = CARTESIAN_POINT ( 'NONE',  ( 108.0517077545248696, -7.250697342233347165, -7.631215200338321125 ) ) ;
#22588 = DIRECTION ( 'NONE',  ( 0.000000000000000000, 0.000000000000000000, 1.000000000000000000 ) ) ;
#22589 = ADVANCED_FACE ( 'NONE', ( #43940 ), #12936, .F. ) ;
#22590 = CARTESIAN_POINT ( 'NONE',  ( 115.9729548109119861, -3.505236298600246325, -18.68346056562440793 ) ) ;
#22591 = CARTESIAN_POINT ( 'NONE',  ( 119.7434548109119703, -13.11073630560948722, -15.94021774473354114 ) ) ;
#22592 = CARTESIAN_POINT ( 'NONE',  ( 118.0718414775786300, -9.261995988541697145, -16.69588392320189030 ) ) ;
#22593 = CARTESIAN_POINT ( 'NONE',  ( 109.0935046295247872, -4.863998795839590272, -7.631215200338315796 ) ) ;
#22594 = CARTESIAN_POINT ( 'NONE',  ( 71.37572422742091760, -11.86958442233774313, -21.39321520033831447 ) ) ;
#22595 = ORIENTED_EDGE ( 'NONE', *, *, #33629, .T. ) ;
#22596 = CARTESIAN_POINT ( 'NONE',  ( 127.7184548109119788, -4.683672500039348208, -14.88233656108870662 ) ) ;
#22597 = CARTESIAN_POINT ( 'NONE',  ( 119.3765548109119834, -10.15424416112533912, -14.75197769757731336 ) ) ;
#22598 = CARTESIAN_POINT ( 'NONE',  ( 115.2922348109119781, -10.63000616557722466, -14.87417383870573495 ) ) ;
#22599 = CIRCLE ( 'NONE', #43008, 2.000000000000000444 ) ;
#22600 = CARTESIAN_POINT ( 'NONE',  ( 116.5402214775786405, 0.2603800115204892296, -16.42320221600525088 ) ) ;
#22601 = CARTESIAN_POINT ( 'NONE',  ( 46.84966980880212617, -19.07391775237791620, -19.39321520033831447 ) ) ;
#22602 = CARTESIAN_POINT ( 'NONE',  ( 122.7801548109119665, -6.222761293078241884, -8.102969835052219238 ) ) ;
#22603 = CARTESIAN_POINT ( 'NONE',  ( 117.9016614775786280, -0.1624402480850797581, -16.17319339645315424 ) ) ;
#22604 = VERTEX_POINT ( 'NONE', #5397 ) ;
#22605 = CARTESIAN_POINT ( 'NONE',  ( 120.8547048109119686, -7.554583864224885481, -18.48844787311982785 ) ) ;
#22606 = CIRCLE ( 'NONE', #33521, 8.000000000000001776 ) ;
#22607 = CARTESIAN_POINT ( 'NONE',  ( 114.2144281442453178, -8.166667518702817929, -8.995218007635859436 ) ) ;
#22608 = CARTESIAN_POINT ( 'NONE',  ( 118.5256548109119876, -8.899110576539710493, -16.42337572283490132 ) ) ;
#22609 = ORIENTED_EDGE ( 'NONE', *, *, #11114, .F. ) ;
#22610 = AXIS2_PLACEMENT_3D ( 'NONE', #33092, #2317, #1861 ) ;
#22611 = PLANE ( 'NONE',  #42762 ) ;
#22612 = CARTESIAN_POINT ( 'NONE',  ( 114.1009748109119784, -4.089484607189486809, -7.948022111789456723 ) ) ;
#22613 = CARTESIAN_POINT ( 'NONE',  ( 115.7610046295247912, -4.863998795839590272, -7.631215200338315796 ) ) ;
#22614 = DIRECTION ( 'NONE',  ( -0.6836572958096076569, 0.7298031939408696767, 0.000000000000000000 ) ) ;
#22615 = ORIENTED_EDGE ( 'NONE', *, *, #22638, .T. ) ;
#22616 = EDGE_LOOP ( 'NONE', ( #39737, #27725, #27153, #21197 ) ) ;
#22617 = CARTESIAN_POINT ( 'NONE',  ( 120.5678148109119832, -1.833838273342659253, -17.42832698103878286 ) ) ;
#22618 = CARTESIAN_POINT ( 'NONE',  ( 120.9081748109119872, -4.153390946401325223, -8.397313243818185668 ) ) ;
#22619 = LINE ( 'NONE', #8495, #43287 ) ;
#22620 = EDGE_CURVE ( 'NONE', #34510, #13487, #14109, .T. ) ;
#22621 = EDGE_LOOP ( 'NONE', ( #28348, #17385, #12413, #41797, #849 ) ) ;
#22622 = DIRECTION ( 'NONE',  ( -1.000000000000000000, 0.000000000000000000, 0.000000000000000000 ) ) ;
#22623 = DIRECTION ( 'NONE',  ( -0.9908103287288505534, 0.1352586133457950313, 0.000000000000000000 ) ) ;
#22624 = CARTESIAN_POINT ( 'NONE',  ( 106.7320983795247855, -0.7896495226426338832, -9.318865927141430916 ) ) ;
#22625 = AXIS2_PLACEMENT_3D ( 'NONE', #4973, #8630, #1327 ) ;
#22626 = CARTESIAN_POINT ( 'NONE',  ( 116.2565881442452991, -9.261995988541697145, -16.69588392320189030 ) ) ;
#22628 = CARTESIAN_POINT ( 'NONE',  ( 115.2922348109119781, 0.4262465694468514643, -12.03445270309931736 ) ) ;
#22627 = CARTESIAN_POINT ( 'NONE',  ( 113.9875214775786532, -0.4660016031367893996, -10.09054647747474043 ) ) ;
#22629 = CARTESIAN_POINT ( 'NONE',  ( 120.7947214775786193, -0.8288870151387760510, -10.36305467784173118 ) ) ;
#22630 = CARTESIAN_POINT ( 'NONE',  ( 70.19189222814998175, -62.62292920857806422, -38.25196254438899501 ) ) ;
#22631 = ORIENTED_EDGE ( 'NONE', *, *, #19192, .T. ) ;
#22632 = CARTESIAN_POINT ( 'NONE',  ( 120.8514481442452961, -2.084020599724406786, -8.691656652584148546 ) ) ;
#22633 = CARTESIAN_POINT ( 'NONE',  ( 123.5176014775786228, -0.8288870151387760510, -10.36305467784173118 ) ) ;
#22634 = CARTESIAN_POINT ( 'NONE',  ( 110.8298327545248299, -2.477300249445798297, -19.15521520033831138 ) ) ;
#22635 = VECTOR ( 'NONE', #10430, 999.9999999999998863 ) ;
#22636 = DIRECTION ( 'NONE',  ( 1.000000000000000000, 0.000000000000000000, -0.000000000000000000 ) ) ;
#22637 = CARTESIAN_POINT ( 'NONE',  ( 112.4272546295247821, -4.863998795839590272, -7.631215200338315796 ) ) ;
#22638 = EDGE_CURVE ( 'NONE', #29032, #36176, #41798, .T. ) ;
#22639 = CARTESIAN_POINT ( 'NONE',  ( 116.9373081442452929, -8.166667518702817929, -8.995218007635861213 ) ) ;
#22640 = ORIENTED_EDGE ( 'NONE', *, *, #18912, .T. ) ;
#22641 = CIRCLE ( 'NONE', #32100, 0.3000000000000022093 ) ;
#22642 = CARTESIAN_POINT ( 'NONE',  ( 119.4332814775786318, -0.4660016031367893996, -10.09054647747474043 ) ) ;
#22643 = CARTESIAN_POINT ( 'NONE',  ( 62.99487470011365531, -37.68830414585190169, -5.018140281204638953 ) ) ;
#22644 = CARTESIAN_POINT ( 'NONE',  ( 108.5378796295247810, -4.863998795839590272, -19.15521520033831493 ) ) ;
#22645 = CARTESIAN_POINT ( 'NONE',  ( 117.3911214775786505, -1.561330072975668504, -17.79121239304076951 ) ) ;
#22646 = CARTESIAN_POINT ( 'NONE',  ( 117.8449348109119938, -8.166667518702817929, -8.995218007635861213 ) ) ;
#22647 = CARTESIAN_POINT ( 'NONE',  ( 111.2751814775786556, -7.618532446445550832, -18.05174138884716939 ) ) ;
#22648 = CARTESIAN_POINT ( 'NONE',  ( 116.5432357643689727, -11.91225050823456755, -6.526147773411142161 ) ) ;
#22649 = ORIENTED_EDGE ( 'NONE', *, *, #2480, .T. ) ;
#22650 = CARTESIAN_POINT ( 'NONE',  ( -2.081610404626085042, -6.909071579789481277, -7.809159120385307240 ) ) ;
#22651 = CARTESIAN_POINT ( 'NONE',  ( 109.2294422610953291, -10.06140057338842020, -15.16114099083124778 ) ) ;
#22652 = CARTESIAN_POINT ( 'NONE',  ( 120.7947214775786193, -0.8288870151387760510, -10.36305467784173118 ) ) ;
#22653 = CARTESIAN_POINT ( 'NONE',  ( 110.9687390045248350, -9.868328341294098749, -11.32035403202665869 ) ) ;
#22654 = CARTESIAN_POINT ( 'NONE',  ( 114.5803015045248117, -6.936859964151250502, -18.39754474579286025 ) ) ;
#22655 = CARTESIAN_POINT ( 'NONE',  ( 119.2063748109119814, -7.894159318335828068, -9.358103419637847864 ) ) ;
#22656 = CARTESIAN_POINT ( 'NONE',  ( 69.36136150295220659, -53.68777669040021294, -31.57312503490508604 ) ) ;
#22657 = CARTESIAN_POINT ( 'NONE',  ( 69.18853725737697857, -25.71063077209354120, -5.871568482255375976 ) ) ;
#22658 = CARTESIAN_POINT ( 'NONE',  ( 112.5693548109119888, 0.4262465694468514643, -12.03445270309931736 ) ) ;
#22659 = CARTESIAN_POINT ( 'NONE',  ( 121.3052614775786111, -1.834011780172310813, -8.268836392978581529 ) ) ;
#22660 = VERTEX_POINT ( 'NONE', #22954 ) ;
#22661 = CARTESIAN_POINT ( 'NONE',  ( 120.3409081442453044, -8.899110576539710493, -16.42337572283490132 ) ) ;
#22662 = CARTESIAN_POINT ( 'NONE',  ( 116.4267681442453153, -3.383040157471821630, -19.15922257007629170 ) ) ;
#22663 = VECTOR ( 'NONE', #23738, 1000.000000000000000 ) ;
#22664 = CARTESIAN_POINT ( 'NONE',  ( 120.3976348109119812, -1.834011780172310813, -8.268836392978581529 ) ) ;
#22665 = CARTESIAN_POINT ( 'NONE',  ( 118.4689281442453250, -10.15424416112533912, -14.75197769757731336 ) ) ;
#22666 = EDGE_LOOP ( 'NONE', ( #14440, #5062, #13520, #18129, #10647, #38378, #29063, #34068, #37989, #7348, #7679, #19796, #29270, #21432, #3537, #25378 ) ) ;
#22667 = CARTESIAN_POINT ( 'NONE',  ( 125.5030348109119558, -6.222761293078241884, -8.102969835052219238 ) ) ;
#22668 = VECTOR ( 'NONE', #11661, 1000.000000000000114 ) ;
#22669 = CARTESIAN_POINT ( 'NONE',  ( 120.8514481442452961, -7.893985811506177619, -18.51759400769804742 ) ) ;
#22670 = CARTESIAN_POINT ( 'NONE',  ( 125.0532895624264569, -6.048765590996615593, -5.961678590775178144 ) ) ;
#22671 = CARTESIAN_POINT ( 'NONE',  ( 124.6521348109119884, -1.561330072975668948, -17.79121239304076951 ) ) ;
#22672 = CARTESIAN_POINT ( 'NONE',  ( 107.1488171295247867, -10.62599879583958540, -13.39321520033831447 ) ) ;
#22673 = CARTESIAN_POINT ( 'NONE',  ( 120.7157985609119635, -0.08252387247370887580, -11.91645802438286417 ) ) ;
#22674 = CARTESIAN_POINT ( 'NONE',  ( 137.4462468446473338, -1.251634937223135013, -16.95462783242788518 ) ) ;
#22675 = CARTESIAN_POINT ( 'NONE',  ( 107.2182702545248105, 0.1403307496149616695, -11.32035403202665336 ) ) ;
#22676 = DIRECTION ( 'NONE',  ( 0.000000000000000000, 1.000000000000000000, 0.000000000000000000 ) ) ;
#22677 = CARTESIAN_POINT ( 'NONE',  ( 136.8611794030155409, -10.05647304890296212, -11.41738541814965124 ) ) ;
#22678 = CARTESIAN_POINT ( 'NONE',  ( 119.7169148109119874, -0.1624402480850797581, -16.17319339645315424 ) ) ;
#22679 = CARTESIAN_POINT ( 'NONE',  ( 125.8433948109119456, -1.834011780172310813, -8.268836392978581529 ) ) ;
#22680 = CARTESIAN_POINT ( 'NONE',  ( 64.49285160086900248, -13.07967021556595100, -15.54970782244410010 ) ) ;
#22681 = ORIENTED_EDGE ( 'NONE', *, *, #26130, .T. ) ;
#22682 = DIRECTION ( 'NONE',  ( 0.000000000000000000, 1.387778780781444413E-14, -1.000000000000000000 ) ) ;
#22683 = CARTESIAN_POINT ( 'NONE',  ( 112.4967077545247633, -2.791137627527939813, -18.39754474579286025 ) ) ;
#22684 = CARTESIAN_POINT ( 'NONE',  ( 116.8238548109119819, -5.574606645277164318, -18.38911715685844683 ) ) ;
#22685 = CARTESIAN_POINT ( 'NONE',  ( 121.9470836909669913, -25.99489077589524300, -13.39321520033831447 ) ) ;
#22687 = CIRCLE ( 'NONE', #19769, 0.5000000000000004441 ) ;
#22686 = CARTESIAN_POINT ( 'NONE',  ( 65.94404352776260225, -0.1671492176496161552, -10.39321520033831625 ) ) ;
#22688 = CARTESIAN_POINT ( 'NONE',  ( -2.434349165179547914, -7.015039675730945667, -19.23631625773906961 ) ) ;
#22690 = CARTESIAN_POINT ( 'NONE',  ( 124.5954081442453116, -3.383040157471821630, -19.15922257007629170 ) ) ;
#22689 = DIRECTION ( 'NONE',  ( -0.9387755102040796773, 0.3445294493088653653, 0.000000000000000000 ) ) ;
#22691 = ADVANCED_FACE ( 'NONE', ( #12027 ), #21501, .T. ) ;
#22692 = CARTESIAN_POINT ( 'NONE',  ( 123.9714148109119805, -8.899110576539710493, -16.42337572283490132 ) ) ;
#22693 = ORIENTED_EDGE ( 'NONE', *, *, #19023, .F. ) ;
#22694 = CARTESIAN_POINT ( 'NONE',  ( 96.54708369096698561, -27.78532125115470208, -14.69016690077367926 ) ) ;
#22695 = CARTESIAN_POINT ( 'NONE',  ( 126.2184548109120072, 0.08211594521788213863, -14.12586826872868961 ) ) ;
#22696 = CARTESIAN_POINT ( 'NONE',  ( 109.7185827545247889, -6.936859964151250502, -8.388885654883777576 ) ) ;
#22697 =( BOUNDED_CURVE ( )  B_SPLINE_CURVE ( 2, ( #42152, #38705, #7472, #31644, #3608, #31422, #187 ),
 .UNSPECIFIED., .F., .F. ) 
 B_SPLINE_CURVE_WITH_KNOTS ( ( 3, 2, 2, 3 ),
 ( 0.4999999999999819589, 0.6249999999999900080, 0.7500000000000000000, 0.7837465698629629829 ),
 .UNSPECIFIED. ) 
 CURVE ( )  GEOMETRIC_REPRESENTATION_ITEM ( )  RATIONAL_B_SPLINE_CURVE ( ( 1.000000000000000000, 0.9238795325112759693, 1.000000000000000000, 0.9238795325112869605, 1.000000000000000000, 0.9794495626071260119, 0.9699952335533410519 ) ) 
 REPRESENTATION_ITEM ( '' )  );
#22698 = CARTESIAN_POINT ( 'NONE',  ( 123.1205148109119563, -7.643976991954077427, -18.09477374809248928 ) ) ;
#22699 = CARTESIAN_POINT ( 'NONE',  ( 119.0929214775786278, -4.153390946401325223, -8.397313243818185668 ) ) ;
#22700 = CARTESIAN_POINT ( 'NONE',  ( 125.0849378844218478, 1.217985041202279461, -17.76587250167452936 ) ) ;
#22701 = CARTESIAN_POINT ( 'NONE',  ( 107.4960827545248350, -2.477300249445798297, -19.15521520033831138 ) ) ;
#22702 = DIRECTION ( 'NONE',  ( 0.000000000000000000, -1.000000000000000000, 0.000000000000000000 ) ) ;
#22703 = CARTESIAN_POINT ( 'NONE',  ( -13.50764450192301602, -4.858897168674483069, -8.690106464020692201 ) ) ;
#22704 = CARTESIAN_POINT ( 'NONE',  ( 110.2047546295247855, -4.863998795839590272, -7.631215200338315796 ) ) ;
#22705 = CARTESIAN_POINT ( 'NONE',  ( -13.52723683684260614, -4.833109925824063957, -18.06246285863358736 ) ) ;
#22706 = CARTESIAN_POINT ( 'NONE',  ( 82.42940256598244275, -31.76384415549768292, -22.80862274410626256 ) ) ;
#22707 = CARTESIAN_POINT ( 'NONE',  ( 120.9649014775786355, -3.383040157471821630, -19.15922257007629170 ) ) ;
#22708 = CARTESIAN_POINT ( 'NONE',  ( 117.4478481442453131, 0.2603800115204892296, -16.42320221600525088 ) ) ;
#22709 = FACE_OUTER_BOUND ( 'NONE', #37499, .T. ) ;
#22710 = CARTESIAN_POINT ( 'NONE',  ( 116.2565881442452991, -9.261995988541697145, -16.69588392320189030 ) ) ;
#22711 = CARTESIAN_POINT ( 'NONE',  ( 124.5203963484541703, -8.366382308237135135, -17.30601432669995532 ) ) ;
#22712 = ORIENTED_EDGE ( 'NONE', *, *, #26957, .F. ) ;
#22713 = DIRECTION ( 'NONE',  ( 0.9609149988134837450, -0.1028163501681639419, 0.2570431154366518145 ) ) ;
#22714 = CARTESIAN_POINT ( 'NONE',  ( 122.7234281442452755, -5.638512984488999180, -18.83840828888717311 ) ) ;
#22715 = CARTESIAN_POINT ( 'NONE',  ( 121.3052614775786111, -1.834011780172310813, -8.268836392978581529 ) ) ;
#22716 = CARTESIAN_POINT ( 'NONE',  ( 125.7866681442452688, -8.899110576539710493, -16.42337572283490132 ) ) ;
#22717 = CARTESIAN_POINT ( 'NONE',  ( 114.4980614775786734, -2.084020599724406786, -8.691656652584148546 ) ) ;
#22718 = CARTESIAN_POINT ( 'NONE',  ( 124.7655881442452852, 0.5811942927096110934, -14.16772938898807510 ) ) ;
#22719 = CARTESIAN_POINT ( 'NONE',  ( 107.1488171295247867, -10.62599879583958540, -13.39321520033831447 ) ) ;
#22720 = CARTESIAN_POINT ( 'NONE',  ( 118.3554748109119998, -9.565557343593413364, -10.61323700422348004 ) ) ;
#22721 = CARTESIAN_POINT ( 'NONE',  ( 69.69189222814998175, -41.76310523276723785, -24.89321520033831447 ) ) ;
#22722 = CARTESIAN_POINT ( 'NONE',  ( 116.1777233795247781, -8.938348069036489818, -17.46756447353520159 ) ) ;
#22723 = ORIENTED_EDGE ( 'NONE', *, *, #7558, .T. ) ;
#22724 = B_SPLINE_CURVE_WITH_KNOTS ( 'NONE', 3,
 ( #15547, #39497, #29452, #25372, #39041, #21939, #8706, #39944, #28793, #8260 ),
 .UNSPECIFIED., .F., .F.,
 ( 4, 3, 3, 4 ),
 ( 0.000000000000000000, 0.0002476487219222849707, 0.0004952974148303729719, 0.0009534114850261750764 ),
 .UNSPECIFIED. ) ;
#22725 = DIRECTION ( 'NONE',  ( 0.000000000000000000, -0.4669533266896290225, -0.8842819633428516957 ) ) ;
#22726 = CARTESIAN_POINT ( 'NONE',  ( 123.5176014775786228, -9.261995988541697145, -16.69588392320189030 ) ) ;
#22727 = CARTESIAN_POINT ( 'NONE',  ( 125.3328548109119964, -0.8288870151387760510, -10.36305467784173118 ) ) ;
#22728 = AXIS2_PLACEMENT_3D ( 'NONE', #2553, #32553, #18206 ) ;
#22729 = CARTESIAN_POINT ( 'NONE',  ( 124.3741441133336991, 3.029370655639220367, -12.39654276031037305 ) ) ;
#22730 = CARTESIAN_POINT ( 'NONE',  ( 118.7525614775786380, -1.833838273342659253, -17.42832698103878286 ) ) ;
#22731 = CARTESIAN_POINT ( 'NONE',  ( 112.2857214775786474, -4.089484607189486809, -7.948022111789456723 ) ) ;
#22732 = LINE ( 'NONE', #12943, #35444 ) ;
#22733 = CARTESIAN_POINT ( 'NONE',  ( 122.6099748109119929, -0.8288870151387760510, -10.36305467784173118 ) ) ;
#22734 = CARTESIAN_POINT ( 'NONE',  ( 121.8755514478796442, -9.877548923986811502, -16.68609415519376427 ) ) ;
#22735 = CARTESIAN_POINT ( 'NONE',  ( 125.2194014775786286, 0.1319031606808879209, -14.10382304977623669 ) ) ;
#22736 = CARTESIAN_POINT ( 'NONE',  ( 125.3159867104938456, -11.52188856829479491, -15.97039513045710102 ) ) ;
#22737 = CARTESIAN_POINT ( 'NONE',  ( 122.2696148109119889, -4.089484607189486809, -7.948022111789456723 ) ) ;
#22738 = CARTESIAN_POINT ( 'NONE',  ( 116.6536748109119941, -10.15424416112533912, -14.75197769757731336 ) ) ;
#22739 = CARTESIAN_POINT ( 'NONE',  ( 121.2485348109119769, -8.899110576539710493, -16.42337572283490132 ) ) ;
#22740 = ORIENTED_EDGE ( 'NONE', *, *, #30620, .F. ) ;
#22741 = CARTESIAN_POINT ( 'NONE',  ( 123.0070614775786169, 0.9020085738987339008, -11.91225656197089222 ) ) ;
#22742 = CARTESIAN_POINT ( 'NONE',  ( 115.1787814775786387, -9.988377603198976828, -10.36322818467138340 ) ) ;
#22743 = CARTESIAN_POINT ( 'NONE',  ( 113.3301452545248083, -9.868328341294098749, -15.46607636864997204 ) ) ;
#22744 = FACE_OUTER_BOUND ( 'NONE', #32752, .T. ) ;
#22745 = CARTESIAN_POINT ( 'NONE',  ( 124.0848681442452772, -5.574606645277164318, -18.38911715685844683 ) ) ;
#22747 = CARTESIAN_POINT ( 'NONE',  ( 123.6877814775786533, -3.383040157471821630, -19.15922257007629170 ) ) ;
#22746 = AXIS2_PLACEMENT_3D ( 'NONE', #3205, #38296, #17130 ) ;
#22748 = CARTESIAN_POINT ( 'NONE',  ( 114.4413952545248350, 0.8980012041604421569, -11.00651665394454071 ) ) ;
#22749 = CARTESIAN_POINT ( 'NONE',  ( 110.7603796295247918, -4.863998795839590272, -8.388885654883775800 ) ) ;
#22750 = CYLINDRICAL_SURFACE ( 'NONE', #16093, 1.999999999999999556 ) ;
#22751 = CARTESIAN_POINT ( 'NONE',  ( 114.4980614775786734, -2.084020599724406786, -8.691656652584148546 ) ) ;
#22752 = AXIS2_PLACEMENT_3D ( 'NONE', #8348, #12680, #29320 ) ;
#22753 = LINE ( 'NONE', #12734, #34969 ) ;
#22754 = CARTESIAN_POINT ( 'NONE',  ( 112.9828796295247884, -4.863998795839590272, -8.388885654883775800 ) ) ;
#22755 = ORIENTED_EDGE ( 'NONE', *, *, #18366, .T. ) ;
#22756 = CARTESIAN_POINT ( 'NONE',  ( 124.0848681442452772, -5.574606645277164318, -18.38911715685844683 ) ) ;
#22757 = CARTESIAN_POINT ( 'NONE',  ( 122.0354079359119908, -5.444069387712269226, -19.60292469916370450 ) ) ;
#22758 = CARTESIAN_POINT ( 'NONE',  ( 123.4939235609119663, 0.6414057260225851653, -11.69287257290600657 ) ) ;
#22759 = CARTESIAN_POINT ( 'NONE',  ( 88.22708560785949317, -3.622631779710408395, -18.64321520033831803 ) ) ;
#22760 = EDGE_CURVE ( 'NONE', #14232, #29216, #6102, .T. ) ;
#22761 = CARTESIAN_POINT ( 'NONE',  ( 106.4542858795248179, -8.402594152722688392, -9.854619843455216355 ) ) ;
#22762 = VERTEX_POINT ( 'NONE', #21110 ) ;
#22763 = TOROIDAL_SURFACE ( 'NONE', #12560, 33.80000000000000426, 1.199999999999999956 ) ;
#22764 = CARTESIAN_POINT ( 'NONE',  ( 120.0005481442453146, -5.638512984488999180, -18.83840828888717311 ) ) ;
#22765 = CARTESIAN_POINT ( 'NONE',  ( 113.0798948109119948, -0.4660016031367885114, -10.09054647747474220 ) ) ;
#22766 = CARTESIAN_POINT ( 'NONE',  ( 123.1772414775786189, -5.574606645277164318, -18.38911715685844683 ) ) ;
#22767 = CARTESIAN_POINT ( 'NONE',  ( 116.3133148109120043, -2.084020599724406786, -8.691656652584148546 ) ) ;
#22768 = DIRECTION ( 'NONE',  ( -0.9609149988134837450, 0.1028163501681639419, -0.2570431154366518145 ) ) ;
#22769 = CARTESIAN_POINT ( 'NONE',  ( 94.20708369096698220, -26.09538666226425363, -14.49867541642786861 ) ) ;
#22770 = CARTESIAN_POINT ( 'NONE',  ( 114.6115148109119986, -3.383040157471821630, -19.15922257007629170 ) ) ;
#22771 = CARTESIAN_POINT ( 'NONE',  ( 112.9828796295247884, -4.863998795839590272, -8.388885654883775800 ) ) ;
#22772 = CARTESIAN_POINT ( 'NONE',  ( 122.4397948109119767, -9.988377603198976828, -10.36322818467138340 ) ) ;
#22773 =( BOUNDED_CURVE ( )  B_SPLINE_CURVE ( 2, ( #26547, #19697, #6246, #20390, #23351, #6009, #12878, #29965, #30865, #26778, #40687, #23589, #9671, #33357, #44788, #13546, #20168 ),
 .UNSPECIFIED., .F., .T. ) 
 B_SPLINE_CURVE_WITH_KNOTS ( ( 3, 2, 2, 2, 2, 2, 2, 2, 3 ),
 ( 0.2602707595410510000, 0.2812500000000000000, 0.3125000000000000000, 0.3437500000000000000, 0.3750000000000000000, 0.4062500000000000000, 0.4375000000000000000, 0.4687500000000000000, 0.4897292404589490000 ),
 .UNSPECIFIED. ) 
 CURVE ( )  GEOMETRIC_REPRESENTATION_ITEM ( )  RATIONAL_B_SPLINE_CURVE ( ( 0.9664089390052280626, 0.9488976130786129781, 1.000000000000000000, 0.9238795325112869605, 1.000000000000000000, 0.9238795325112869605, 1.000000000000000000, 0.9238795325112869605, 1.000000000000000000, 0.9238795325112869605, 1.000000000000000000, 0.9238795325112869605, 1.000000000000000000, 0.9238795325112869605, 1.000000000000000000, 0.9488976130786129781, 0.9664089390052280626 ) ) 
 REPRESENTATION_ITEM ( '' )  );
#22774 = FACE_OUTER_BOUND ( 'NONE', #6186, .T. ) ;
#22775 = VERTEX_POINT ( 'NONE', #7198 ) ;
#22776 = EDGE_CURVE ( 'NONE', #43318, #34402, #586, .T. ) ;
#22777 = CARTESIAN_POINT ( 'NONE',  ( 112.6828081442453282, -7.893985811506177619, -18.51759400769804742 ) ) ;
#22778 = EDGE_CURVE ( 'NONE', #23986, #37731, #4224, .T. ) ;
#22779 = EDGE_CURVE ( 'NONE', #970, #28048, #19942, .T. ) ;
#22780 = CARTESIAN_POINT ( 'NONE',  ( 114.5547881442453217, -4.153390946401321671, -8.397313243818183892 ) ) ;
#22781 = VECTOR ( 'NONE', #29663, 1000.000000000000000 ) ;
#22782 = CARTESIAN_POINT ( 'NONE',  ( 126.2455040230458536, -5.344711546414948167, -18.38488247629714678 ) ) ;
#22783 = CARTESIAN_POINT ( 'NONE',  ( 125.7299414775786346, -10.15424416112533912, -14.75197769757731336 ) ) ;
#22784 = ORIENTED_EDGE ( 'NONE', *, *, #1026, .F. ) ;
#22785 = CARTESIAN_POINT ( 'NONE',  ( 122.6667014775786413, -7.893985811506177619, -18.51759400769804742 ) ) ;
#22786 = LINE ( 'NONE', #1803, #5585 ) ;
#22787 = CARTESIAN_POINT ( 'NONE',  ( 115.8150068052895563, -1.125321370491268125, -17.12283323191015327 ) ) ;
#22788 = CARTESIAN_POINT ( 'NONE',  ( 111.5125327111057345, -1.267766418764825875, -16.93314635290698789 ) ) ;
#22789 = CARTESIAN_POINT ( 'NONE',  ( 123.4844656136282026, -4.072025463651757882, -15.69684013478500972 ) ) ;
#22790 = CARTESIAN_POINT ( 'NONE',  ( 113.9875214775786532, -8.899110576539710493, -16.42337572283490132 ) ) ;
#22791 = DIRECTION ( 'NONE',  ( -0.6383198453882292789, -0.7697712484781092934, 0.000000000000000000 ) ) ;
#22792 = VECTOR ( 'NONE', #32256, 1000.000000000000000 ) ;
#22793 = CARTESIAN_POINT ( 'NONE',  ( 125.2222176290895845, -1.950389891022559663, -20.09533972395541568 ) ) ;
#22794 = CARTESIAN_POINT ( 'NONE',  ( 126.0703014775786102, -9.988377603198980381, -10.36322818467138518 ) ) ;
#22795 = CARTESIAN_POINT ( 'NONE',  ( 112.9664414775786412, 0.5811942927096154232, -14.16772938898807155 ) ) ;
#22796 = CARTESIAN_POINT ( 'NONE',  ( 124.1884548109119777, -2.527210466738041728, -8.967976844669124148 ) ) ;
#22797 = CARTESIAN_POINT ( 'NONE',  ( 126.2404814775786264, -0.8288870151387760510, -10.36305467784173118 ) ) ;
#22798 = CARTESIAN_POINT ( 'NONE',  ( 116.0864081442453113, -0.1624402480850797581, -16.17319339645315424 ) ) ;
#22799 = CARTESIAN_POINT ( 'NONE',  ( 122.6099748109119929, -9.261995988541697145, -16.69588392320189030 ) ) ;
#22800 = CARTESIAN_POINT ( 'NONE',  ( 120.1707281442453166, 0.2603800115204892296, -16.42320221600525088 ) ) ;
#22801 = VERTEX_POINT ( 'NONE', #27970 ) ;
#22802 = CARTESIAN_POINT ( 'NONE',  ( 89.67401078471493747, -25.99489077589524300, -13.39321520033831447 ) ) ;
#22803 = CARTESIAN_POINT ( 'NONE',  ( 109.7880358795247986, -0.7896495226426338832, -17.46756447353520159 ) ) ;
#22804 = EDGE_CURVE ( 'NONE', #18421, #41822, #15574, .T. ) ;
#22805 = CARTESIAN_POINT ( 'NONE',  ( 109.0240515045248202, -6.936859964151250502, -18.39754474579286025 ) ) ;
#22806 = CARTESIAN_POINT ( 'NONE',  ( 108.0517077545248696, -2.791137627527939813, -18.39754474579286025 ) ) ;
#22807 = CARTESIAN_POINT ( 'NONE',  ( 70.19189222814998175, -57.25954915413987578, -36.10662921840084749 ) ) ;
#22808 = CARTESIAN_POINT ( 'NONE',  ( 116.7671281442453335, -1.834011780172310813, -8.268836392978581529 ) ) ;
#22809 = ORIENTED_EDGE ( 'NONE', *, *, #25664, .T. ) ;
#22810 = CARTESIAN_POINT ( 'NONE',  ( 125.2714945850566863, -9.321016064732583928, -19.11382972112425804 ) ) ;
#22811 = CARTESIAN_POINT ( 'NONE',  ( 124.3273610609119686, -6.340755971794695078, -8.611740276972781771 ) ) ;
#22812 = CARTESIAN_POINT ( 'NONE',  ( 121.9470836909669913, -25.99489077589524300, -13.39321520033831447 ) ) ;
#22813 = CARTESIAN_POINT ( 'NONE',  ( 114.1009748109119784, -5.574606645277164318, -18.38911715685844683 ) ) ;
#22814 = EDGE_CURVE ( 'NONE', #39438, #20119, #43967, .T. ) ;
#22815 = B_SPLINE_CURVE_WITH_KNOTS ( 'NONE', 3,
 ( #14285, #9984, #28204, #17480, #38440, #7210, #37554, #41447, #3781, #42111 ),
 .UNSPECIFIED., .F., .F.,
 ( 4, 3, 3, 4 ),
 ( 3.127317220692749988E-18, 0.0002476486808869860054, 0.0004952973797228679611, 0.0009539399846111490172 ),
 .UNSPECIFIED. ) ;
#22816 = CARTESIAN_POINT ( 'NONE',  ( 118.4122014775786340, 0.5811942927096110934, -14.16772938898807510 ) ) ;
#22817 = EDGE_CURVE ( 'NONE', #13419, #24082, #35212, .T. ) ;
#22818 = CARTESIAN_POINT ( 'NONE',  ( 109.7880358795247986, -0.7896495226426338832, -17.46756447353520159 ) ) ;
#22819 = LINE ( 'NONE', #8918, #40276 ) ;
#22820 = VERTEX_POINT ( 'NONE', #3771 ) ;
#22821 = CARTESIAN_POINT ( 'NONE',  ( 120.5887993777725029, -1.267766418764730840, -16.93314635290706605 ) ) ;
#22822 = CARTESIAN_POINT ( 'NONE',  ( 117.1642148109119859, -0.8288870151387760510, -10.36305467784173118 ) ) ;
#22823 = VECTOR ( 'NONE', #32068, 1000.000000000000000 ) ;
#22824 = CARTESIAN_POINT ( 'NONE',  ( 119.0361948109119652, -7.893985811506177619, -18.51759400769804742 ) ) ;
#22825 = CARTESIAN_POINT ( 'NONE',  ( 112.9664414775786412, -9.859900752359374465, -12.68260735090039404 ) ) ;
#22826 = CARTESIAN_POINT ( 'NONE',  ( 114.7816948109119863, 0.5811942927096154232, -14.16772938898807155 ) ) ;
#22827 = CARTESIAN_POINT ( 'NONE',  ( 121.9470836909669913, -27.84333996136784961, -14.15691383771150136 ) ) ;
#22828 = CARTESIAN_POINT ( 'NONE',  ( 122.7234281442452755, -4.153390946401325223, -8.397313243818185668 ) ) ;
#22829 = CARTESIAN_POINT ( 'NONE',  ( 121.0783548109119749, -9.565557343593413364, -10.61323700422348004 ) ) ;
#22830 = ORIENTED_EDGE ( 'NONE', *, *, #18972, .T. ) ;
#22831 = CARTESIAN_POINT ( 'NONE',  ( 89.29245855188943892, -9.882163754870950001, -8.143215200338314474 ) ) ;
#22832 = CIRCLE ( 'NONE', #9732, 5.999999999999997335 ) ;
#22833 = CARTESIAN_POINT ( 'NONE',  ( 114.0442481442453300, -1.834011780172310813, -8.268836392978581529 ) ) ;
#22834 = CARTESIAN_POINT ( 'NONE',  ( 120.3409081442453044, -8.899110576539710493, -16.42337572283490132 ) ) ;
#22835 = EDGE_LOOP ( 'NONE', ( #16299, #44284, #9411, #9086 ) ) ;
#22836 = EDGE_CURVE ( 'NONE', #44158, #32023, #39432, .T. ) ;
#22837 = CARTESIAN_POINT ( 'NONE',  ( 124.5357204359119550, -10.25716656981731489, -12.88942061488890545 ) ) ;
#22838 = EDGE_CURVE ( 'NONE', #10520, #43489, #26491, .T. ) ;
#22839 = EDGE_CURVE ( 'NONE', #15605, #35231, #32864, .T. ) ;
#22840 = CARTESIAN_POINT ( 'NONE',  ( 119.8870948109119752, -9.261995988541697145, -16.69588392320189030 ) ) ;
#22841 = CARTESIAN_POINT ( 'NONE',  ( 113.3995983795247895, -0.7896495226426338832, -9.318865927141430916 ) ) ;
#22842 = CARTESIAN_POINT ( 'NONE',  ( 117.6180281442453150, -8.899110576539710493, -16.42337572283490132 ) ) ;
#22843 = VERTEX_POINT ( 'NONE', #4896 ) ;
#22844 = ORIENTED_EDGE ( 'NONE', *, *, #16974, .F. ) ;
#22845 = CARTESIAN_POINT ( 'NONE',  ( 120.7947214775786193, -0.8288870151387760510, -10.36305467784173118 ) ) ;
#22846 = CARTESIAN_POINT ( 'NONE',  ( 121.3619881442452879, -5.574606645277164318, -18.38911715685844683 ) ) ;
#22847 = CARTESIAN_POINT ( 'NONE',  ( 96.54708369096698561, -27.29184247633061489, -11.60278472507885894 ) ) ;
#22848 = CARTESIAN_POINT ( 'NONE',  ( 121.9470836909669913, -25.99489077589524300, -13.39321520033831447 ) ) ;
#22849 = VECTOR ( 'NONE', #15788, 1000.000000000000000 ) ;
#22850 = CARTESIAN_POINT ( 'NONE',  ( 61.80622722289361093, -65.84395357266009796, -43.65918878370688105 ) ) ;
#22851 = CARTESIAN_POINT ( 'NONE',  ( 116.5969481442453031, 0.5811942927096154232, -14.16772938898807155 ) ) ;
#22852 = CARTESIAN_POINT ( 'NONE',  ( 70.19189222814998175, -100.0979043305785581, -53.24182196210380624 ) ) ;
#22853 = CARTESIAN_POINT ( 'NONE',  ( 117.5045748109119756, 0.5811942927096110934, -14.16772938898807510 ) ) ;
#22855 = CARTESIAN_POINT ( 'NONE',  ( 115.2355081442453155, 0.1319031606808879209, -14.10382304977623669 ) ) ;
#22854 = CARTESIAN_POINT ( 'NONE',  ( 114.3846081442453197, -10.63000616557722466, -14.87417383870573495 ) ) ;
#22856 = CARTESIAN_POINT ( 'NONE',  ( 122.6099748109119929, -0.8288870151387760510, -10.36305467784173118 ) ) ;
#22857 = CARTESIAN_POINT ( 'NONE',  ( 113.5904348109119866, -7.893985811506177619, -18.51759400769804742 ) ) ;
#22858 = VERTEX_POINT ( 'NONE', #18813 ) ;
#22859 = CARTESIAN_POINT ( 'NONE',  ( 124.3685014775786328, 0.4262465694468514643, -12.03445270309931736 ) ) ;
#22860 = CARTESIAN_POINT ( 'NONE',  ( 113.8197041868944979, -2.239543233855025850, -18.13706010537467606 ) ) ;
#22861 = CARTESIAN_POINT ( 'NONE',  ( 112.9828796295247884, -4.863998795839590272, -19.15521520033831493 ) ) ;
#22862 = DIRECTION ( 'NONE',  ( 0.1957579692570465546, -0.4041862076864165543, -0.8934832550128906092 ) ) ;
#22863 = CARTESIAN_POINT ( 'NONE',  ( 113.7468640045248236, -10.62599879583958717, -11.00651665394454604 ) ) ;
#22864 = CARTESIAN_POINT ( 'NONE',  ( 120.4543614775786295, -4.089484607189486809, -7.948022111789456723 ) ) ;
#22865 = ORIENTED_EDGE ( 'NONE', *, *, #19192, .F. ) ;
#22866 = CARTESIAN_POINT ( 'NONE',  ( 119.9438214775786378, -7.893985811506177619, -18.51759400769804742 ) ) ;
#22867 = CARTESIAN_POINT ( 'NONE',  ( 90.06246830635160450, -25.38011337280982715, -14.88121679464376257 ) ) ;
#22868 = CARTESIAN_POINT ( 'NONE',  ( 107.6349890045248401, 0.8980012041604421569, -15.77991374673208469 ) ) ;
#22869 = CARTESIAN_POINT ( 'NONE',  ( 120.5678148109119832, -8.166667518702819706, -8.995218007635861213 ) ) ;
#22870 = CARTESIAN_POINT ( 'NONE',  ( 115.8595014775786609, -1.834011780172310813, -8.268836392978581529 ) ) ;
#22871 = CARTESIAN_POINT ( 'NONE',  ( 125.4584548109119737, -8.245233026025740486, -17.07659070123625611 ) ) ;
#22872 = LINE ( 'NONE', #18560, #22048 ) ;
#22873 = ORIENTED_EDGE ( 'NONE', *, *, #31477, .T. ) ;
#22874 = CYLINDRICAL_SURFACE ( 'NONE', #22313, 5.999999999999997335 ) ;
#22875 = CARTESIAN_POINT ( 'NONE',  ( 109.2295804820058436, -10.43592689531145190, -13.30118990145861702 ) ) ;
#22876 = CARTESIAN_POINT ( 'NONE',  ( 119.3198281442452924, -9.859900752359374465, -12.68260735090039404 ) ) ;
#22877 = CARTESIAN_POINT ( 'NONE',  ( 113.6774108795247997, -1.325403438956436419, -16.93181055722141792 ) ) ;
#22878 = CARTESIAN_POINT ( 'NONE',  ( 111.3854577545248645, -2.791137627527939813, -18.39754474579286025 ) ) ;
#22879 = CARTESIAN_POINT ( 'NONE',  ( 119.5467348109119712, -5.574606645277164318, -18.38911715685844683 ) ) ;
#22880 = DIRECTION ( 'NONE',  ( 0.000000000000000000, 0.000000000000000000, 1.000000000000000000 ) ) ;
#22881 = CARTESIAN_POINT ( 'NONE',  ( 71.20716749095201692, -24.93145248074033660, -5.218938316983485315 ) ) ;
#22882 = CARTESIAN_POINT ( 'NONE',  ( 114.1577014775786552, -3.505236298600246325, -18.68346056562440793 ) ) ;
#22883 = CARTESIAN_POINT ( 'NONE',  ( 123.0070614775786169, 0.9020085738987339008, -11.91225656197089222 ) ) ;
#22885 = ORIENTED_EDGE ( 'NONE', *, *, #1868, .T. ) ;
#22884 = ADVANCED_FACE ( 'NONE', ( #12206 ), #32705, .F. ) ;
#22886 = CIRCLE ( 'NONE', #1807, 5.132259260909266985 ) ;
#22887 = CARTESIAN_POINT ( 'NONE',  ( 122.2696148109119889, -5.574606645277164318, -18.38911715685844683 ) ) ;
#22888 = CARTESIAN_POINT ( 'NONE',  ( 113.3635281442453504, -9.988377603198976828, -10.36322818467138340 ) ) ;
#22889 = CARTESIAN_POINT ( 'NONE',  ( 122.3263414775786373, -6.344957434206665248, -7.627207830600338134 ) ) ;
#22890 = CARTESIAN_POINT ( 'NONE',  ( 123.0070614775786169, -10.15424416112533912, -14.75197769757731336 ) ) ;
#22891 = ORIENTED_EDGE ( 'NONE', *, *, #30487, .F. ) ;
#22892 = CARTESIAN_POINT ( 'NONE',  ( 123.9714148109119805, -8.899110576539710493, -16.42337572283490132 ) ) ;
#22893 = CARTESIAN_POINT ( 'NONE',  ( 124.7088614775786226, 0.2603800115204892296, -16.42320221600525088 ) ) ;
#22894 = CARTESIAN_POINT ( 'NONE',  ( 124.0650380271182200, -8.523251919909833774, -6.279197823564533820 ) ) ;
#22895 = CARTESIAN_POINT ( 'NONE',  ( 126.2404814775786264, -9.261995988541697145, -16.69588392320189030 ) ) ;
#22896 = ADVANCED_FACE ( 'NONE', ( #5121 ), #1734, .T. ) ;
#22897 = CARTESIAN_POINT ( 'NONE',  ( 107.2877233795247776, -8.938348069036489818, -17.46756447353520159 ) ) ;
#22898 = B_SPLINE_CURVE_WITH_KNOTS ( 'NONE', 3,
 ( #44863, #41443, #41667, #44637, #37316, #6087, #31157, #13619, #27527, #27075 ),
 .UNSPECIFIED., .F., .F.,
 ( 4, 3, 3, 4 ),
 ( 0.000000000000000000, 0.0002476486447138875262, 0.0004952972925464290419, 0.0009604418836934499335 ),
 .UNSPECIFIED. ) ;
#22899 = CARTESIAN_POINT ( 'NONE',  ( 120.5768923109119868, -0.4387604401700512802, -15.73000352943951619 ) ) ;
#22900 = CARTESIAN_POINT ( 'NONE',  ( 127.7500697630001554, -3.418455135964745484, -14.06918277244200510 ) ) ;
#22901 = AXIS2_PLACEMENT_3D ( 'NONE', #13837, #17700, #31600 ) ;
#22902 = CARTESIAN_POINT ( 'NONE',  ( 108.6767858795247861, -8.402594152722688392, -9.854619843455216355 ) ) ;
#22903 = CARTESIAN_POINT ( 'NONE',  ( 93.44708369096697709, -25.23119213852205789, -15.24166438581092109 ) ) ;
#22904 = CARTESIAN_POINT ( 'NONE',  ( 117.1519828165343853, -2.324775150319241757, -18.02356106541842706 ) ) ;
#22905 = CARTESIAN_POINT ( 'NONE',  ( 120.3976348109119812, -7.643976991954077427, -18.09477374809248928 ) ) ;
#22906 = CARTESIAN_POINT ( 'NONE',  ( 123.8579614775786126, 0.5811942927096110934, -14.16772938898807510 ) ) ;
#22907 = CARTESIAN_POINT ( 'NONE',  ( 126.2184548109119788, -5.614349408395407970, -18.33681267546239724 ) ) ;
#22908 = VERTEX_POINT ( 'NONE', #15851 ) ;
#22909 = CARTESIAN_POINT ( 'NONE',  ( 116.3860827545247787, -6.936859964151250502, -8.388885654883777576 ) ) ;
#22910 = CARTESIAN_POINT ( 'NONE',  ( 107.9822546295247889, -4.863998795839590272, -18.39754474579285315 ) ) ;
#22911 = CARTESIAN_POINT ( 'NONE',  ( 116.3133148109120043, -2.084020599724406786, -8.691656652584148546 ) ) ;
#22912 = AXIS2_PLACEMENT_3D ( 'NONE', #40529, #37314, #20003 ) ;
#22913 = CARTESIAN_POINT ( 'NONE',  ( 86.75477599865929790, -26.60966817898065884, -11.90521360603286816 ) ) ;
#22914 = CARTESIAN_POINT ( 'NONE',  ( 66.95179978577000668, -0.07398856205378337436, -10.39321520033831447 ) ) ;
#22915 = LINE ( 'NONE', #32489, #12949 ) ;
#22917 = CARTESIAN_POINT ( 'NONE',  ( 121.3619881442452879, -4.089484607189486809, -7.948022111789456723 ) ) ;
#22916 = CARTESIAN_POINT ( 'NONE',  ( 69.04371756932381743, -26.05018752390734349, -5.893215200338321580 ) ) ;
#22918 = CARTESIAN_POINT ( 'NONE',  ( 122.0994348109119443, -10.15424416112533912, -14.75197769757731336 ) ) ;
#22919 = ORIENTED_EDGE ( 'NONE', *, *, #36970, .T. ) ;
#22920 = CARTESIAN_POINT ( 'NONE',  ( 84.87879901378997261, -30.44422003934618814, -8.393215200338314474 ) ) ;
#22921 = CARTESIAN_POINT ( 'NONE',  ( 126.2940345447965456, 0.06676713698955166754, -14.42618009100540277 ) ) ;
#22922 = CARTESIAN_POINT ( 'NONE',  ( 108.4684265045247997, -2.791137627527939813, -8.388885654883777576 ) ) ;
#22923 = CARTESIAN_POINT ( 'NONE',  ( 121.0783548109119749, -9.565557343593413364, -10.61323700422348004 ) ) ;
#22924 = CARTESIAN_POINT ( 'NONE',  ( 118.4122014775786340, -9.859900752359374465, -12.68260735090039404 ) ) ;
#22925 = CARTESIAN_POINT ( 'NONE',  ( 119.4455134719562182, -1.125321370491285444, -17.12283323191017814 ) ) ;
#22926 = CARTESIAN_POINT ( 'NONE',  ( 116.0388171295248014, 0.1403307496149613920, -13.39321520033831447 ) ) ;
#22927 = CARTESIAN_POINT ( 'NONE',  ( 1093.930577029472943, -25.99489077589524300, -13.39321520033831447 ) ) ;
#22928 = CARTESIAN_POINT ( 'NONE',  ( 59.24641515291911986, -13.72835195454734247, -8.593215200338315540 ) ) ;
#22929 = DIRECTION ( 'NONE',  ( 1.000000000000000000, 2.439015257082815255E-15, 0.000000000000000000 ) ) ;
#22930 = CARTESIAN_POINT ( 'NONE',  ( 109.3018640045248304, -10.62599879583958717, -11.00651665394454604 ) ) ;
#22931 = CARTESIAN_POINT ( 'NONE',  ( 116.3539803407245046, 2.267523965085636917, -20.30237287253366674 ) ) ;
#22932 = CARTESIAN_POINT ( 'NONE',  ( 113.9552233795247815, -8.938348069036489818, -17.46756447353520159 ) ) ;
#22933 = CARTESIAN_POINT ( 'NONE',  ( 119.4900081442453086, -1.834011780172310813, -8.268836392978581529 ) ) ;
#22934 = CARTESIAN_POINT ( 'NONE',  ( 121.3052614775786111, -1.834011780172310813, -8.268836392978581529 ) ) ;
#22935 = CARTESIAN_POINT ( 'NONE',  ( 108.5378796295247810, -4.863998795839590272, -19.15521520033831493 ) ) ;
#22936 = CARTESIAN_POINT ( 'NONE',  ( 116.3700414775786527, -5.638512984488999180, -18.83840828888717311 ) ) ;
#22937 = CARTESIAN_POINT ( 'NONE',  ( 112.5693548109119888, -10.63000616557722466, -14.87417383870573495 ) ) ;
#22938 = ORIENTED_EDGE ( 'NONE', *, *, #18920, .T. ) ;
#22939 = DIRECTION ( 'NONE',  ( 0.5735764363510499342, 0.3127926500124801890, -0.7570804645221008711 ) ) ;
#22940 = B_SPLINE_CURVE_WITH_KNOTS ( 'NONE', 3,
 ( #30665, #26569, #12443, #19953, #20189, #23151, #16543, #2840, #19500, #44134 ),
 .UNSPECIFIED., .F., .F.,
 ( 4, 3, 3, 4 ),
 ( 0.000000000000000000, 0.0002476487219222810133, 0.0004952974148303670087, 0.0009534114850261750764 ),
 .UNSPECIFIED. ) ;
#22941 = AXIS2_PLACEMENT_3D ( 'NONE', #42650, #14606, #38992 ) ;
#22942 = CARTESIAN_POINT ( 'NONE',  ( 122.4965214775786251, -10.30919188438810075, -12.61870101168855918 ) ) ;
#22943 = CARTESIAN_POINT ( 'NONE',  ( 121.7590748109119687, -7.893985811506177619, -18.51759400769804742 ) ) ;
#22944 = CARTESIAN_POINT ( 'NONE',  ( 111.8319081442453182, -5.638512984488999180, -18.83840828888717311 ) ) ;
#22945 = ITEM_DEFINED_TRANSFORMATION ( 'NONE', 'NONE', #24947,  #12375 ) ;
#22946 = CARTESIAN_POINT ( 'NONE',  ( 125.9001214775786224, -4.089484607189486809, -7.948022111789456723 ) ) ;
#22947 = CARTESIAN_POINT ( 'NONE',  ( 114.6115148109119986, -6.222761293078241884, -8.102969835052219238 ) ) ;
#22948 = CARTESIAN_POINT ( 'NONE',  ( 124.0848681442452772, -4.089484607189486809, -7.948022111789456723 ) ) ;
#22949 = CIRCLE ( 'NONE', #33838, 5.999999999999997335 ) ;
#22950 = CARTESIAN_POINT ( 'NONE',  ( 109.9963952545248134, 0.8980012041604421569, -11.00651665394454071 ) ) ;
#22951 = EDGE_CURVE ( 'NONE', #31774, #25264, #27242, .T. ) ;
#22952 = CARTESIAN_POINT ( 'NONE',  ( 121.0216281442452981, -7.894159318335828068, -9.358103419637847864 ) ) ;
#22953 = DIRECTION ( 'NONE',  ( 0.000000000000000000, 0.000000000000000000, 1.000000000000000000 ) ) ;
#22954 = CARTESIAN_POINT ( 'NONE',  ( 77.25325688895158294, -4.012910213732562070, -8.143215200338314474 ) ) ;
#22955 = ORIENTED_EDGE ( 'NONE', *, *, #12048, .T. ) ;
#22956 = CARTESIAN_POINT ( 'NONE',  ( 71.02242295334774269, -60.62383483080748903, -40.55713941032976066 ) ) ;
#22957 = CARTESIAN_POINT ( 'NONE',  ( 123.2906948109119867, -8.166667518702819706, -8.995218007635861213 ) ) ;
#22958 = CARTESIAN_POINT ( 'NONE',  ( 93.44708369096697709, -25.99489077589524300, -13.39321520033831447 ) ) ;
#22959 = CARTESIAN_POINT ( 'NONE',  ( 125.0480389746925738, 2.573808657167731440, -12.21219197517087096 ) ) ;
#22960 =( NAMED_UNIT ( * ) SI_UNIT ( $, .STERADIAN. ) SOLID_ANGLE_UNIT ( ) );
#22961 = CARTESIAN_POINT ( 'NONE',  ( 67.42128206111212307, -0.1796520177129405649, -16.39321520033831447 ) ) ;
#22962 = CARTESIAN_POINT ( 'NONE',  ( 83.72016463086879412, -27.84333996136784961, -14.15691383771150136 ) ) ;
#22963 =( BOUNDED_CURVE ( )  B_SPLINE_CURVE ( 3, ( #44101, #34643, #12866, #26537 ),
 .UNSPECIFIED., .F., .F. ) 
 B_SPLINE_CURVE_WITH_KNOTS ( ( 4, 4 ),
 ( 4.712388980384689674, 6.283185307179590673 ),
 .UNSPECIFIED. ) 
 CURVE ( )  GEOMETRIC_REPRESENTATION_ITEM ( )  RATIONAL_B_SPLINE_CURVE ( ( 1.000000000000000000, 0.8047378541243649375, 0.8047378541243649375, 1.000000000000000000 ) ) 
 REPRESENTATION_ITEM ( '' )  );
#22964 = CARTESIAN_POINT ( 'NONE',  ( 124.2550481442452792, -0.1624402480850797581, -16.17319339645315424 ) ) ;
#22965 = CARTESIAN_POINT ( 'NONE',  ( 120.9936110609119737, -3.163656168406939528, -18.89861972220014152 ) ) ;
#22966 = CARTESIAN_POINT ( 'NONE',  ( 123.9146881442452894, -10.15424416112533912, -14.75197769757731336 ) ) ;
#22967 = AXIS2_PLACEMENT_3D ( 'NONE', #33146, #4668, #18590 ) ;
#22968 = CARTESIAN_POINT ( 'NONE',  ( 125.2909043387969490, -11.52983536252548546, -16.08521104921829448 ) ) ;
#22969 = EDGE_CURVE ( 'NONE', #18093, #3055, #23127, .T. ) ;
#22970 = CARTESIAN_POINT ( 'NONE',  ( 125.5597614775786326, -1.561330072975669392, -17.79121239304076951 ) ) ;
#22971 = CARTESIAN_POINT ( 'NONE',  ( 116.7671281442453335, -7.643976991954077427, -18.09477374809248928 ) ) ;
#22972 = LINE ( 'NONE', #3511, #33513 ) ;
#22973 = EDGE_LOOP ( 'NONE', ( #35774, #38524, #44521, #14478 ) ) ;
#22974 = CARTESIAN_POINT ( 'NONE',  ( 124.8223148109119762, 0.9020085738987339008, -11.91225656197089222 ) ) ;
#22975 = CARTESIAN_POINT ( 'NONE',  ( 115.3489614775786407, -9.261995988541697145, -16.69588392320189030 ) ) ;
#22976 = CARTESIAN_POINT ( 'NONE',  ( 114.9970202545248412, 0.1403307496149616695, -11.32035403202665336 ) ) ;
#22977 = CARTESIAN_POINT ( 'NONE',  ( 113.4202548109119846, 0.1319031606808879209, -14.10382304977623669 ) ) ;
#22978 = VECTOR ( 'NONE', #41591, 1000.000000000000227 ) ;
#22979 = CARTESIAN_POINT ( 'NONE',  ( 124.7655881442452852, -9.859900752359378018, -12.68260735090039759 ) ) ;
#22980 = CARTESIAN_POINT ( 'NONE',  ( 122.7234281442452755, -5.638512984488999180, -18.83840828888717311 ) ) ;
#22981 = CARTESIAN_POINT ( 'NONE',  ( 116.3166296295247832, -4.863998795839590272, -19.15521520033831493 ) ) ;
#22982 = CARTESIAN_POINT ( 'NONE',  ( 109.4407702545248355, 0.1403307496149616695, -11.32035403202665336 ) ) ;
#22983 = DIRECTION ( 'NONE',  ( 0.000000000000000000, -0.9242245927363028635, -0.3818493186865930533 ) ) ;
#22984 = CYLINDRICAL_SURFACE ( 'NONE', #9358, 5.999999999999997335 ) ;
#22985 = CARTESIAN_POINT ( 'NONE',  ( 115.9162281442453093, -5.574606645277164318, -18.38911715685844683 ) ) ;
#22986 = CARTESIAN_POINT ( 'NONE',  ( 85.82015659721905365, -26.75858941326842810, -11.54476601486570964 ) ) ;
#22987 = CARTESIAN_POINT ( 'NONE',  ( 115.4831921295247952, -9.868328341294093420, -13.39321520033831447 ) ) ;
#22988 = EDGE_LOOP ( 'NONE', ( #17133, #39952, #14674, #6521 ) ) ;
#22989 = CARTESIAN_POINT ( 'NONE',  ( 124.1415948109119540, -3.505236298600246325, -18.68346056562440793 ) ) ;
#22990 = CARTESIAN_POINT ( 'NONE',  ( 120.4379860609119675, -3.387241619883791355, -18.17469012370385073 ) ) ;
#22991 = CARTESIAN_POINT ( 'NONE',  ( 122.2437673109119629, 0.2312338769422704887, -16.08380026872395874 ) ) ;
#22992 = ORIENTED_EDGE ( 'NONE', *, *, #43882, .F. ) ;
#22993 = CARTESIAN_POINT ( 'NONE',  ( 123.8290266009169045, -8.403782945130243931, -17.37684090985457885 ) ) ;
#22994 = CARTESIAN_POINT ( 'NONE',  ( 116.9101653964060858, -11.61644908211846605, -21.52136771687170480 ) ) ;
#22995 = ORIENTED_EDGE ( 'NONE', *, *, #5061, .F. ) ;
#22996 = CARTESIAN_POINT ( 'NONE',  ( 117.6180281442453150, -0.4660016031367893996, -10.09054647747474043 ) ) ;
#22997 = CARTESIAN_POINT ( 'NONE',  ( 125.2761281442453054, 0.4262465694468514643, -12.03445270309931736 ) ) ;
#22998 = CARTESIAN_POINT ( 'NONE',  ( 114.0442481442453300, -7.643976991954077427, -18.09477374809248928 ) ) ;
#22999 = CARTESIAN_POINT ( 'NONE',  ( 90.33554924625337890, -26.75858941326842810, -11.54476601486570964 ) ) ;
#23000 = FACE_OUTER_BOUND ( 'NONE', #17572, .T. ) ;
#23001 = CARTESIAN_POINT ( 'NONE',  ( 115.6893214775786447, 0.5811942927096154232, -14.16772938898807155 ) ) ;
#23002 = CARTESIAN_POINT ( 'NONE',  ( 113.0523327545247838, -6.936859964151250502, -8.388885654883777576 ) ) ;
#23003 = CARTESIAN_POINT ( 'NONE',  ( 125.8433948109119456, -1.834011780172310813, -8.268836392978581529 ) ) ;
#23004 = FACE_OUTER_BOUND ( 'NONE', #30143, .T. ) ;
#23005 = ORIENTED_EDGE ( 'NONE', *, *, #38423, .T. ) ;
#23006 = PRESENTATION_LAYER_ASSIGNMENT (  '', '', ( #2631 ) ) ;
#23007 = CARTESIAN_POINT ( 'NONE',  ( 114.8384214775786489, 0.9020085738987339008, -11.91225656197089222 ) ) ;
#23008 = CARTESIAN_POINT ( 'NONE',  ( 115.2355081442453155, 0.1319031606808879209, -14.10382304977623669 ) ) ;
#23009 = CIRCLE ( 'NONE', #32438, 2.999999999999999556 ) ;
#23010 = CARTESIAN_POINT ( 'NONE',  ( 70.36267391504962632, -5.685877709920933221, -4.893215200338314474 ) ) ;
#23011 = CARTESIAN_POINT ( 'NONE',  ( 125.7866681442452688, -8.899110576539710493, -16.42337572283490132 ) ) ;
#23012 = ORIENTED_EDGE ( 'NONE', *, *, #24771, .F. ) ;
#23013 = CARTESIAN_POINT ( 'NONE',  ( 121.8158014775786171, -5.638512984488999180, -18.83840828888717311 ) ) ;
#23014 = AXIS2_PLACEMENT_3D ( 'NONE', #9897, #10945, #4311 ) ;
#23015 = DIRECTION ( 'NONE',  ( 0.3090169943749413450, -0.8789898214420970302, -0.3631602827797496547 ) ) ;
#23016 = CARTESIAN_POINT ( 'NONE',  ( 119.8115785246182412, -4.413224050718078217, -8.020953925612355206 ) ) ;
#23017 = CARTESIAN_POINT ( 'NONE',  ( 124.4330791887808516, -1.261433387662844297, -20.45354594542311588 ) ) ;
#23018 = CARTESIAN_POINT ( 'NONE',  ( 123.6047240866468684, -4.379635970098219921, -15.28718505432590113 ) ) ;
#23019 = CARTESIAN_POINT ( 'NONE',  ( 113.2500748109119968, -3.505236298600246325, -18.68346056562440793 ) ) ;
#23020 = B_SPLINE_CURVE_WITH_KNOTS ( 'NONE', 3,
 ( #44632, #13830, #13396, #38210, #3995, #31592, #37769, #6542, #17041, #31367 ),
 .UNSPECIFIED., .F., .F.,
 ( 4, 3, 3, 4 ),
 ( 6.254634441385499976E-18, 0.0002476486541971024665, 0.0004952973025691019462, 0.0009610892161188130988 ),
 .UNSPECIFIED. ) ;
#23021 = DIRECTION ( 'NONE',  ( 0.9609149988134837450, -0.1028163501681639419, 0.2570431154366518145 ) ) ;
#23022 = CARTESIAN_POINT ( 'NONE',  ( 125.0921134857867827, -3.652124968999053145, -20.77843945995303088 ) ) ;
#23023 = AXIS2_PLACEMENT_3D ( 'NONE', #40209, #16040, #2112 ) ;
#23024 = CARTESIAN_POINT ( 'NONE',  ( 125.5597614775786326, -1.561330072975669392, -17.79121239304076951 ) ) ;
#23025 = APPLICATION_CONTEXT ( 'automotive_design' ) ;
#23026 = CARTESIAN_POINT ( 'NONE',  ( 112.2289948109119848, -1.834011780172310813, -8.268836392978581529 ) ) ;
#23027 = CARTESIAN_POINT ( 'NONE',  ( 121.8270485609119760, -0.08252387247370887580, -11.91645802438286417 ) ) ;
#23028 = CARTESIAN_POINT ( 'NONE',  ( 113.6471614775786492, -5.638512984488999180, -18.83840828888717311 ) ) ;
#23029 = CARTESIAN_POINT ( 'NONE',  ( 117.1074881442453233, 0.4262465694468514643, -12.03445270309931736 ) ) ;
#23030 = CARTESIAN_POINT ( 'NONE',  ( 121.6456214775786293, -10.63000616557722466, -14.87417383870573495 ) ) ;
#23031 = CARTESIAN_POINT ( 'NONE',  ( 121.2485348109119769, -0.4660016031367893996, -10.09054647747474043 ) ) ;
#23032 = VERTEX_POINT ( 'NONE', #22456 ) ;
#23033 = DIRECTION ( 'NONE',  ( 1.000000000000000000, 0.000000000000000000, -0.000000000000000000 ) ) ;
#23034 = CARTESIAN_POINT ( 'NONE',  ( 112.2188952545247531, 0.8980012041604421569, -11.00651665394454071 ) ) ;
#23035 = CIRCLE ( 'NONE', #9939, 5.000000000000004441 ) ;
#23036 = CARTESIAN_POINT ( 'NONE',  ( 107.9822546295247889, -4.863998795839590272, -18.39754474579285315 ) ) ;
#23037 = CARTESIAN_POINT ( 'NONE',  ( 109.6491296295247793, -4.863998795839590272, -8.388885654883775800 ) ) ;
#23038 = CARTESIAN_POINT ( 'NONE',  ( 109.5796765045248264, -7.250697342233347165, -19.15521520033832203 ) ) ;
#23039 = CARTESIAN_POINT ( 'NONE',  ( 119.1496481442453046, -3.383040157471821630, -19.15922257007629170 ) ) ;
#23040 = ORIENTED_EDGE ( 'NONE', *, *, #22472, .F. ) ;
#23041 = CARTESIAN_POINT ( 'NONE',  ( 125.2761281442453054, -10.63000616557722466, -14.87417383870573495 ) ) ;
#23042 = CARTESIAN_POINT ( 'NONE',  ( 109.2294421295247275, -8.715624763370474426, -9.113786294776467400 ) ) ;
#23043 = CARTESIAN_POINT ( 'NONE',  ( 120.7432071540078340, -2.348512537728041583, -17.99195118506215962 ) ) ;
#23044 = CARTESIAN_POINT ( 'NONE',  ( 115.5758681442453053, -7.894159318335828068, -9.358103419637847864 ) ) ;
#23045 = EDGE_CURVE ( 'NONE', #28442, #10907, #29526, .T. ) ;
#23046 = CARTESIAN_POINT ( 'NONE',  ( 107.5655358795247736, -8.402594152722688392, -9.854619843455216355 ) ) ;
#23047 = CIRCLE ( 'NONE', #15044, 1.499999999999999556 ) ;
#23048 = CARTESIAN_POINT ( 'NONE',  ( 121.5888948109119809, -10.30919188438810075, -12.61870101168855918 ) ) ;
#23049 = CARTESIAN_POINT ( 'NONE',  ( 112.0105358795247810, -0.7896495226426338832, -17.46756447353520159 ) ) ;
#23050 = FACE_OUTER_BOUND ( 'NONE', #8787, .T. ) ;
#23051 = ORIENTED_EDGE ( 'NONE', *, *, #30594, .F. ) ;
#23052 = CARTESIAN_POINT ( 'NONE',  ( 124.5059548109119731, -9.675232987814487373, -12.03232374619203249 ) ) ;
#23053 = CARTESIAN_POINT ( 'NONE',  ( 122.6667014775786413, -2.084020599724406786, -8.691656652584148546 ) ) ;
#23054 = CARTESIAN_POINT ( 'NONE',  ( 118.7525614775786380, -8.166667518702819706, -8.995218007635861213 ) ) ;
#23055 = CARTESIAN_POINT ( 'NONE',  ( 114.2144281442453178, -1.833838273342658809, -17.42832698103878286 ) ) ;
#23056 =( BOUNDED_CURVE ( )  B_SPLINE_CURVE ( 2, ( #8578, #19735, #33620, #13581, #20650 ),
 .UNSPECIFIED., .F., .T. ) 
 B_SPLINE_CURVE_WITH_KNOTS ( ( 3, 2, 3 ),
 ( 0.06250000000000000000, 0.07031250000000000000, 0.07662175834314119416 ),
 .UNSPECIFIED. ) 
 CURVE ( )  GEOMETRIC_REPRESENTATION_ITEM ( )  RATIONAL_B_SPLINE_CURVE ( ( 1.000000000000000000, 0.9238795325112869605, 1.000000000000000000, 0.9385262470928680267, 0.9763430640195970289 ) ) 
 REPRESENTATION_ITEM ( '' )  );
#23057 = CARTESIAN_POINT ( 'NONE',  ( 116.1998614775786507, -10.63000616557722466, -14.87417383870573495 ) ) ;
#23058 = LINE ( 'NONE', #5714, #40975 ) ;
#23059 = CARTESIAN_POINT ( 'NONE',  ( 121.7023481442452777, -0.8288870151387760510, -10.36305467784173118 ) ) ;
#23060 = CARTESIAN_POINT ( 'NONE',  ( 117.9583881442453048, 0.1319031606808879209, -14.10382304977623669 ) ) ;
#23061 = ORIENTED_EDGE ( 'NONE', *, *, #36448, .F. ) ;
#23062 = LINE ( 'NONE', #23754, #11797 ) ;
#23063 = VECTOR ( 'NONE', #3049, 1000.000000000000000 ) ;
#23064 = CARTESIAN_POINT ( 'NONE',  ( 113.6471614775786492, -5.638512984488999180, -18.83840828888717311 ) ) ;
#23065 = CARTESIAN_POINT ( 'NONE',  ( 122.3830681442452857, -1.833838273342659697, -17.42832698103878286 ) ) ;
#23066 = VERTEX_POINT ( 'NONE', #40011 ) ;
#23067 = CARTESIAN_POINT ( 'NONE',  ( 124.7440798109119697, -7.200787124940443817, -17.81845355600750835 ) ) ;
#23068 = CARTESIAN_POINT ( 'NONE',  ( 119.2631014775786298, 0.2603800115204892296, -16.42320221600525088 ) ) ;
#23069 = CARTESIAN_POINT ( 'NONE',  ( 111.1770983795247787, -0.7896495226426338832, -9.318865927141430916 ) ) ;
#23070 = CARTESIAN_POINT ( 'NONE',  ( 116.8238548109119819, -5.574606645277164318, -18.38911715685844683 ) ) ;
#23071 = EDGE_CURVE ( 'NONE', #28016, #9382, #8776, .T. ) ;
#23072 = VERTEX_POINT ( 'NONE', #29746 ) ;
#23073 = ORIENTED_EDGE ( 'NONE', *, *, #12309, .T. ) ;
#23074 = CARTESIAN_POINT ( 'NONE',  ( 124.5954081442453116, -6.222761293078241884, -8.102969835052219238 ) ) ;
#23075 = CARTESIAN_POINT ( 'NONE',  ( 119.9438214775786378, -2.084020599724406786, -8.691656652584148546 ) ) ;
#23076 = CARTESIAN_POINT ( 'NONE',  ( 65.83173732663925648, -15.38336477915846245, -16.39321520033830737 ) ) ;
#23077 = EDGE_CURVE ( 'NONE', #10999, #41325, #7566, .T. ) ;
#23078 = AXIS2_PLACEMENT_3D ( 'NONE', #44002, #4782, #38046 ) ;
#23079 = CARTESIAN_POINT ( 'NONE',  ( 85.82015659721905365, -25.99489077589524300, -13.39321520033831625 ) ) ;
#23080 = EDGE_CURVE ( 'NONE', #18545, #20614, #30134, .T. ) ;
#23081 = CARTESIAN_POINT ( 'NONE',  ( 117.8449348109119938, -8.166667518702817929, -8.995218007635861213 ) ) ;
#23082 = CARTESIAN_POINT ( 'NONE',  ( 108.3295202545248657, -10.62599879583958717, -15.77991374673208469 ) ) ;
#23083 = CARTESIAN_POINT ( 'NONE',  ( 115.4056881442453459, -7.893985811506177619, -18.51759400769804742 ) ) ;
#23085 = CARTESIAN_POINT ( 'NONE',  ( 116.3133148109120043, -2.084020599724406786, -8.691656652584148546 ) ) ;
#23084 = CARTESIAN_POINT ( 'NONE',  ( 114.6682414775786469, -1.561330072975668060, -17.79121239304076596 ) ) ;
#23086 = CARTESIAN_POINT ( 'NONE',  ( 123.5743281442453139, -2.084020599724406786, -8.691656652584148546 ) ) ;
#23087 = LINE ( 'NONE', #33321, #41513 ) ;
#23088 = EDGE_LOOP ( 'NONE', ( #44058, #14991, #31441, #44469, #20780, #20218, #31635, #10118, #31397 ) ) ;
#23089 = CARTESIAN_POINT ( 'NONE',  ( 122.2128881442453263, -7.643976991954077427, -18.09477374809248928 ) ) ;
#23090 = DIRECTION ( 'NONE',  ( -1.000000000000000000, 0.000000000000000000, 0.000000000000000000 ) ) ;
#23091 = EDGE_CURVE ( 'NONE', #34606, #25201, #39905, .T. ) ;
#23092 = CARTESIAN_POINT ( 'NONE',  ( 113.7414098793805408, -2.191907684172563986, -18.20049396185734025 ) ) ;
#23093 = CARTESIAN_POINT ( 'NONE',  ( 113.6079577545248043, -7.250697342233347165, -7.631215200338321125 ) ) ;
#23094 = CARTESIAN_POINT ( 'NONE',  ( 115.3442858795247759, -8.402594152722688392, -9.854619843455216355 ) ) ;
#23095 = CARTESIAN_POINT ( 'NONE',  ( 110.7603796295247918, -4.863998795839590272, -19.15521520033831493 ) ) ;
#23096 = CONICAL_SURFACE ( 'NONE', #33259, 5.999999999999997335, 0.4636476090008060935 ) ;
#23097 = CARTESIAN_POINT ( 'NONE',  ( 123.1772414775786189, -4.089484607189486809, -7.948022111789456723 ) ) ;
#23098 = ORIENTED_EDGE ( 'NONE', *, *, #34492, .F. ) ;
#23099 = EDGE_CURVE ( 'NONE', #34005, #11415, #31189, .T. ) ;
#23100 = CARTESIAN_POINT ( 'NONE',  ( 119.3198281442452924, 0.5811942927096110934, -14.16772938898807510 ) ) ;
#23101 = DIRECTION ( 'NONE',  ( -0.000000000000000000, -0.9284778069183721172, -0.3713878862591650232 ) ) ;
#23102 = CARTESIAN_POINT ( 'NONE',  ( 108.3989733795248753, -8.938348069036489818, -17.46756447353520159 ) ) ;
#23103 = CARTESIAN_POINT ( 'NONE',  ( 119.3198281442452924, 0.5811942927096110934, -14.16772938898807510 ) ) ;
#23104 = EDGE_CURVE ( 'NONE', #16491, #19163, #13413, .T. ) ;
#23105 = EDGE_CURVE ( 'NONE', #44717, #1202, #26162, .T. ) ;
#23106 = CARTESIAN_POINT ( 'NONE',  ( 120.8514481442452961, -7.893985811506177619, -18.51759400769804742 ) ) ;
#23107 = CARTESIAN_POINT ( 'NONE',  ( 64.65782898596719974, -2.683267933343334910, -18.61496147612403362 ) ) ;
#23108 = FACE_OUTER_BOUND ( 'NONE', #13024, .T. ) ;
#23109 = CARTESIAN_POINT ( 'NONE',  ( 119.6045485609119794, -0.08252387247370887580, -11.91645802438286417 ) ) ;
#23110 = VECTOR ( 'NONE', #9062, 1000.000000000000000 ) ;
#23111 = EDGE_LOOP ( 'NONE', ( #32392, #7281 ) ) ;
#23112 = CARTESIAN_POINT ( 'NONE',  ( -2.063229709340284046, -6.903538917046990520, -7.827879352907993749 ) ) ;
#23113 = CARTESIAN_POINT ( 'NONE',  ( 114.3898204873411970, -2.348512537728063787, -17.99195118506216318 ) ) ;
#23114 = CARTESIAN_POINT ( 'NONE',  ( 122.4965214775786251, 0.1319031606808879209, -14.10382304977623669 ) ) ;
#23115 = CARTESIAN_POINT ( 'NONE',  ( 116.3166296295247832, -4.863998795839590272, -19.15521520033831493 ) ) ;
#23116 = CARTESIAN_POINT ( 'NONE',  ( 112.9828796295247884, -4.863998795839590272, -8.388885654883775800 ) ) ;
#23117 = CARTESIAN_POINT ( 'NONE',  ( 116.1998614775786507, 0.4262465694468514643, -12.03445270309931736 ) ) ;
#23118 = CARTESIAN_POINT ( 'NONE',  ( 138.2184548109119930, -2.458068653496962686, -15.34808096303632396 ) ) ;
#23119 = CARTESIAN_POINT ( 'NONE',  ( 68.96620373265562876, -25.90251568920598757, -5.893215200338315363 ) ) ;
#23120 = CARTESIAN_POINT ( 'NONE',  ( 113.1933481442453058, -5.574606645277164318, -18.38911715685844683 ) ) ;
#23121 = CARTESIAN_POINT ( 'NONE',  ( 122.7801548109119665, -3.383040157471821630, -19.15922257007629170 ) ) ;
#23122 = ORIENTED_EDGE ( 'NONE', *, *, #28259, .T. ) ;
#23123 =( GEOMETRIC_REPRESENTATION_CONTEXT ( 3 ) GLOBAL_UNCERTAINTY_ASSIGNED_CONTEXT ( ( #17726 ) ) GLOBAL_UNIT_ASSIGNED_CONTEXT ( ( #21341, #17475, #31598 ) ) REPRESENTATION_CONTEXT ( 'NONE', 'WORKASPACE' ) );
#23124 = CARTESIAN_POINT ( 'NONE',  ( 122.0994348109119443, -10.15424416112533912, -14.75197769757731336 ) ) ;
#23125 = CARTESIAN_POINT ( 'NONE',  ( 114.8384214775786489, 0.9020085738987339008, -11.91225656197089222 ) ) ;
#23126 = CARTESIAN_POINT ( 'NONE',  ( 123.6877814775786533, -3.383040157471821630, -19.15922257007629170 ) ) ;
#23127 = B_SPLINE_CURVE_WITH_KNOTS ( 'NONE', 3,
 ( #14948, #19037, #1700, #11534 ),
 .UNSPECIFIED., .F., .F.,
 ( 4, 4 ),
 ( 3.976470764362284670E-06, 0.0005769793764277350448 ),
 .UNSPECIFIED. ) ;
#23128 = CARTESIAN_POINT ( 'NONE',  ( 122.7801548109119665, -6.222761293078241884, -8.102969835052219238 ) ) ;
#23129 = EDGE_LOOP ( 'NONE', ( #15383, #21667 ) ) ;
#23130 = CARTESIAN_POINT ( 'NONE',  ( 123.7184548109119788, -5.764726629347491027, -12.19376142051037348 ) ) ;
#23131 = CARTESIAN_POINT ( 'NONE',  ( 122.6667014775786413, -7.893985811506177619, -18.51759400769804742 ) ) ;
#23132 = CARTESIAN_POINT ( 'NONE',  ( 113.8173414775786512, -9.565557343593413364, -10.61323700422348004 ) ) ;
#23133 = AXIS2_PLACEMENT_3D ( 'NONE', #42724, #8062, #15801 ) ;
#23134 = CARTESIAN_POINT ( 'NONE',  ( 123.6310548109119765, -5.638512984488999180, -18.83840828888717311 ) ) ;
#23135 = CARTESIAN_POINT ( 'NONE',  ( 108.0517077545248696, -7.250697342233347165, -7.631215200338321125 ) ) ;
#23136 = CARTESIAN_POINT ( 'NONE',  ( 121.2019704359119743, -10.25716656981731489, -12.88942061488890545 ) ) ;
#23137 = EDGE_LOOP ( 'NONE', ( #4768, #3493, #11442, #24687, #43994 ) ) ;
#23138 = CARTESIAN_POINT ( 'NONE',  ( 136.7822455296790736, -0.9253760310430724223, -17.38909034558905020 ) ) ;
#23139 = EDGE_CURVE ( 'NONE', #11067, #1412, #33923, .T. ) ;
#23140 = CARTESIAN_POINT ( 'NONE',  ( 109.5102233795247884, -1.325403438956436419, -9.854619843455211026 ) ) ;
#23141 = FACE_OUTER_BOUND ( 'NONE', #7598, .T. ) ;
#23142 = CARTESIAN_POINT ( 'NONE',  ( 120.7947214775786193, -0.8288870151387760510, -10.36305467784173118 ) ) ;
#23143 = CARTESIAN_POINT ( 'NONE',  ( 113.5904348109119866, -2.084020599724406786, -8.691656652584148546 ) ) ;
#23144 = CARTESIAN_POINT ( 'NONE',  ( 125.7866681442453256, -8.899110576539104756, -16.42337572283570424 ) ) ;
#23145 = VERTEX_POINT ( 'NONE', #35399 ) ;
#23146 = DIRECTION ( 'NONE',  ( 0.7871354856660198740, 0.4483307682966886643, 0.4235767337848242442 ) ) ;
#23147 = CARTESIAN_POINT ( 'NONE',  ( 118.1285681442453068, -2.084020599724406786, -8.691656652584148546 ) ) ;
#23148 = CARTESIAN_POINT ( 'NONE',  ( 73.07463722459043254, -61.28190943231786036, -36.82105141712754914 ) ) ;
#23149 = CARTESIAN_POINT ( 'NONE',  ( 68.14371629974728251, -1.351251493923715685, -10.39321520033831625 ) ) ;
#23150 = FACE_BOUND ( 'NONE', #8121, .T. ) ;
#23152 = CARTESIAN_POINT ( 'NONE',  ( 123.9714148109119805, -0.4660016031367893996, -10.09054647747474043 ) ) ;
#23151 = CARTESIAN_POINT ( 'NONE',  ( 114.0977889883689897, 0.3193521225029610777, -12.14321520033831625 ) ) ;
#23153 = CARTESIAN_POINT ( 'NONE',  ( 122.1561614775786353, -8.899110576539710493, -16.42337572283490132 ) ) ;
#23154 = VERTEX_POINT ( 'NONE', #6939 ) ;
#23155 = CARTESIAN_POINT ( 'NONE',  ( 119.2255797424434149, -0.9924539043446216624, -17.29976612834909133 ) ) ;
#23156 = CARTESIAN_POINT ( 'NONE',  ( 125.9568481442452850, -6.344957434206665248, -7.627207830600338134 ) ) ;
#23157 = CARTESIAN_POINT ( 'NONE',  ( 110.1353015045248469, -6.936859964151250502, -18.39754474579286025 ) ) ;
#23158 = ADVANCED_FACE ( 'NONE', ( #14449 ), #3725, .F. ) ;
#23159 = CARTESIAN_POINT ( 'NONE',  ( 125.4463081442452932, -4.153390946401325223, -8.397313243818185668 ) ) ;
#23160 = CARTESIAN_POINT ( 'NONE',  ( 118.2420214775786320, -6.222761293078241884, -8.102969835052219238 ) ) ;
#23161 = CARTESIAN_POINT ( 'NONE',  ( 125.2183010572640853, 1.181151835247190141, -17.51410646645848956 ) ) ;
#23162 = CARTESIAN_POINT ( 'NONE',  ( 112.9828796295247884, -4.863998795839590272, -8.388885654883775800 ) ) ;
#23163 = CARTESIAN_POINT ( 'NONE',  ( -7.917624645353497748, -12.21642755857638818, -8.593215200338315540 ) ) ;
#23164 = ADVANCED_FACE ( 'NONE', ( #311 ), #41612, .F. ) ;
#23165 = CARTESIAN_POINT ( 'NONE',  ( 96.54708369096698561, -24.20446030063578391, -12.09626349990295147 ) ) ;
#23166 = CARTESIAN_POINT ( 'NONE',  ( 114.2144281442453178, -1.833838273342658809, -17.42832698103878286 ) ) ;
#23167 = CIRCLE ( 'NONE', #23891, 2.000000000000000444 ) ;
#23168 = CARTESIAN_POINT ( 'NONE',  ( 110.4131140045248287, -10.62599879583958717, -11.00651665394454604 ) ) ;
#23169 = CARTESIAN_POINT ( 'NONE',  ( -13.32377113153209791, -5.100909530930219482, -18.19321520033831874 ) ) ;
#23170 = CARTESIAN_POINT ( 'NONE',  ( 114.3024890045248156, 0.8980012041604421569, -15.77991374673208469 ) ) ;
#23171 = CARTESIAN_POINT ( 'NONE',  ( 122.1561614775786353, -0.4660016031367893996, -10.09054647747474043 ) ) ;
#23172 = CARTESIAN_POINT ( 'NONE',  ( 121.4754414775786131, -8.166667518702819706, -8.995218007635861213 ) ) ;
#23173 = CARTESIAN_POINT ( 'NONE',  ( 119.6811727111058588, -1.267766418764730840, -16.93314635290706605 ) ) ;
#23174 = EDGE_CURVE ( 'NONE', #24392, #40113, #4314, .T. ) ;
#23175 = CARTESIAN_POINT ( 'NONE',  ( 116.1998614775786507, -10.63000616557722466, -14.87417383870573495 ) ) ;
#23176 = DIRECTION ( 'NONE',  ( 0.000000000000000000, 0.9284778069183717841, 0.3713878862591654673 ) ) ;
#23177 = ORIENTED_EDGE ( 'NONE', *, *, #17225, .F. ) ;
#23178 = CARTESIAN_POINT ( 'NONE',  ( 112.9097148109120070, -9.565557343593413364, -10.61323700422348004 ) ) ;
#23179 = CARTESIAN_POINT ( 'NONE',  ( 112.7962614775786676, -6.222761293078241884, -8.102969835052219238 ) ) ;
#23180 = CARTESIAN_POINT ( 'NONE',  ( 120.5110881442453206, -6.344957434206665248, -7.627207830600338134 ) ) ;
#23181 = CARTESIAN_POINT ( 'NONE',  ( 124.0281414775786146, -7.643976991954077427, -18.09477374809248928 ) ) ;
#23182 = CARTESIAN_POINT ( 'NONE',  ( 112.6260814775786514, -0.8288870151387760510, -10.36305467784173118 ) ) ;
#23183 = EDGE_LOOP ( 'NONE', ( #43639, #23703, #1552 ) ) ;
#23184 = CARTESIAN_POINT ( 'NONE',  ( 116.1431348109119881, 0.1319031606808879209, -14.10382304977623669 ) ) ;
#23185 = CARTESIAN_POINT ( 'NONE',  ( 125.9568481442452850, -6.344957434206665248, -7.627207830600338134 ) ) ;
#23186 = CARTESIAN_POINT ( 'NONE',  ( 108.6073327545248048, -2.477300249445798297, -19.15521520033831138 ) ) ;
#23187 = CARTESIAN_POINT ( 'NONE',  ( 120.4543614775786295, -5.574606645277164318, -18.38911715685844683 ) ) ;
#23188 = CARTESIAN_POINT ( 'NONE',  ( 116.8211612789303473, -1.788438657886855632, -17.61956049856755158 ) ) ;
#23189 = DIRECTION ( 'NONE',  ( -0.000000000000000000, -0.9284778069183718952, -0.3713878862591649677 ) ) ;
#23190 = ORIENTED_EDGE ( 'NONE', *, *, #14712, .T. ) ;
#23191 = CARTESIAN_POINT ( 'NONE',  ( 122.0354079359119908, -4.360204210389833968, -8.000047426360245240 ) ) ;
#23192 = CARTESIAN_POINT ( 'NONE',  ( 124.6521348109119884, -1.561330072975668948, -17.79121239304076951 ) ) ;
#23193 = CARTESIAN_POINT ( 'NONE',  ( 112.9134265045247787, -2.791137627527939813, -8.388885654883754484 ) ) ;
#23194 = DIRECTION ( 'NONE',  ( 0.9609149988134834119, -0.1028163501681648995, 0.2570431154366529802 ) ) ;
#23195 = AXIS2_PLACEMENT_3D ( 'NONE', #877, #42167, #14345 ) ;
#23196 = CARTESIAN_POINT ( 'NONE',  ( 122.2437673109119629, 0.2312338769422687679, -16.08380026872396229 ) ) ;
#23197 = CARTESIAN_POINT ( 'NONE',  ( 70.89841814381148311, -68.89136543047671069, -37.69090763720760151 ) ) ;
#23198 = CARTESIAN_POINT ( 'NONE',  ( 108.8851452545248151, -9.868328341294098749, -15.46607636864997204 ) ) ;
#23199 = ADVANCED_FACE ( 'NONE', ( #27471 ), #3916, .T. ) ;
#23200 = CARTESIAN_POINT ( 'NONE',  ( 78.75330084444993872, 4.432659906640606273, -21.58937828823235350 ) ) ;
#23201 = CARTESIAN_POINT ( 'NONE',  ( 136.4689272580752686, -7.050714571525749541, -18.72418924296322729 ) ) ;
#23202 = DIRECTION ( 'NONE',  ( -0.000000000000000000, -0.9284778069183720062, -0.3713878862591650232 ) ) ;
#23203 = CARTESIAN_POINT ( 'NONE',  ( 125.9001214775786224, -4.089484607189486809, -7.948022111789456723 ) ) ;
#23204 = CARTESIAN_POINT ( 'NONE',  ( 117.4478481442453131, -9.565557343593413364, -10.61323700422348004 ) ) ;
#23205 = CARTESIAN_POINT ( 'NONE',  ( 119.7434548109119845, 0.1464806637125226352, -15.28762191210849153 ) ) ;
#23206 = EDGE_LOOP ( 'NONE', ( #39353, #24621, #12147, #2482, #21286 ) ) ;
#23207 = CARTESIAN_POINT ( 'NONE',  ( 124.0848681442452772, -4.089484607189486809, -7.948022111789456723 ) ) ;
#23208 = CARTESIAN_POINT ( 'NONE',  ( 115.8027748109119841, -0.4660016031367893996, -10.09054647747474043 ) ) ;
#23209 = CARTESIAN_POINT ( 'NONE',  ( 116.5249890045247980, -9.868328341294098749, -11.32035403202665869 ) ) ;
#23210 = CARTESIAN_POINT ( 'NONE',  ( 112.1722681442453222, -8.899110576539710493, -16.42337572283490132 ) ) ;
#23211 = CARTESIAN_POINT ( 'NONE',  ( 122.4397948109119767, -0.1624402480850797581, -16.17319339645315424 ) ) ;
#23212 = CARTESIAN_POINT ( 'NONE',  ( 125.7866681442452688, -0.4660016031367893996, -10.09054647747474043 ) ) ;
#23213 = CARTESIAN_POINT ( 'NONE',  ( 106.2459265045248173, -2.791137627527939813, -8.388885654883777576 ) ) ;
#23214 = CARTESIAN_POINT ( 'NONE',  ( 111.1770983795247787, -8.402594152722688392, -16.93181055722141792 ) ) ;
#23215 = DIRECTION ( 'NONE',  ( 1.000000000000000000, 0.000000000000000000, -0.000000000000000000 ) ) ;
#23216 = CARTESIAN_POINT ( 'NONE',  ( 117.6180281442453150, -8.899110576539710493, -16.42337572283490132 ) ) ;
#23217 = CARTESIAN_POINT ( 'NONE',  ( 117.6180281442453150, -8.899110576539710493, -16.42337572283490132 ) ) ;
#23218 = ADVANCED_FACE ( 'NONE', ( #21284 ), #31766, .T. ) ;
#23219 = CARTESIAN_POINT ( 'NONE',  ( 113.2987212410415765, 0.7607806665037644134, -12.14321520033829493 ) ) ;
#23220 = CARTESIAN_POINT ( 'NONE',  ( 111.8716296295247901, -4.863998795839590272, -8.388885654883775800 ) ) ;
#23221 = ORIENTED_EDGE ( 'NONE', *, *, #37007, .F. ) ;
#23222 = CARTESIAN_POINT ( 'NONE',  ( 122.9503348109119827, -9.859900752359369136, -12.68260735090035318 ) ) ;
#23223 = CARTESIAN_POINT ( 'NONE',  ( 126.5241148109119393, -9.565557343593413364, -10.61323700422348004 ) ) ;
#23224 = CARTESIAN_POINT ( 'NONE',  ( 121.9659548109119811, -7.554583864224885481, -18.48844787311982785 ) ) ;
#23225 = CARTESIAN_POINT ( 'NONE',  ( 120.8547048109119686, -2.527210466738041728, -8.967976844669124148 ) ) ;
#23226 = VERTEX_POINT ( 'NONE', #7149 ) ;
#23227 = CARTESIAN_POINT ( 'NONE',  ( 116.6117576306022841, -11.86965430100211805, -21.21901607071682605 ) ) ;
#23228 = ORIENTED_EDGE ( 'NONE', *, *, #1314, .T. ) ;
#23229 = CARTESIAN_POINT ( 'NONE',  ( 117.3343948109119737, -3.383040157471821630, -19.15922257007629170 ) ) ;
#23230 = CARTESIAN_POINT ( 'NONE',  ( 123.2906948109119867, -1.833838273342659697, -17.42832698103878286 ) ) ;
#23231 = CARTESIAN_POINT ( 'NONE',  ( 114.7816948109119863, -9.859900752359374465, -12.68260735090039404 ) ) ;
#23232 = FACE_OUTER_BOUND ( 'NONE', #39602, .T. ) ;
#23233 = FACE_OUTER_BOUND ( 'NONE', #37570, .T. ) ;
#23234 = CARTESIAN_POINT ( 'NONE',  ( 114.2711548109119803, -9.988377603198976828, -10.36322818467138340 ) ) ;
#23235 = CARTESIAN_POINT ( 'NONE',  ( 110.2047546295247855, -4.863998795839590272, -18.39754474579285315 ) ) ;
#23236 = EDGE_CURVE ( 'NONE', #42441, #26037, #31986, .T. ) ;
#23237 = CARTESIAN_POINT ( 'NONE',  ( 124.6521348109119884, -1.561330072975668948, -17.79121239304076951 ) ) ;
#23238 = FACE_OUTER_BOUND ( 'NONE', #14373, .T. ) ;
#23239 = ORIENTED_EDGE ( 'NONE', *, *, #10985, .F. ) ;
#23240 =( BOUNDED_SURFACE ( )  B_SPLINE_SURFACE ( 1, 2, ( 
 ( #10944, #25076, #668, #35538, #21648, #32126, #1119, #15037, #42856, #25526, #39431, #8195, #22103, #35991, #19808, #19130, #22326, #2237, #16169, #36890, #29391, #18900, #36222, #43303, #4987, #5437, #5886, #9097, #12525, #12748, #12072, #25974, #8645, #22998, #37113, #40105, #26198, #33013, #33458, #30072, #39880, #5659, #40332, #26425, #40791, #43984, #23231, #29615, #12979, #12299, #22545, #36443, #2467, #16391, #26649, #40564, #32791, #43759, #19356, #1563, #19578, #9324, #33696, #8866, #30291, #44218, #26875, #15486, #5211, #1787, #15712, #36664, #43530, #22767, #33243, #2016, #15941, #29841, #27106, #41028, #37582, #27335, #3376, #24356, #38243, #23463, #44892, #7022, #23696, #20933, #23920, #44669, #34807, #37801, #44439, #30969, #38030, #37349, #31188, #3156, #20040, #9781, #17504, #2923, #9548, #6122, #24137, #17296, #10452, #3593, #17076, #31402, #45106, #34375, #6806, #6355, #20267, #10011, #34154, #41690, #20494, #13865, #6577, #27778, #171, #14087, #2693, #13652, #27558, #33922, #20714, #16623, #28004, #41471, #30517, #10230, #34593, #13205, #16854, #30745, #13431, #41253, #7913, #38687, #840, #18411, #24794, #25476, #11568, #396, #11120, #7684, #21598, #4032, #17953, #14759, #8147, #28228, #35485, #10895, #22050, #25250, #39381, #4712, #35023, #14310, #4259, #3806, #42134, #35943, #7452, #21372, #32072, #39148, #35255, #38913, #42578, #18177, #28675, #18633, #31853, #32520, #14983, #21822, #15207, #28447, #35715, #17731, #1295, #622, #41911, #14533, #42358, #11340, #31628, #10674, #25020, #24577, #4489, #32303, #38462, #1070, #7234, #28895, #42807, #21150, #32961, #25699, #8594, #23181, #39606, #19528, #26597, #40510, #39826, #2181, #40047, #1738, #11792, #29112, #9271, #33636, #8367, #22492, #40280, #2411, #1961, #36387, #37059, #43254, #5832, #43480, #19075, #19752, #12247, #18848, #5390, #12471, #22272, #5605, #22716, #15889, #36615, #43023, #36166, #25922, #5158, #4933, #8814, #19308, #26371, #9045, #15662, #43698, #29564, #26144, #33187 ),
 ( #29785, #43930, #22944, #32740, #36837, #33405, #1514, #16111, #15433, #30012, #29341, #12019, #12697, #13817, #27728, #27052, #34540, #27281, #34101, #44163, #16338, #41645, #20882, #40735, #40970, #27505, #34757, #34325, #23637, #26824, #2638, #24310, #9725, #30241, #12927, #30917, #10179, #17242, #10400, #23869, #38196, #37980, #41196, #44840, #30465, #44385, #16799, #37523, #3321, #9956, #6754, #44613, #24086, #45057, #31133, #9492, #37755, #6525, #23407, #13596, #37290, #6060, #30695, #19980, #20442, #3098, #17026, #6973, #6296, #33869, #20665, #41424, #13149, #16570, #20216, #2869, #13380, #18356, #7182, #17903, #14481, #28391, #10843, #24738, #21545, #14933, #34970, #42301, #17679, #28844, #32021, #1017, #38412, #24967, #786, #31351, #25198, #11065, #35434, #38863, #25424, #8093, #345, #38628, #10623, #7631, #4209, #14707, #28620, #21321, #18126, #14258, #3980, #42530, #21092, #41861, #39325, #27954, #39096, #125, #3758, #11290, #7866, #21773, #35665, #31800, #24525, #7403, #31577, #571, #28175, #35207, #42083, #3540, #42756, #11519, #4438, #21995, #32246, #17455, #14037, #32689, #35885, #15831, #29728, #5334, #42970, #32468, #4655, #11738, #18576, #19019, #19471, #22664, #26088, #26317, #25649, #39553, #22215, #36560, #5553, #8539, #39768, #1459, #1902, #43642, #8315, #19252, #8758, #39992, #9217, #12416, #36782, #43199, #26544, #25864, #36112, #4883, #16055, #29961, #40225, #8989, #1244, #12188, #32906, #15155, #33132, #22889, #33353, #22440, #2126, #43877, #12648, #40455, #29061, #18800, #15381, #5103, #29285, #11965, #36333, #1681, #15603, #29507, #43423, #44108, #26774, #6006, #20165, #30639, #44556, #23126, #26994, #27226, #12875, #41144, #2585, #19928, #9903, #16516, #23816, #37704, #2357, #40683, #13095, #16288, #30190, #37003, #9435, #23348, #40914, #34048, #37232, #30415, #37470, #9668, #44335, #5774, #33815, #19694, #33582, #23586, #6242, #2816, #16745, #13322, #20013, #23897, #13625, #27083, #16601, #151, #2668, #13842, #33898, #13180, #41449 ) ),
 .UNSPECIFIED., .F., .F., .T. ) 
 B_SPLINE_SURFACE_WITH_KNOTS ( ( 2, 2 ),
 ( 3, 2, 2, 2, 2, 2, 2, 2, 2, 2, 2, 2, 2, 2, 2, 2, 2, 2, 2, 2, 2, 2, 2, 2, 2, 2, 2, 2, 2, 2, 2, 2, 2, 2, 2, 2, 2, 2, 2, 2, 2, 2, 2, 2, 2, 2, 2, 2, 2, 2, 2, 2, 2, 2, 2, 2, 2, 2, 2, 2, 2, 2, 2, 2, 2, 2, 2, 2, 2, 2, 2, 2, 2, 2, 2, 2, 2, 2, 2, 2, 2, 2, 2, 2, 2, 2, 2, 2, 2, 2, 2, 2, 2, 2, 2, 2, 2, 2, 2, 2, 2, 2, 2, 2, 2, 2, 2, 2, 2, 2, 2, 2, 2, 2, 2, 2, 2, 2, 2, 2, 2, 2, 2, 2, 2, 2, 2, 2, 3 ),
 ( 0.000000000000000000, 1.000000000000000000 ),
 ( 0.000000000000000000, 0.007812500000000000000, 0.01562500000000000000, 0.02343750000000000000, 0.03125000000000000000, 0.03906250000000000000, 0.04687500000000000000, 0.05468750000000000000, 0.06250000000000000000, 0.07031250000000000000, 0.07812500000000000000, 0.08593750000000000000, 0.09375000000000000000, 0.1015625000000000000, 0.1093750000000000000, 0.1171875000000000000, 0.1250000000000000000, 0.1328125000000000000, 0.1406250000000000000, 0.1484375000000000000, 0.1562500000000000000, 0.1640625000000000000, 0.1718750000000000000, 0.1796875000000000000, 0.1875000000000000000, 0.1953125000000000000, 0.2031250000000000000, 0.2109375000000000000, 0.2187500000000000000, 0.2265625000000000000, 0.2343750000000000000, 0.2421875000000000000, 0.2500000000000000000, 0.2578125000000000000, 0.2656250000000000000, 0.2734375000000000000, 0.2812500000000000000, 0.2890625000000000000, 0.2968750000000000000, 0.3046875000000000000, 0.3125000000000000000, 0.3203125000000000000, 0.3281250000000000000, 0.3359375000000000000, 0.3437500000000000000, 0.3515625000000000000, 0.3593750000000000000, 0.3671875000000000000, 0.3750000000000000000, 0.3828125000000000000, 0.3906250000000000000, 0.3984375000000000000, 0.4062500000000000000, 0.4140625000000000000, 0.4218750000000000000, 0.4296875000000000000, 0.4375000000000000000, 0.4453125000000000000, 0.4531250000000000000, 0.4609375000000000000, 0.4687500000000000000, 0.4765625000000000000, 0.4843750000000000000, 0.4921875000000000000, 0.5000000000000000000, 0.5078125000000000000, 0.5156250000000000000, 0.5234375000000000000, 0.5312500000000000000, 0.5390625000000000000, 0.5468750000000000000, 0.5546875000000000000, 0.5625000000000000000, 0.5703125000000000000, 0.5781250000000000000, 0.5859375000000000000, 0.5937500000000000000, 0.6015625000000000000, 0.6093750000000000000, 0.6171875000000000000, 0.6250000000000000000, 0.6328125000000000000, 0.6406250000000000000, 0.6484375000000000000, 0.6562500000000000000, 0.6640625000000000000, 0.6718750000000000000, 0.6796875000000000000, 0.6875000000000000000, 0.6953125000000000000, 0.7031250000000000000, 0.7109375000000000000, 0.7187500000000000000, 0.7265625000000000000, 0.7343750000000000000, 0.7421875000000000000, 0.7500000000000000000, 0.7578125000000000000, 0.7656250000000000000, 0.7734375000000000000, 0.7812500000000000000, 0.7890625000000000000, 0.7968750000000000000, 0.8046875000000000000, 0.8125000000000000000, 0.8203125000000000000, 0.8281250000000000000, 0.8359375000000000000, 0.8437500000000000000, 0.8515625000000000000, 0.8593750000000000000, 0.8671875000000000000, 0.8750000000000000000, 0.8828125000000000000, 0.8906250000000000000, 0.8984375000000000000, 0.9062500000000000000, 0.9140625000000000000, 0.9218750000000000000, 0.9296875000000000000, 0.9375000000000000000, 0.9453125000000000000, 0.9531250000000000000, 0.9609375000000000000, 0.9687500000000000000, 0.9765625000000000000, 0.9843750000000000000, 0.9921875000000000000, 1.000000000000000000 ),
 .UNSPECIFIED. ) 
 GEOMETRIC_REPRESENTATION_ITEM ( )  RATIONAL_B_SPLINE_SURFACE ( (
 ( 1.000000000000000000, 0.9238795325112869605, 1.000000000000000000, 0.9238795325112869605, 1.000000000000000000, 0.9238795325112869605, 1.000000000000000000, 0.9238795325112869605, 1.000000000000000000, 0.9238795325112869605, 1.000000000000000000, 0.9238795325112869605, 1.000000000000000000, 0.9238795325112869605, 1.000000000000000000, 0.9238795325112869605, 1.000000000000000000, 0.9238795325112869605, 1.000000000000000000, 0.9238795325112869605, 1.000000000000000000, 0.9238795325112869605, 1.000000000000000000, 0.9238795325112869605, 1.000000000000000000, 0.9238795325112869605, 1.000000000000000000, 0.9238795325112869605, 1.000000000000000000, 0.9238795325112869605, 1.000000000000000000, 0.9238795325112869605, 1.000000000000000000, 0.9238795325112869605, 1.000000000000000000, 0.9238795325112869605, 1.000000000000000000, 0.9238795325112869605, 1.000000000000000000, 0.9238795325112869605, 1.000000000000000000, 0.9238795325112869605, 1.000000000000000000, 0.9238795325112869605, 1.000000000000000000, 0.9238795325112869605, 1.000000000000000000, 0.9238795325112869605, 1.000000000000000000, 0.9238795325112869605, 1.000000000000000000, 0.9238795325112869605, 1.000000000000000000, 0.9238795325112869605, 1.000000000000000000, 0.9238795325112869605, 1.000000000000000000, 0.9238795325112869605, 1.000000000000000000, 0.9238795325112869605, 1.000000000000000000, 0.9238795325112869605, 1.000000000000000000, 0.9238795325112869605, 1.000000000000000000, 0.9238795325112869605, 1.000000000000000000, 0.9238795325112869605, 1.000000000000000000, 0.9238795325112869605, 1.000000000000000000, 0.9238795325112869605, 1.000000000000000000, 0.9238795325112869605, 1.000000000000000000, 0.9238795325112869605, 1.000000000000000000, 0.9238795325112869605, 1.000000000000000000, 0.9238795325112869605, 1.000000000000000000, 0.9238795325112869605, 1.000000000000000000, 0.9238795325112869605, 1.000000000000000000, 0.9238795325112869605, 1.000000000000000000, 0.9238795325112869605, 1.000000000000000000, 0.9238795325112869605, 1.000000000000000000, 0.9238795325112869605, 1.000000000000000000, 0.9238795325112869605, 1.000000000000000000, 0.9238795325112869605, 1.000000000000000000, 0.9238795325112869605, 1.000000000000000000, 0.9238795325112869605, 1.000000000000000000, 0.9238795325112869605, 1.000000000000000000, 0.9238795325112869605, 1.000000000000000000, 0.9238795325112869605, 1.000000000000000000, 0.9238795325112869605, 1.000000000000000000, 0.9238795325112869605, 1.000000000000000000, 0.9238795325112869605, 1.000000000000000000, 0.9238795325112869605, 1.000000000000000000, 0.9238795325112869605, 1.000000000000000000, 0.9238795325112869605, 1.000000000000000000, 0.9238795325112869605, 1.000000000000000000, 0.9238795325112869605, 1.000000000000000000, 0.9238795325112869605, 1.000000000000000000, 0.9238795325112869605, 1.000000000000000000, 0.9238795325112869605, 1.000000000000000000, 0.9238795325112869605, 1.000000000000000000, 0.9238795325112869605, 1.000000000000000000, 0.9238795325112869605, 1.000000000000000000, 0.9238795325112869605, 1.000000000000000000, 0.9238795325112869605, 1.000000000000000000, 0.9238795325112869605, 1.000000000000000000, 0.9238795325112869605, 1.000000000000000000, 0.9238795325112869605, 1.000000000000000000, 0.9238795325112869605, 1.000000000000000000, 0.9238795325112869605, 1.000000000000000000, 0.9238795325112869605, 1.000000000000000000, 0.9238795325112869605, 1.000000000000000000, 0.9238795325112869605, 1.000000000000000000, 0.9238795325112869605, 1.000000000000000000, 0.9238795325112869605, 1.000000000000000000, 0.9238795325112869605, 1.000000000000000000, 0.9238795325112869605, 1.000000000000000000, 0.9238795325112869605, 1.000000000000000000, 0.9238795325112869605, 1.000000000000000000, 0.9238795325112869605, 1.000000000000000000, 0.9238795325112869605, 1.000000000000000000, 0.9238795325112869605, 1.000000000000000000, 0.9238795325112869605, 1.000000000000000000, 0.9238795325112869605, 1.000000000000000000, 0.9238795325112869605, 1.000000000000000000, 0.9238795325112869605, 1.000000000000000000, 0.9238795325112869605, 1.000000000000000000, 0.9238795325112869605, 1.000000000000000000, 0.9238795325112869605, 1.000000000000000000, 0.9238795325112869605, 1.000000000000000000, 0.9238795325112869605, 1.000000000000000000, 0.9238795325112869605, 1.000000000000000000, 0.9238795325112869605, 1.000000000000000000, 0.9238795325112869605, 1.000000000000000000, 0.9238795325112869605, 1.000000000000000000, 0.9238795325112869605, 1.000000000000000000, 0.9238795325112869605, 1.000000000000000000, 0.9238795325112869605, 1.000000000000000000, 0.9238795325112869605, 1.000000000000000000, 0.9238795325112869605, 1.000000000000000000, 0.9238795325112869605, 1.000000000000000000, 0.9238795325112869605, 1.000000000000000000, 0.9238795325112869605, 1.000000000000000000, 0.9238795325112869605, 1.000000000000000000, 0.9238795325112869605, 1.000000000000000000, 0.9238795325112869605, 1.000000000000000000, 0.9238795325112869605, 1.000000000000000000, 0.9238795325112869605, 1.000000000000000000, 0.9238795325112869605, 1.000000000000000000, 0.9238795325112869605, 1.000000000000000000, 0.9238795325112869605, 1.000000000000000000, 0.9238795325112869605, 1.000000000000000000, 0.9238795325112869605, 1.000000000000000000, 0.9238795325112869605, 1.000000000000000000, 0.9238795325112869605, 1.000000000000000000, 0.9238795325112869605, 1.000000000000000000, 0.9238795325112869605, 1.000000000000000000, 0.9238795325112869605, 1.000000000000000000, 0.9238795325112869605, 1.000000000000000000, 0.9238795325112869605, 1.000000000000000000, 0.9238795325112869605, 1.000000000000000000, 0.9238795325112869605, 1.000000000000000000, 0.9238795325112869605, 1.000000000000000000, 0.9238795325112869605, 1.000000000000000000),
 ( 1.000000000000000000, 0.9238795325112869605, 1.000000000000000000, 0.9238795325112869605, 1.000000000000000000, 0.9238795325112869605, 1.000000000000000000, 0.9238795325112869605, 1.000000000000000000, 0.9238795325112869605, 1.000000000000000000, 0.9238795325112869605, 1.000000000000000000, 0.9238795325112869605, 1.000000000000000000, 0.9238795325112869605, 1.000000000000000000, 0.9238795325112869605, 1.000000000000000000, 0.9238795325112869605, 1.000000000000000000, 0.9238795325112869605, 1.000000000000000000, 0.9238795325112869605, 1.000000000000000000, 0.9238795325112869605, 1.000000000000000000, 0.9238795325112869605, 1.000000000000000000, 0.9238795325112869605, 1.000000000000000000, 0.9238795325112869605, 1.000000000000000000, 0.9238795325112869605, 1.000000000000000000, 0.9238795325112869605, 1.000000000000000000, 0.9238795325112869605, 1.000000000000000000, 0.9238795325112869605, 1.000000000000000000, 0.9238795325112869605, 1.000000000000000000, 0.9238795325112869605, 1.000000000000000000, 0.9238795325112869605, 1.000000000000000000, 0.9238795325112869605, 1.000000000000000000, 0.9238795325112869605, 1.000000000000000000, 0.9238795325112869605, 1.000000000000000000, 0.9238795325112869605, 1.000000000000000000, 0.9238795325112869605, 1.000000000000000000, 0.9238795325112869605, 1.000000000000000000, 0.9238795325112869605, 1.000000000000000000, 0.9238795325112869605, 1.000000000000000000, 0.9238795325112869605, 1.000000000000000000, 0.9238795325112869605, 1.000000000000000000, 0.9238795325112869605, 1.000000000000000000, 0.9238795325112869605, 1.000000000000000000, 0.9238795325112869605, 1.000000000000000000, 0.9238795325112869605, 1.000000000000000000, 0.9238795325112869605, 1.000000000000000000, 0.9238795325112869605, 1.000000000000000000, 0.9238795325112869605, 1.000000000000000000, 0.9238795325112869605, 1.000000000000000000, 0.9238795325112869605, 1.000000000000000000, 0.9238795325112869605, 1.000000000000000000, 0.9238795325112869605, 1.000000000000000000, 0.9238795325112869605, 1.000000000000000000, 0.9238795325112869605, 1.000000000000000000, 0.9238795325112869605, 1.000000000000000000, 0.9238795325112869605, 1.000000000000000000, 0.9238795325112869605, 1.000000000000000000, 0.9238795325112869605, 1.000000000000000000, 0.9238795325112869605, 1.000000000000000000, 0.9238795325112869605, 1.000000000000000000, 0.9238795325112869605, 1.000000000000000000, 0.9238795325112869605, 1.000000000000000000, 0.9238795325112869605, 1.000000000000000000, 0.9238795325112869605, 1.000000000000000000, 0.9238795325112869605, 1.000000000000000000, 0.9238795325112869605, 1.000000000000000000, 0.9238795325112869605, 1.000000000000000000, 0.9238795325112869605, 1.000000000000000000, 0.9238795325112869605, 1.000000000000000000, 0.9238795325112869605, 1.000000000000000000, 0.9238795325112869605, 1.000000000000000000, 0.9238795325112869605, 1.000000000000000000, 0.9238795325112869605, 1.000000000000000000, 0.9238795325112869605, 1.000000000000000000, 0.9238795325112869605, 1.000000000000000000, 0.9238795325112869605, 1.000000000000000000, 0.9238795325112869605, 1.000000000000000000, 0.9238795325112869605, 1.000000000000000000, 0.9238795325112869605, 1.000000000000000000, 0.9238795325112869605, 1.000000000000000000, 0.9238795325112869605, 1.000000000000000000, 0.9238795325112869605, 1.000000000000000000, 0.9238795325112869605, 1.000000000000000000, 0.9238795325112869605, 1.000000000000000000, 0.9238795325112869605, 1.000000000000000000, 0.9238795325112869605, 1.000000000000000000, 0.9238795325112869605, 1.000000000000000000, 0.9238795325112869605, 1.000000000000000000, 0.9238795325112869605, 1.000000000000000000, 0.9238795325112869605, 1.000000000000000000, 0.9238795325112869605, 1.000000000000000000, 0.9238795325112869605, 1.000000000000000000, 0.9238795325112869605, 1.000000000000000000, 0.9238795325112869605, 1.000000000000000000, 0.9238795325112869605, 1.000000000000000000, 0.9238795325112869605, 1.000000000000000000, 0.9238795325112869605, 1.000000000000000000, 0.9238795325112869605, 1.000000000000000000, 0.9238795325112869605, 1.000000000000000000, 0.9238795325112869605, 1.000000000000000000, 0.9238795325112869605, 1.000000000000000000, 0.9238795325112869605, 1.000000000000000000, 0.9238795325112869605, 1.000000000000000000, 0.9238795325112869605, 1.000000000000000000, 0.9238795325112869605, 1.000000000000000000, 0.9238795325112869605, 1.000000000000000000, 0.9238795325112869605, 1.000000000000000000, 0.9238795325112869605, 1.000000000000000000, 0.9238795325112869605, 1.000000000000000000, 0.9238795325112869605, 1.000000000000000000, 0.9238795325112869605, 1.000000000000000000, 0.9238795325112869605, 1.000000000000000000, 0.9238795325112869605, 1.000000000000000000, 0.9238795325112869605, 1.000000000000000000, 0.9238795325112869605, 1.000000000000000000, 0.9238795325112869605, 1.000000000000000000, 0.9238795325112869605, 1.000000000000000000, 0.9238795325112869605, 1.000000000000000000, 0.9238795325112869605, 1.000000000000000000, 0.9238795325112869605, 1.000000000000000000, 0.9238795325112869605, 1.000000000000000000, 0.9238795325112869605, 1.000000000000000000, 0.9238795325112869605, 1.000000000000000000, 0.9238795325112869605, 1.000000000000000000, 0.9238795325112869605, 1.000000000000000000, 0.9238795325112869605, 1.000000000000000000, 0.9238795325112869605, 1.000000000000000000, 0.9238795325112869605, 1.000000000000000000, 0.9238795325112869605, 1.000000000000000000, 0.9238795325112869605, 1.000000000000000000, 0.9238795325112869605, 1.000000000000000000, 0.9238795325112869605, 1.000000000000000000, 0.9238795325112869605, 1.000000000000000000, 0.9238795325112869605, 1.000000000000000000, 0.9238795325112869605, 1.000000000000000000, 0.9238795325112869605, 1.000000000000000000) ) ) 
 REPRESENTATION_ITEM ( '' )  SURFACE ( )  );
#23241 = CARTESIAN_POINT ( 'NONE',  ( 112.5126281442453120, -10.30919188438810075, -12.61870101168855918 ) ) ;
#23242 = CARTESIAN_POINT ( 'NONE',  ( 113.5337081442453240, -0.8288870151387760510, -10.36305467784173118 ) ) ;
#23243 = LINE ( 'NONE', #23010, #14729 ) ;
#23244 = CARTESIAN_POINT ( 'NONE',  ( 113.4769814775786330, -10.63000616557722466, -14.87417383870573495 ) ) ;
#23245 = VERTEX_POINT ( 'NONE', #24053 ) ;
#23246 = CARTESIAN_POINT ( 'NONE',  ( 123.4041481442452834, -10.30919188438810075, -12.61870101168855918 ) ) ;
#23247 = CARTESIAN_POINT ( 'NONE',  ( 121.9470836909669913, -27.84333996136784961, -14.15691383771150136 ) ) ;
#23248 = CARTESIAN_POINT ( 'NONE',  ( 64.69189222814998175, -41.76310523276723785, -47.71602681600972318 ) ) ;
#23249 = CARTESIAN_POINT ( 'NONE',  ( 77.92559343843963404, -57.44393871073324931, -1.136555471121397209 ) ) ;
#23250 = CARTESIAN_POINT ( 'NONE',  ( 117.7314814775786260, -5.574606645277164318, -18.38911715685844683 ) ) ;
#23251 = CARTESIAN_POINT ( 'NONE',  ( 123.6018618195759160, -4.372193249654628744, -15.29709325109553930 ) ) ;
#23252 = CARTESIAN_POINT ( 'NONE',  ( 114.6682414775786469, -7.894159318335828068, -9.358103419637847864 ) ) ;
#23253 = LINE ( 'NONE', #15505, #14643 ) ;
#23254 = CARTESIAN_POINT ( 'NONE',  ( 125.1861822135562079, -1.866968678097731260, -20.11746626182562991 ) ) ;
#23255 = CARTESIAN_POINT ( 'NONE',  ( 116.1998614775786507, 0.4262465694468514643, -12.03445270309931736 ) ) ;
#23256 = CARTESIAN_POINT ( 'NONE',  ( 116.9940348109119839, -9.988377603198976828, -10.36322818467138340 ) ) ;
#23257 = CARTESIAN_POINT ( 'NONE',  ( 123.5633766859119760, -9.033780868592240054, -16.85052413769862056 ) ) ;
#23258 = CIRCLE ( 'NONE', #43634, 2.999999999999999556 ) ;
#23259 = CARTESIAN_POINT ( 'NONE',  ( 112.5693548109119888, -10.63000616557722466, -14.87417383870573495 ) ) ;
#23260 = CARTESIAN_POINT ( 'NONE',  ( 114.9518748109119883, -7.643976991954077427, -18.09477374809248928 ) ) ;
#23261 = CARTESIAN_POINT ( 'NONE',  ( 121.8725281442453223, -3.383040157471821630, -19.15922257007629170 ) ) ;
#23262 = CARTESIAN_POINT ( 'NONE',  ( 123.4608748109119745, -10.63000616557722466, -14.87417383870573495 ) ) ;
#23263 = ORIENTED_EDGE ( 'NONE', *, *, #42780, .F. ) ;
#23264 = CARTESIAN_POINT ( 'NONE',  ( 114.6115148109119986, -3.383040157471821630, -19.15922257007629170 ) ) ;
#23265 = CARTESIAN_POINT ( 'NONE',  ( 110.0658483795247804, -0.7896495226426338832, -9.318865927141430916 ) ) ;
#23266 = CARTESIAN_POINT ( 'NONE',  ( 107.0099108795247815, -1.325403438956436419, -16.93181055722141792 ) ) ;
#23267 = CARTESIAN_POINT ( 'NONE',  ( 70.19189222814998175, -50.76020450571126474, -33.50691401458669105 ) ) ;
#23268 = CARTESIAN_POINT ( 'NONE',  ( 64.58043734853313822, -37.66840613803912419, -5.037594184586155599 ) ) ;
#23269 = CARTESIAN_POINT ( 'NONE',  ( 119.0361948109119652, -7.893985811506177619, -18.51759400769804742 ) ) ;
#23270 = EDGE_LOOP ( 'NONE', ( #18173, #463, #37489, #27019, #11115 ) ) ;
#23271 = CARTESIAN_POINT ( 'NONE',  ( 125.9001214775786224, -4.089484607189486809, -7.948022111789456723 ) ) ;
#23272 = CARTESIAN_POINT ( 'NONE',  ( 124.8223148109119762, 0.9020085738987273505, -11.91225656197088512 ) ) ;
#23273 = CARTESIAN_POINT ( 'NONE',  ( 113.1933481442453058, -5.574606645277164318, -18.38911715685844683 ) ) ;
#23274 = CARTESIAN_POINT ( 'NONE',  ( 106.1764733795248219, -1.325403438956436419, -9.854619843455211026 ) ) ;
#23275 = CARTESIAN_POINT ( 'NONE',  ( 118.4689281442453392, 0.9020085738987339008, -11.91225656197089222 ) ) ;
#23276 = CARTESIAN_POINT ( 'NONE',  ( 105.9681140045248355, -10.62599879583958717, -11.00651665394454604 ) ) ;
#23277 = CARTESIAN_POINT ( 'NONE',  ( 70.19189222814998175, -57.62004466406306591, -36.25082616574646721 ) ) ;
#23278 = ORIENTED_EDGE ( 'NONE', *, *, #32840, .F. ) ;
#23279 = PLANE ( 'NONE',  #4100 ) ;
#23280 = CARTESIAN_POINT ( 'NONE',  ( 123.2906948109119867, -1.833838273342659697, -17.42832698103878286 ) ) ;
#23281 = CARTESIAN_POINT ( 'NONE',  ( 121.5888948109119809, -10.30919188438810075, -12.61870101168855918 ) ) ;
#23282 = CARTESIAN_POINT ( 'NONE',  ( 114.4980614775786734, -2.084020599724406786, -8.691656652584148546 ) ) ;
#23283 = CARTESIAN_POINT ( 'NONE',  ( 115.6893214775786447, 0.5811942927096154232, -14.16772938898807155 ) ) ;
#23284 = DIRECTION ( 'NONE',  ( 0.9609149988134833009, -0.1028163501681649411, 0.2570431154366530913 ) ) ;
#23285 = CARTESIAN_POINT ( 'NONE',  ( 125.5597614775786326, -7.894159318335828068, -9.358103419637847864 ) ) ;
#23286 = CARTESIAN_POINT ( 'NONE',  ( 119.7169148109119874, -0.1624402480850797581, -16.17319339645315424 ) ) ;
#23287 = ORIENTED_EDGE ( 'NONE', *, *, #18088, .T. ) ;
#23288 = CARTESIAN_POINT ( 'NONE',  ( 119.8303681442452984, -10.63000616557722466, -14.87417383870573495 ) ) ;
#23289 = AXIS2_PLACEMENT_3D ( 'NONE', #3979, #18575, #18355 ) ;
#23290 = CARTESIAN_POINT ( 'NONE',  ( 114.8951481442453115, -0.4660016031367893996, -10.09054647747474043 ) ) ;
#23291 = CARTESIAN_POINT ( 'NONE',  ( 120.2841814775786276, -10.15424416112533912, -14.75197769757731336 ) ) ;
#23292 = ORIENTED_EDGE ( 'NONE', *, *, #2559, .F. ) ;
#23293 = CARTESIAN_POINT ( 'NONE',  ( 123.5633766859119760, -9.033780868592240054, -16.85052413769862056 ) ) ;
#23294 = CARTESIAN_POINT ( 'NONE',  ( 118.1852948109119836, -5.638512984488999180, -18.83840828888717311 ) ) ;
#23295 = CARTESIAN_POINT ( 'NONE',  ( 111.9410827545248708, -2.477300249445798297, -19.15521520033831138 ) ) ;
#23296 = CARTESIAN_POINT ( 'NONE',  ( 117.5045748109119756, -9.859900752359374465, -12.68260735090039404 ) ) ;
#23297 = EDGE_LOOP ( 'NONE', ( #44656, #19905, #16458, #246, #3652 ) ) ;
#23298 = ORIENTED_EDGE ( 'NONE', *, *, #3869, .T. ) ;
#23299 = CIRCLE ( 'NONE', #29222, 8.000000000000000000 ) ;
#23300 = CARTESIAN_POINT ( 'NONE',  ( 125.6164881442453094, -9.565557343593413364, -10.61323700422348004 ) ) ;
#23301 = CARTESIAN_POINT ( 'NONE',  ( 122.2696148109119889, -5.574606645277164318, -18.38911715685844683 ) ) ;
#23302 = APPLICATION_CONTEXT ( 'automotive_design' ) ;
#23303 = LINE ( 'NONE', #37186, #9807 ) ;
#23304 = DIRECTION ( 'NONE',  ( 0.000000000000000000, -0.9242245927363028635, -0.3818493186865930533 ) ) ;
#23305 = CARTESIAN_POINT ( 'NONE',  ( 119.2063748109119814, -1.561330072975668504, -17.79121239304076951 ) ) ;
#23306 = CARTESIAN_POINT ( 'NONE',  ( 108.8156921295247912, 0.8980012041604618078, -13.39321520033831447 ) ) ;
#23307 = CARTESIAN_POINT ( 'NONE',  ( 121.2485348109119769, -0.4660016031367893996, -10.09054647747474043 ) ) ;
#23309 = CARTESIAN_POINT ( 'NONE',  ( 120.4543614775786295, -5.574606645277164318, -18.38911715685844683 ) ) ;
#23308 = CARTESIAN_POINT ( 'NONE',  ( 113.8740681442453138, 0.5811942927096154232, -14.16772938898807155 ) ) ;
#23310 = CARTESIAN_POINT ( 'NONE',  ( 123.4608748109119745, 0.4262465694468514643, -12.03445270309931736 ) ) ;
#23311 = CARTESIAN_POINT ( 'NONE',  ( 114.2144281442453178, -8.166667518702817929, -8.995218007635859436 ) ) ;
#23312 = ORIENTED_EDGE ( 'NONE', *, *, #30730, .F. ) ;
#23313 = CARTESIAN_POINT ( 'NONE',  ( 124.0848681442452772, -5.574606645277164318, -18.38911715685844683 ) ) ;
#23314 = CARTESIAN_POINT ( 'NONE',  ( 122.0217798611595867, -1.036737761566197014, -17.24079555149560861 ) ) ;
#23315 = DIRECTION ( 'NONE',  ( -0.5735764363510446051, 0.3127926500124816878, -0.7570804645221042017 ) ) ;
#23316 = CARTESIAN_POINT ( 'NONE',  ( 114.2330358795247776, -0.7896495226426338832, -17.46756447353520159 ) ) ;
#23317 = CARTESIAN_POINT ( 'NONE',  ( 114.9970202545248412, 0.1403307496149616695, -11.32035403202665336 ) ) ;
#23318 = CARTESIAN_POINT ( 'NONE',  ( 110.6909265045248247, -7.250697342233347165, -19.15521520033831138 ) ) ;
#23319 = AXIS2_PLACEMENT_3D ( 'NONE', #28711, #7948, #21859 ) ;
#23320 = CARTESIAN_POINT ( 'NONE',  ( 121.4754414775786131, -8.166667518702819706, -8.995218007635861213 ) ) ;
#23321 = CARTESIAN_POINT ( 'NONE',  ( 123.1772414775786189, -5.574606645277164318, -18.38911715685844683 ) ) ;
#23322 = ORIENTED_EDGE ( 'NONE', *, *, #4956, .F. ) ;
#23323 = CARTESIAN_POINT ( 'NONE',  ( 120.6812681442452941, -10.30919188438810075, -12.61870101168855918 ) ) ;
#23324 = CARTESIAN_POINT ( 'NONE',  ( 113.3635281442453504, -0.1624402480850797581, -16.17319339645315424 ) ) ;
#23325 = CARTESIAN_POINT ( 'NONE',  ( 70.19189222814998175, -100.0979043305785581, -53.24182196210380624 ) ) ;
#23326 = CARTESIAN_POINT ( 'NONE',  ( 120.5110881442453206, -6.344957434206665248, -7.627207830600338134 ) ) ;
#23327 = CARTESIAN_POINT ( 'NONE',  ( 121.2485348109119769, -0.4660016031367893996, -10.09054647747474043 ) ) ;
#23328 = CARTESIAN_POINT ( 'NONE',  ( 65.37779407113983154, -2.408155782755655672, -18.33092689054683078 ) ) ;
#23329 = CARTESIAN_POINT ( 'NONE',  ( 122.7234281442452755, -4.153390946401325223, -8.397313243818185668 ) ) ;
#23330 = CARTESIAN_POINT ( 'NONE',  ( 70.19189222814998175, -41.58126682492877535, -29.83537093841426469 ) ) ;
#23331 = CARTESIAN_POINT ( 'NONE',  ( 90.72400676789006013, -26.60966817898065884, -11.90521360603286816 ) ) ;
#23332 = EDGE_CURVE ( 'NONE', #37016, #19714, #9965, .T. ) ;
#23333 = EDGE_LOOP ( 'NONE', ( #45033, #5254, #4758, #4422 ) ) ;
#23334 = DIRECTION ( 'NONE',  ( 1.000000000000000000, 0.000000000000000000, -0.000000000000000000 ) ) ;
#23335 = CARTESIAN_POINT ( 'NONE',  ( 94.20708369096698220, -25.89439488952623591, -12.28775498424876211 ) ) ;
#23336 = CARTESIAN_POINT ( 'NONE',  ( 122.3830681442452857, -1.833838273342659697, -17.42832698103878286 ) ) ;
#23337 = CARTESIAN_POINT ( 'NONE',  ( 108.1906140045248037, 0.1403307496149616695, -15.46607636864997204 ) ) ;
#23338 = CARTESIAN_POINT ( 'NONE',  ( 111.1076452545248259, -9.868328341294098749, -15.46607636864997204 ) ) ;
#23339 = AXIS2_PLACEMENT_3D ( 'NONE', #18487, #11425, #1369 ) ;
#23340 = CARTESIAN_POINT ( 'NONE',  ( 117.8449348109119938, -1.833838273342659253, -17.42832698103878286 ) ) ;
#23341 = CARTESIAN_POINT ( 'NONE',  ( 70.00926641990830035, -26.29760602141568526, -5.721420406450495655 ) ) ;
#23342 = CARTESIAN_POINT ( 'NONE',  ( 115.6325948109119821, -9.565557343593413364, -10.61323700422348004 ) ) ;
#23343 = CARTESIAN_POINT ( 'NONE',  ( 122.2128881442453263, -1.834011780172310813, -8.268836392978581529 ) ) ;
#23344 = ORIENTED_EDGE ( 'NONE', *, *, #41477, .T. ) ;
#23345 = EDGE_CURVE ( 'NONE', #17886, #930, #3507, .T. ) ;
#23346 = CARTESIAN_POINT ( 'NONE',  ( 121.8158014775786171, -4.153390946401325223, -8.397313243818185668 ) ) ;
#23347 = CARTESIAN_POINT ( 'NONE',  ( 118.6958348109119754, -6.344957434206665248, -7.627207830600338134 ) ) ;
#23348 = CARTESIAN_POINT ( 'NONE',  ( 124.7088614775786226, 0.2603800115204892296, -16.42320221600525088 ) ) ;
#23349 = CARTESIAN_POINT ( 'NONE',  ( 123.2339681442453241, -3.505236298600246325, -18.68346056562440793 ) ) ;
#23350 = ORIENTED_EDGE ( 'NONE', *, *, #25920, .T. ) ;
#23351 = CARTESIAN_POINT ( 'NONE',  ( 120.5768923109119868, -0.4387604401700512802, -15.73000352943951619 ) ) ;
#23352 = CARTESIAN_POINT ( 'NONE',  ( 125.2761281442453054, -10.63000616557722466, -14.87417383870573495 ) ) ;
#23353 = AXIS2_PLACEMENT_3D ( 'NONE', #4855, #1213, #11707 ) ;
#23354 = CARTESIAN_POINT ( 'NONE',  ( 115.8027748109119841, -8.899110576539710493, -16.42337572283490132 ) ) ;
#23355 = CARTESIAN_POINT ( 'NONE',  ( 126.1270281442452870, -10.30919188438810075, -12.61870101168855918 ) ) ;
#23356 = ADVANCED_FACE ( 'NONE', ( #985 ), #7833, .T. ) ;
#23357 = CARTESIAN_POINT ( 'NONE',  ( 107.0793640045248196, -10.62599879583958717, -11.00651665394454604 ) ) ;
#23358 = EDGE_CURVE ( 'NONE', #36439, #31222, #27958, .T. ) ;
#23359 = EDGE_CURVE ( 'NONE', #2225, #29882, #8056, .T. ) ;
#23360 = FACE_OUTER_BOUND ( 'NONE', #18327, .T. ) ;
#23361 = VERTEX_POINT ( 'NONE', #14673 ) ;
#23362 = CARTESIAN_POINT ( 'NONE',  ( 59.75121349346655109, -13.58877957849837870, -7.404803486908546617 ) ) ;
#23363 = CARTESIAN_POINT ( 'NONE',  ( 108.1906140045248037, 0.1403307496149616695, -15.46607636864997204 ) ) ;
#23364 = AXIS2_PLACEMENT_3D ( 'NONE', #30233, #26816, #44830 ) ;
#23365 = CARTESIAN_POINT ( 'NONE',  ( 70.19189222814998175, -49.76310523276723785, -36.33917278160906505 ) ) ;
#23366 = CIRCLE ( 'NONE', #7343, 4.999999999999998224 ) ;
#23367 = CARTESIAN_POINT ( 'NONE',  ( 121.1350814775786233, -9.859900752359378018, -12.68260735090039759 ) ) ;
#23368 = CARTESIAN_POINT ( 'NONE',  ( 113.1933481442453058, -5.574606645277164318, -18.38911715685844683 ) ) ;
#23369 = CARTESIAN_POINT ( 'NONE',  ( 126.6390922358299207, -0.2797733988919791637, -10.91602890339326137 ) ) ;
#23370 = ORIENTED_EDGE ( 'NONE', *, *, #18308, .F. ) ;
#23371 = CARTESIAN_POINT ( 'NONE',  ( 61.69189222814998175, -49.76310523276723785, -7.393215200338315363 ) ) ;
#23372 = CARTESIAN_POINT ( 'NONE',  ( 120.8514481442452961, -2.084020599724406786, -8.691656652584148546 ) ) ;
#23373 = PRESENTATION_LAYER_ASSIGNMENT (  '', '', ( #5162 ) ) ;
#23374 = CARTESIAN_POINT ( 'NONE',  ( 112.3991748109119868, -1.833838273342658809, -17.42832698103878286 ) ) ;
#23375 = CARTESIAN_POINT ( 'NONE',  ( 67.82132387878262136, -0.4275346869931948013, -10.39321520033832158 ) ) ;
#23376 = CARTESIAN_POINT ( 'NONE',  ( 112.1722681442453222, -8.899110576539710493, -16.42337572283490132 ) ) ;
#23378 = CARTESIAN_POINT ( 'NONE',  ( 122.6667014775786413, -7.893985811506177619, -18.51759400769804742 ) ) ;
#23377 = CYLINDRICAL_SURFACE ( 'NONE', #24378, 1.499999999999999556 ) ;
#23379 = CARTESIAN_POINT ( 'NONE',  ( 126.5808414775786446, -9.859900752359378018, -12.68260735090039759 ) ) ;
#23380 = ORIENTED_EDGE ( 'NONE', *, *, #11652, .F. ) ;
#23381 = DIRECTION ( 'NONE',  ( -0.3445294493088594256, -0.9387755102040817867, 0.000000000000000000 ) ) ;
#23382 = CARTESIAN_POINT ( 'NONE',  ( 109.2294421295247844, -1.388378309844742642, -16.99368411936019641 ) ) ;
#23383 = CARTESIAN_POINT ( 'NONE',  ( 106.1070202545248407, 0.1403307496149616695, -11.32035403202665336 ) ) ;
#23384 = CARTESIAN_POINT ( 'NONE',  ( 124.6521348109119884, -7.894159318335828068, -9.358103419637847864 ) ) ;
#23385 = CARTESIAN_POINT ( 'NONE',  ( 118.9227414775786542, 0.4262465694468514643, -12.03445270309931736 ) ) ;
#23386 = DIRECTION ( 'NONE',  ( 0.000000000000000000, -0.3818493186865927203, 0.9242245927363029745 ) ) ;
#23387 = CARTESIAN_POINT ( 'NONE',  ( 115.5526452545247622, -9.868328341294098749, -15.46607636864997204 ) ) ;
#23388 = EDGE_CURVE ( 'NONE', #37171, #38683, #10194, .T. ) ;
#23389 = CARTESIAN_POINT ( 'NONE',  ( 116.6536748109119941, 0.9020085738987385637, -11.91225656197091887 ) ) ;
#23390 = CARTESIAN_POINT ( 'NONE',  ( 113.7722331777918896, -0.01829820670813664396, -14.64321520033831447 ) ) ;
#23391 = CARTESIAN_POINT ( 'NONE',  ( 112.9664414775786412, -9.859900752359374465, -12.68260735090037983 ) ) ;
#23392 = CARTESIAN_POINT ( 'NONE',  ( 110.1353015045248469, -2.477300249445798297, -7.631215200338321125 ) ) ;
#23393 = CARTESIAN_POINT ( 'NONE',  ( 117.4103264091100840, -0.9924539043446216624, -17.29976612834909133 ) ) ;
#23394 = CARTESIAN_POINT ( 'NONE',  ( 111.8716296295247901, -4.863998795839590272, -19.15521520033831493 ) ) ;
#23395 = CARTESIAN_POINT ( 'NONE',  ( 123.5743281442453139, -7.893985811506177619, -18.51759400769804742 ) ) ;
#23396 = CARTESIAN_POINT ( 'NONE',  ( 122.4397948109119767, -9.988377603198976828, -10.36322818467138340 ) ) ;
#23397 = CARTESIAN_POINT ( 'NONE',  ( 112.0147320646196789, 0.6269505268395592079, -14.64321520033831447 ) ) ;
#23398 = CARTESIAN_POINT ( 'NONE',  ( 118.4689281442453392, 0.9020085738987339008, -11.91225656197089222 ) ) ;
#23399 = B_SPLINE_CURVE_WITH_KNOTS ( 'NONE', 3,
 ( #330, #42069, #10827, #44822, #17228, #20425, #31561, #34743, #27266, #27714 ),
 .UNSPECIFIED., .F., .F.,
 ( 4, 3, 3, 4 ),
 ( 1.939479807224430197E-18, 0.0001671877548681309858, 0.0003343755096277730159, 0.0006463528481650640013 ),
 .UNSPECIFIED. ) ;
#23400 = CARTESIAN_POINT ( 'NONE',  ( 113.7606148109119886, -1.561330072975668060, -17.79121239304076596 ) ) ;
#23401 = ORIENTED_EDGE ( 'NONE', *, *, #33100, .T. ) ;
#23402 = CARTESIAN_POINT ( 'NONE',  ( 113.9875214775786532, -8.899110576539710493, -16.42337572283490132 ) ) ;
#23403 = ADVANCED_FACE ( 'NONE', ( #11931 ), #5070, .T. ) ;
#23404 = CARTESIAN_POINT ( 'NONE',  ( 112.0588148109119828, -9.859900752359374465, -12.68260735090039404 ) ) ;
#23405 = VECTOR ( 'NONE', #39657, 1000.000000000000114 ) ;
#23406 = CARTESIAN_POINT ( 'NONE',  ( 121.8725281442453223, -3.383040157471821630, -19.15922257007629170 ) ) ;
#23407 = CARTESIAN_POINT ( 'NONE',  ( 115.0086014775786509, -4.089484607189486809, -7.948022111789456723 ) ) ;
#23408 = CARTESIAN_POINT ( 'NONE',  ( 113.7038881442453402, -6.222761293078241884, -8.102969835052219238 ) ) ;
#23409 = ORIENTED_EDGE ( 'NONE', *, *, #28101, .T. ) ;
#23410 = VECTOR ( 'NONE', #28287, 999.9999999999998863 ) ;
#23411 = CARTESIAN_POINT ( 'NONE',  ( 119.4900081442453086, -7.643976991954077427, -18.09477374809248928 ) ) ;
#23412 = CARTESIAN_POINT ( 'NONE',  ( 114.3278814775786429, 0.1319031606808879209, -14.10382304977623669 ) ) ;
#23413 = CARTESIAN_POINT ( 'NONE',  ( 109.9269421295247753, 0.8980012041604618078, -13.39321520033831447 ) ) ;
#23414 = CARTESIAN_POINT ( 'NONE',  ( 109.6491296295247793, -4.863998795839590272, -8.388885654883775800 ) ) ;
#23415 = CARTESIAN_POINT ( 'NONE',  ( 122.2696148109119889, -5.574606645277164318, -18.38911715685844683 ) ) ;
#23416 = CARTESIAN_POINT ( 'NONE',  ( 123.7749110609119754, -3.388519251034822766, -18.17055338314092694 ) ) ;
#23417 = DIRECTION ( 'NONE',  ( 0.9609149988134837450, -0.1028163501681639419, 0.2570431154366518145 ) ) ;
#23418 = VERTEX_POINT ( 'NONE', #11487 ) ;
#23419 = EDGE_CURVE ( 'NONE', #38926, #5080, #32011, .T. ) ;
#23420 = DIRECTION ( 'NONE',  ( -1.000000000000000000, 1.091021054073464066E-15, 0.000000000000000000 ) ) ;
#23421 = CARTESIAN_POINT ( 'NONE',  ( 122.5532481442453019, -10.63000616557722466, -14.87417383870573495 ) ) ;
#23422 = DIRECTION ( 'NONE',  ( 0.000000000000000000, -0.3818493186865927203, 0.9242245927363029745 ) ) ;
#23423 = AXIS2_PLACEMENT_3D ( 'NONE', #33145, #36123, #15616 ) ;
#23424 = CARTESIAN_POINT ( 'NONE',  ( 78.69189222814998175, -69.76310523276724496, -16.89321520033831447 ) ) ;
#23425 = CARTESIAN_POINT ( 'NONE',  ( 116.7079629495975155, 2.076812647898142572, -6.016578692477766666 ) ) ;
#23426 = EDGE_CURVE ( 'NONE', #33232, #28936, #18320, .T. ) ;
#23427 = DIRECTION ( 'NONE',  ( -0.9609149988134837450, 0.1028163501681639419, -0.2570431154366518145 ) ) ;
#23428 = CARTESIAN_POINT ( 'NONE',  ( 106.3848327545248651, -6.936859964151250502, -8.388885654883777576 ) ) ;
#23429 = CARTESIAN_POINT ( 'NONE',  ( 123.3840568734310779, -1.223627541775709426, -16.99192386690442547 ) ) ;
#23430 = CARTESIAN_POINT ( 'NONE',  ( 137.4076159488029134, -6.138040881925985737, -18.34368890900572424 ) ) ;
#23431 = AXIS2_PLACEMENT_3D ( 'NONE', #1604, #8914, #25568 ) ;
#23432 = CARTESIAN_POINT ( 'NONE',  ( 125.1162100278347111, -2.486277384090758602, -17.80849669464902973 ) ) ;
#23433 = CARTESIAN_POINT ( 'NONE',  ( 123.7022829359119953, -5.367793381288350041, -18.78638297431641391 ) ) ;
#23434 = CARTESIAN_POINT ( 'NONE',  ( 120.2841814775786276, -10.15424416112533912, -14.75197769757731336 ) ) ;
#23435 = CARTESIAN_POINT ( 'NONE',  ( 119.7434548109119845, -6.180136000736347945, -18.94341591693292415 ) ) ;
#23436 = ORIENTED_EDGE ( 'NONE', *, *, #40911, .T. ) ;
#23437 = CARTESIAN_POINT ( 'NONE',  ( 121.7590748109119687, -7.893985811506177619, -18.51759400769804742 ) ) ;
#23438 = CARTESIAN_POINT ( 'NONE',  ( 120.5678148109119832, -8.166667518702819706, -8.995218007635861213 ) ) ;
#23439 = DIRECTION ( 'NONE',  ( 0.000000000000000000, -0.3818493186865927203, 0.9242245927363029745 ) ) ;
#23440 = CARTESIAN_POINT ( 'NONE',  ( 113.5904348109119866, -2.084020599724406786, -8.691656652584148546 ) ) ;
#23441 = CARTESIAN_POINT ( 'NONE',  ( 112.7962614775786676, -3.383040157471821630, -19.15922257007629170 ) ) ;
#23442 = CARTESIAN_POINT ( 'NONE',  ( 124.3685014775786328, -10.63000616557722466, -14.87417383870573495 ) ) ;
#23443 = CARTESIAN_POINT ( 'NONE',  ( 110.8992858795247827, -0.7896495226426338832, -17.46756447353520159 ) ) ;
#23444 = CARTESIAN_POINT ( 'NONE',  ( 107.4266296295248821, -4.863998795839590272, -8.388885654883775800 ) ) ;
#23445 = CARTESIAN_POINT ( 'NONE',  ( 83.55688843573754809, -32.40901487178031459, -23.84144039813870464 ) ) ;
#23446 = CARTESIAN_POINT ( 'NONE',  ( 115.0653281442453277, -3.505236298600246325, -18.68346056562440793 ) ) ;
#23447 = CARTESIAN_POINT ( 'NONE',  ( 118.0718414775786442, -0.8288870151387760510, -10.36305467784173118 ) ) ;
#23448 = CARTESIAN_POINT ( 'NONE',  ( 87.80477198183443477, -25.99489077589524300, -13.39321520033831625 ) ) ;
#23449 = B_SPLINE_CURVE_WITH_KNOTS ( 'NONE', 3,
 ( #26396, #23435, #5632, #21063, #40999, #23664, #6323, #34127, #33894, #34941, #95, #17428, #30264, #3728, #27923, #19780, #36862, #19552, #33430, #2209, #37319, #30039, #9517, #33662, #43956, #9297, #23205, #2439, #2664, #6090, #16597, #16362, #44190, #12952, #26848, #30490, #40761, #25168, #7374, #42723, #4178, #42054, #752, #28815 ),
 .UNSPECIFIED., .F., .F.,
 ( 4, 2, 2, 2, 2, 2, 2, 2, 2, 2, 2, 2, 2, 2, 2, 2, 2, 2, 2, 2, 2, 4 ),
 ( 0.000000000000000000, 0.03124999999999984041, 0.06249999999999968081, 0.1249999999999993616, 0.1874999999999988898, 0.2187499999999985567, 0.2499999999999982236, 0.2812499999999978906, 0.3124999999999975575, 0.3749999999999973355, 0.4374999999999970579, 0.4687499999999972244, 0.4999999999999973910, 0.5312499999999975575, 0.5624999999999976685, 0.6249999999999980016, 0.6874999999999983347, 0.7499999999999986677, 0.8124999999999991118, 0.8749999999999994449, 0.9374999999999997780, 1.000000000000000000 ),
 .UNSPECIFIED. ) ;
#23450 = CARTESIAN_POINT ( 'NONE',  ( 113.8857702545248003, 0.1403307496149616695, -11.32035403202665336 ) ) ;
#23451 = ORIENTED_EDGE ( 'NONE', *, *, #44066, .T. ) ;
#23452 = CARTESIAN_POINT ( 'NONE',  ( 124.0848681442452772, -5.574606645277146555, -18.38911715685845394 ) ) ;
#23453 = CARTESIAN_POINT ( 'NONE',  ( 124.8223148109119762, -10.15424416112533912, -14.75197769757731336 ) ) ;
#23454 = CARTESIAN_POINT ( 'NONE',  ( 112.0588148109119828, 0.5811942927096154232, -14.16772938898807155 ) ) ;
#23455 = CARTESIAN_POINT ( 'NONE',  ( 123.4939235609119663, 0.6414057260225851653, -11.69287257290600657 ) ) ;
#23456 = CARTESIAN_POINT ( 'NONE',  ( 119.9518141859119851, -8.321307733199551748, -9.223433127585318303 ) ) ;
#23457 = ORIENTED_EDGE ( 'NONE', *, *, #19492, .T. ) ;
#23458 = CARTESIAN_POINT ( 'NONE',  ( 123.5659569693743265, -3.079928505020781415, -14.51995809183469710 ) ) ;
#23459 = LINE ( 'NONE', #37344, #13172 ) ;
#23460 = VERTEX_POINT ( 'NONE', #1210 ) ;
#23461 = CARTESIAN_POINT ( 'NONE',  ( 120.0572748109119772, -3.383040157471821630, -19.15922257007629170 ) ) ;
#23462 = CARTESIAN_POINT ( 'NONE',  ( 126.0135748109119902, -1.833838273342660141, -17.42832698103878286 ) ) ;
#23463 = CARTESIAN_POINT ( 'NONE',  ( 116.9940348109119839, -0.1624402480850797581, -16.17319339645315424 ) ) ;
#23464 =( LENGTH_UNIT ( ) NAMED_UNIT ( * ) SI_UNIT ( .MILLI., .METRE. ) );
#23465 = FACE_OUTER_BOUND ( 'NONE', #39185, .T. ) ;
#23466 = CARTESIAN_POINT ( 'NONE',  ( 120.7379948109119709, -10.63000616557722466, -14.87417383870573495 ) ) ;
#23467 = CARTESIAN_POINT ( 'NONE',  ( 114.2144281442453178, -8.166667518702817929, -8.995218007635859436 ) ) ;
#23468 = EDGE_CURVE ( 'NONE', #41318, #20584, #32436, .T. ) ;
#23469 = CARTESIAN_POINT ( 'NONE',  ( 112.0105358795247810, -8.402594152722688392, -9.854619843455216355 ) ) ;
#23470 = AXIS2_PLACEMENT_3D ( 'NONE', #29932, #40881, #35054 ) ;
#23471 = CARTESIAN_POINT ( 'NONE',  ( 124.5954081442453116, -3.383040157471821630, -19.15922257007629170 ) ) ;
#23472 = CARTESIAN_POINT ( 'NONE',  ( 70.19189222814998175, -60.04498257489500190, -37.22079287717834717 ) ) ;
#23473 = ORIENTED_EDGE ( 'NONE', *, *, #26430, .F. ) ;
#23474 = CARTESIAN_POINT ( 'NONE',  ( 117.7314814775786260, -4.089484607189486809, -7.948022111789456723 ) ) ;
#23475 = CARTESIAN_POINT ( 'NONE',  ( 113.8740681442453138, -9.859900752359374465, -12.68260735090039404 ) ) ;
#23476 = CARTESIAN_POINT ( 'NONE',  ( 126.5010429760490496, -4.957175668312200578, -18.53366791911779288 ) ) ;
#23477 = CARTESIAN_POINT ( 'NONE',  ( 111.9453614775786434, -1.561330072975668060, -17.79121239304076596 ) ) ;
#23478 = VERTEX_POINT ( 'NONE', #29472 ) ;
#23479 = CARTESIAN_POINT ( 'NONE',  ( 121.2485348109119769, -0.4660016031367893996, -10.09054647747474043 ) ) ;
#23480 = LINE ( 'NONE', #9800, #9251 ) ;
#23481 = EDGE_CURVE ( 'NONE', #43660, #10084, #33460, .T. ) ;
#23482 = DIRECTION ( 'NONE',  ( -0.000000000000000000, -0.9284778069183718952, -0.3713878862591649677 ) ) ;
#23483 = CARTESIAN_POINT ( 'NONE',  ( 75.95778847736481509, -3.256761025687722189, -9.893215200338316251 ) ) ;
#23484 = CARTESIAN_POINT ( 'NONE',  ( 116.8805814775786445, -3.505236298600246325, -18.68346056562440793 ) ) ;
#23485 = CARTESIAN_POINT ( 'NONE',  ( 112.7604630939976857, -2.236191541394345172, -18.14152338500401029 ) ) ;
#23486 = VECTOR ( 'NONE', #12806, 1000.000000000000000 ) ;
#23487 = CARTESIAN_POINT ( 'NONE',  ( 116.7671281442453335, -7.643976991954077427, -18.09477374809248928 ) ) ;
#23488 = CARTESIAN_POINT ( 'NONE',  ( 113.1217858795247935, -8.402594152722688392, -9.854619843455216355 ) ) ;
#23489 = VECTOR ( 'NONE', #42219, 1000.000000000000227 ) ;
#23490 = CARTESIAN_POINT ( 'NONE',  ( 82.31000308962319423, -13.76004065658516673, -18.64321520033831803 ) ) ;
#23491 = CARTESIAN_POINT ( 'NONE',  ( 117.1642148109119859, -0.8288870151387760510, -10.36305467784173118 ) ) ;
#23492 = CARTESIAN_POINT ( 'NONE',  ( 116.1431348109119881, -10.30919188438810075, -12.61870101168855918 ) ) ;
#23493 = CARTESIAN_POINT ( 'NONE',  ( 119.8129079359119942, -5.444069387712269226, -19.60292469916370450 ) ) ;
#23494 = CARTESIAN_POINT ( 'NONE',  ( 112.2289948109119848, -1.834011780172310813, -8.268836392978581529 ) ) ;
#23495 = CARTESIAN_POINT ( 'NONE',  ( 116.3133148109120043, -2.084020599724406786, -8.691656652584148546 ) ) ;
#23496 = CARTESIAN_POINT ( 'NONE',  ( 122.3263414775786373, -6.344957434206665248, -7.627207830600338134 ) ) ;
#23497 = CARTESIAN_POINT ( 'NONE',  ( 115.2922348109119781, 0.4262465694468514643, -12.03445270309931736 ) ) ;
#23498 = ORIENTED_EDGE ( 'NONE', *, *, #16469, .T. ) ;
#23499 = CARTESIAN_POINT ( 'NONE',  ( 113.5337081442453240, -9.261995988541697145, -16.69588392320189030 ) ) ;
#23500 = CARTESIAN_POINT ( 'NONE',  ( 111.3854577545248645, -7.250697342233347165, -7.631215200338321125 ) ) ;
#23501 = CARTESIAN_POINT ( 'NONE',  ( 106.0375671295248310, 0.1403307496149613920, -13.39321520033831447 ) ) ;
#23502 = CIRCLE ( 'NONE', #31481, 1.499999999999996225 ) ;
#23503 = FACE_OUTER_BOUND ( 'NONE', #2325, .T. ) ;
#23504 = CARTESIAN_POINT ( 'NONE',  ( 70.19189222814998175, -51.12070001563444066, -33.65111096193285078 ) ) ;
#23505 = CARTESIAN_POINT ( 'NONE',  ( 118.0718414775786300, -9.261995988541697145, -16.69588392320189030 ) ) ;
#23506 = ORIENTED_EDGE ( 'NONE', *, *, #3698, .F. ) ;
#23507 = CARTESIAN_POINT ( 'NONE',  ( 125.4584548109119453, -9.057393577726255529, -18.61460078952223895 ) ) ;
#23508 = CARTESIAN_POINT ( 'NONE',  ( 124.9357681442453014, -1.834011780172303929, -8.268836392978592187 ) ) ;
#23509 = CARTESIAN_POINT ( 'NONE',  ( 115.8595014775786609, -7.643976991954077427, -18.09477374809248928 ) ) ;
#23510 = CARTESIAN_POINT ( 'NONE',  ( 124.1497896737536877, -8.611453504372539314, -17.77011218421760574 ) ) ;
#23511 = CARTESIAN_POINT ( 'NONE',  ( 124.5386814775786206, -5.638512984488999180, -18.83840828888717311 ) ) ;
#23512 = CARTESIAN_POINT ( 'NONE',  ( 115.9693640045247776, 0.1403307496149616695, -15.46607636864997204 ) ) ;
#23513 = CARTESIAN_POINT ( 'NONE',  ( 78.69189222814998175, -69.76310523276724496, -16.89321520033831447 ) ) ;
#23514 = VERTEX_POINT ( 'NONE', #32875 ) ;
#23515 = CARTESIAN_POINT ( 'NONE',  ( 111.7184548109119788, -9.261995988541697145, -16.69588392320189030 ) ) ;
#23516 = CARTESIAN_POINT ( 'NONE',  ( 121.5321681442453183, -0.1624402480850797581, -16.17319339645315424 ) ) ;
#23517 = CARTESIAN_POINT ( 'NONE',  ( 118.6958348109119754, -6.344957434206665248, -7.627207830600338134 ) ) ;
#23518 = CARTESIAN_POINT ( 'NONE',  ( 112.6260814775786514, -0.8288870151387760510, -10.36305467784173118 ) ) ;
#23519 = CARTESIAN_POINT ( 'NONE',  ( 116.0296814775786345, -8.166667518702817929, -8.995218007635861213 ) ) ;
#23520 = CARTESIAN_POINT ( 'NONE',  ( 151.2860562277021472, -4.863998795839242995, -13.39321520033831447 ) ) ;
#23521 =( BOUNDED_SURFACE ( )  B_SPLINE_SURFACE ( 1, 2, ( 
 ( #39292, #35173, #4626, #31991, #15127, #38597, #32215, #35402, #29034, #988, #42944, #31769, #11036, #11261, #8285, #28590, #10812, #541, #24936, #38832, #7601, #18095, #14676, #25834, #40651, #16026, #29934, #26518, #2099, #8962, #12843, #5743, #9187, #5306, #23316, #40427, #39966, #36975, #43848, #19663, #16258, #12389, #2329, #23093, #29702, #8728, #33550, #30160, #5074, #12159, #40195, #43615, #22861, #15573, #9406, #15350, #29258, #36754, #36306, #26287, #39741, #12616, #36533, #5522, #8509, #19442, #33325, #11937, #44079, #26744, #37201, #18773, #32662, #1430, #43168, #43392, #22413, #18991, #32879, #1652, #19222, #29479, #26062, #22634, #33103, #1873, #15800, #30833, #2556, #10320, #30385, #44980, #6888, #13515, #20133, #13955, #41115, #10536, #16485, #41345, #23558, #44525, #34019, #6212, #2788, #13738, #3237, #37440, #24224, #27647, #34678, #13289, #41561, #34243, #13063, #16715, #6449, #30608, #33785, #10102, #24438, #5974, #19899, #27424, #41780, #24006, #27196, #9874, #23784, #38113, #40883, #20798, #20357, #17163, #26962, #37893, #37673, #3463, #6671, #17380, #9637, #3015, #16938, #31269, #44756, #42, #20579, #27867, #34458, #31051, #44308, #11438, #25115, #34889, #21690, #35117, #21909, #14172, #35803, #14853, #10761 ),
 ( #3678, #32388, #11654, #8001, #18498, #3899, #35576, #25343, #7319, #4573, #4349, #7782, #21240, #38329, #1157, #31936, #42892, #7105, #17818, #24884, #24658, #42445, #42220, #39012, #702, #14622, #15073, #41998, #31715, #35347, #10981, #11211, #28985, #17598, #18269, #28762, #31492, #7548, #32164, #21015, #484, #28539, #262, #28089, #42668, #933, #38544, #39237, #28308, #14397, #38778, #21464, #4122, #18041, #5693, #32828, #5250, #43111, #1378, #44023, #1598, #29201, #26233, #26012, #33047, #36482, #12333, #5023, #8231, #36923, #19167, #29878, #1821, #19388, #18939, #4799, #33277, #39916, #30107, #32611, #15293, #25560, #39467, #15975, #15518, #9132, #15749, #40142, #8678, #18720, #22138, #43794, #19612, #12109, #22581, #29650, #43564, #8906, #33496, #22361, #36030, #22805, #11881, #25784, #2051, #12559, #29425, #39692, #8457, #2274, #36256, #43339, #36700, #5468, #26465, #40369, #23036, #16204, #6393, #20301, #34625, #16431, #40830, #9819, #30551, #30779, #41508, #9356, #44704, #3186, #23266, #27139, #10050, #27595, #9585, #2960, #3412, #31218, #34405, #34186, #10264, #16887, #2732, #13465, #23501, #12785, #40598, #6159, #38062, #20078, #37620, #30329, #33733, #26688, #33964, #44255, #27367, #13237, #41289, #23729, #23954 ) ),
 .UNSPECIFIED., .F., .F., .T. ) 
 B_SPLINE_SURFACE_WITH_KNOTS ( ( 2, 2 ),
 ( 3, 2, 2, 2, 2, 2, 2, 2, 2, 2, 2, 2, 2, 2, 2, 2, 2, 2, 2, 2, 2, 2, 2, 2, 2, 2, 2, 2, 2, 2, 2, 2, 2, 2, 2, 2, 2, 2, 2, 2, 2, 2, 2, 2, 2, 2, 2, 2, 2, 2, 2, 2, 2, 2, 2, 2, 2, 2, 2, 2, 2, 2, 2, 2, 2, 2, 2, 2, 2, 2, 2, 2, 2, 2, 2, 2, 2, 2, 2, 2, 3 ),
 ( 0.000000000000000000, 1.000000000000000000 ),
 ( 0.000000000000000000, 0.01250000000000000069, 0.02500000000000000139, 0.03749999999999999861, 0.05000000000000000278, 0.06250000000000000000, 0.07499999999999999722, 0.08749999999999999445, 0.1000000000000000056, 0.1125000000000000028, 0.1250000000000000000, 0.1375000000000000111, 0.1499999999999999944, 0.1625000000000000056, 0.1749999999999999889, 0.1875000000000000000, 0.2000000000000000111, 0.2124999999999999944, 0.2250000000000000056, 0.2374999999999999889, 0.2500000000000000000, 0.2625000000000000111, 0.2750000000000000222, 0.2874999999999999778, 0.2999999999999999889, 0.3125000000000000000, 0.3250000000000000111, 0.3375000000000000222, 0.3499999999999999778, 0.3624999999999999889, 0.3750000000000000000, 0.3875000000000000111, 0.4000000000000000222, 0.4124999999999999778, 0.4249999999999999889, 0.4375000000000000000, 0.4500000000000000111, 0.4625000000000000222, 0.4749999999999999778, 0.4874999999999999889, 0.5000000000000000000, 0.5124999999999999556, 0.5250000000000000222, 0.5374999999999999778, 0.5500000000000000444, 0.5625000000000000000, 0.5749999999999999556, 0.5875000000000000222, 0.5999999999999999778, 0.6125000000000000444, 0.6250000000000000000, 0.6374999999999999556, 0.6500000000000000222, 0.6624999999999999778, 0.6750000000000000444, 0.6875000000000000000, 0.6999999999999999556, 0.7125000000000000222, 0.7249999999999999778, 0.7375000000000000444, 0.7500000000000000000, 0.7624999999999999556, 0.7750000000000000222, 0.7874999999999999778, 0.8000000000000000444, 0.8125000000000000000, 0.8249999999999999556, 0.8375000000000000222, 0.8499999999999999778, 0.8625000000000000444, 0.8750000000000000000, 0.8874999999999999556, 0.9000000000000000222, 0.9124999999999999778, 0.9250000000000000444, 0.9375000000000000000, 0.9499999999999999556, 0.9625000000000000222, 0.9749999999999999778, 0.9875000000000000444, 1.000000000000000000 ),
 .UNSPECIFIED. ) 
 GEOMETRIC_REPRESENTATION_ITEM ( )  RATIONAL_B_SPLINE_SURFACE ( (
 ( 1.000000000000000000, 0.9238795325112869605, 1.000000000000000000, 0.9238795325112869605, 1.000000000000000000, 0.9238795325112869605, 1.000000000000000000, 0.9238795325112869605, 1.000000000000000000, 0.9238795325112869605, 1.000000000000000000, 0.9238795325112869605, 1.000000000000000000, 0.9238795325112869605, 1.000000000000000000, 0.9238795325112869605, 1.000000000000000000, 0.9238795325112869605, 1.000000000000000000, 0.9238795325112869605, 1.000000000000000000, 0.9238795325112869605, 1.000000000000000000, 0.9238795325112869605, 1.000000000000000000, 0.9238795325112869605, 1.000000000000000000, 0.9238795325112869605, 1.000000000000000000, 0.9238795325112869605, 1.000000000000000000, 0.9238795325112869605, 1.000000000000000000, 0.9238795325112869605, 1.000000000000000000, 0.9238795325112869605, 1.000000000000000000, 0.9238795325112869605, 1.000000000000000000, 0.9238795325112869605, 1.000000000000000000, 0.9238795325112869605, 1.000000000000000000, 0.9238795325112869605, 1.000000000000000000, 0.9238795325112869605, 1.000000000000000000, 0.9238795325112869605, 1.000000000000000000, 0.9238795325112869605, 1.000000000000000000, 0.9238795325112869605, 1.000000000000000000, 0.9238795325112869605, 1.000000000000000000, 0.9238795325112869605, 1.000000000000000000, 0.9238795325112869605, 1.000000000000000000, 0.9238795325112869605, 1.000000000000000000, 0.9238795325112869605, 1.000000000000000000, 0.9238795325112869605, 1.000000000000000000, 0.9238795325112869605, 1.000000000000000000, 0.9238795325112869605, 1.000000000000000000, 0.9238795325112869605, 1.000000000000000000, 0.9238795325112869605, 1.000000000000000000, 0.9238795325112869605, 1.000000000000000000, 0.9238795325112869605, 1.000000000000000000, 0.9238795325112869605, 1.000000000000000000, 0.9238795325112869605, 1.000000000000000000, 0.9238795325112869605, 1.000000000000000000, 0.9238795325112869605, 1.000000000000000000, 0.9238795325112869605, 1.000000000000000000, 0.9238795325112869605, 1.000000000000000000, 0.9238795325112869605, 1.000000000000000000, 0.9238795325112869605, 1.000000000000000000, 0.9238795325112869605, 1.000000000000000000, 0.9238795325112869605, 1.000000000000000000, 0.9238795325112869605, 1.000000000000000000, 0.9238795325112869605, 1.000000000000000000, 0.9238795325112869605, 1.000000000000000000, 0.9238795325112869605, 1.000000000000000000, 0.9238795325112869605, 1.000000000000000000, 0.9238795325112869605, 1.000000000000000000, 0.9238795325112869605, 1.000000000000000000, 0.9238795325112869605, 1.000000000000000000, 0.9238795325112869605, 1.000000000000000000, 0.9238795325112869605, 1.000000000000000000, 0.9238795325112869605, 1.000000000000000000, 0.9238795325112869605, 1.000000000000000000, 0.9238795325112869605, 1.000000000000000000, 0.9238795325112869605, 1.000000000000000000, 0.9238795325112869605, 1.000000000000000000, 0.9238795325112869605, 1.000000000000000000, 0.9238795325112869605, 1.000000000000000000, 0.9238795325112869605, 1.000000000000000000, 0.9238795325112869605, 1.000000000000000000, 0.9238795325112869605, 1.000000000000000000, 0.9238795325112869605, 1.000000000000000000, 0.9238795325112869605, 1.000000000000000000, 0.9238795325112869605, 1.000000000000000000, 0.9238795325112869605, 1.000000000000000000, 0.9238795325112869605, 1.000000000000000000, 0.9238795325112869605, 1.000000000000000000, 0.9238795325112869605, 1.000000000000000000, 0.9238795325112869605, 1.000000000000000000, 0.9238795325112869605, 1.000000000000000000, 0.9238795325112869605, 1.000000000000000000, 0.9238795325112869605, 1.000000000000000000, 0.9238795325112869605, 1.000000000000000000),
 ( 1.000000000000000000, 0.9238795325112869605, 1.000000000000000000, 0.9238795325112869605, 1.000000000000000000, 0.9238795325112869605, 1.000000000000000000, 0.9238795325112869605, 1.000000000000000000, 0.9238795325112869605, 1.000000000000000000, 0.9238795325112869605, 1.000000000000000000, 0.9238795325112869605, 1.000000000000000000, 0.9238795325112869605, 1.000000000000000000, 0.9238795325112869605, 1.000000000000000000, 0.9238795325112869605, 1.000000000000000000, 0.9238795325112869605, 1.000000000000000000, 0.9238795325112869605, 1.000000000000000000, 0.9238795325112869605, 1.000000000000000000, 0.9238795325112869605, 1.000000000000000000, 0.9238795325112869605, 1.000000000000000000, 0.9238795325112869605, 1.000000000000000000, 0.9238795325112869605, 1.000000000000000000, 0.9238795325112869605, 1.000000000000000000, 0.9238795325112869605, 1.000000000000000000, 0.9238795325112869605, 1.000000000000000000, 0.9238795325112869605, 1.000000000000000000, 0.9238795325112869605, 1.000000000000000000, 0.9238795325112869605, 1.000000000000000000, 0.9238795325112869605, 1.000000000000000000, 0.9238795325112869605, 1.000000000000000000, 0.9238795325112869605, 1.000000000000000000, 0.9238795325112869605, 1.000000000000000000, 0.9238795325112869605, 1.000000000000000000, 0.9238795325112869605, 1.000000000000000000, 0.9238795325112869605, 1.000000000000000000, 0.9238795325112869605, 1.000000000000000000, 0.9238795325112869605, 1.000000000000000000, 0.9238795325112869605, 1.000000000000000000, 0.9238795325112869605, 1.000000000000000000, 0.9238795325112869605, 1.000000000000000000, 0.9238795325112869605, 1.000000000000000000, 0.9238795325112869605, 1.000000000000000000, 0.9238795325112869605, 1.000000000000000000, 0.9238795325112869605, 1.000000000000000000, 0.9238795325112869605, 1.000000000000000000, 0.9238795325112869605, 1.000000000000000000, 0.9238795325112869605, 1.000000000000000000, 0.9238795325112869605, 1.000000000000000000, 0.9238795325112869605, 1.000000000000000000, 0.9238795325112869605, 1.000000000000000000, 0.9238795325112869605, 1.000000000000000000, 0.9238795325112869605, 1.000000000000000000, 0.9238795325112869605, 1.000000000000000000, 0.9238795325112869605, 1.000000000000000000, 0.9238795325112869605, 1.000000000000000000, 0.9238795325112869605, 1.000000000000000000, 0.9238795325112869605, 1.000000000000000000, 0.9238795325112869605, 1.000000000000000000, 0.9238795325112869605, 1.000000000000000000, 0.9238795325112869605, 1.000000000000000000, 0.9238795325112869605, 1.000000000000000000, 0.9238795325112869605, 1.000000000000000000, 0.9238795325112869605, 1.000000000000000000, 0.9238795325112869605, 1.000000000000000000, 0.9238795325112869605, 1.000000000000000000, 0.9238795325112869605, 1.000000000000000000, 0.9238795325112869605, 1.000000000000000000, 0.9238795325112869605, 1.000000000000000000, 0.9238795325112869605, 1.000000000000000000, 0.9238795325112869605, 1.000000000000000000, 0.9238795325112869605, 1.000000000000000000, 0.9238795325112869605, 1.000000000000000000, 0.9238795325112869605, 1.000000000000000000, 0.9238795325112869605, 1.000000000000000000, 0.9238795325112869605, 1.000000000000000000, 0.9238795325112869605, 1.000000000000000000, 0.9238795325112869605, 1.000000000000000000, 0.9238795325112869605, 1.000000000000000000, 0.9238795325112869605, 1.000000000000000000, 0.9238795325112869605, 1.000000000000000000, 0.9238795325112869605, 1.000000000000000000, 0.9238795325112869605, 1.000000000000000000, 0.9238795325112869605, 1.000000000000000000, 0.9238795325112869605, 1.000000000000000000, 0.9238795325112869605, 1.000000000000000000) ) ) 
 REPRESENTATION_ITEM ( '' )  SURFACE ( )  );
#23522 = CARTESIAN_POINT ( 'NONE',  ( 125.2761281442453054, 0.4262465694468514643, -12.03445270309931736 ) ) ;
#23523 = CARTESIAN_POINT ( 'NONE',  ( 118.0151148109119816, 0.4262465694468514643, -12.03445270309931736 ) ) ;
#23524 = ORIENTED_EDGE ( 'NONE', *, *, #41607, .F. ) ;
#23525 = AXIS2_PLACEMENT_3D ( 'NONE', #5213, #43985, #22768 ) ;
#23526 = CARTESIAN_POINT ( 'NONE',  ( 123.2855641859119942, -0.8832429491016019485, -18.19431474523657855 ) ) ;
#23527 = VECTOR ( 'NONE', #40949, 1000.000000000000114 ) ;
#23528 = B_SPLINE_CURVE_WITH_KNOTS ( 'NONE', 3,
 ( #30822, #41550, #2776, #44745, #34446, #38104, #24212 ),
 .UNSPECIFIED., .F., .F.,
 ( 4, 3, 4 ),
 ( 0.000000000000000000, 0.0003208458851410865066, 0.0006416917706845399550 ),
 .UNSPECIFIED. ) ;
#23529 = CARTESIAN_POINT ( 'NONE',  ( 115.0086014775786509, -4.089484607189486809, -7.948022111789456723 ) ) ;
#23530 = CARTESIAN_POINT ( 'NONE',  ( 122.0994348109119443, -10.15424416112533912, -14.75197769757731336 ) ) ;
#23531 = ORIENTED_EDGE ( 'NONE', *, *, #30147, .F. ) ;
#23532 = CARTESIAN_POINT ( 'NONE',  ( 123.8411891859119862, -1.406689858478933353, -17.56299727309130887 ) ) ;
#23533 = CARTESIAN_POINT ( 'NONE',  ( 137.4478226697587502, -0.5562480781206902147, -10.71977384483395568 ) ) ;
#23534 = CARTESIAN_POINT ( 'NONE',  ( 120.4543614775786295, -4.089484607189486809, -7.948022111789456723 ) ) ;
#23535 = COLOUR_RGB ( '',0.7921568627450980005, 0.8196078431372548767, 0.9333333333333333481 ) ;
#23536 = CARTESIAN_POINT ( 'NONE',  ( 110.7603796295247918, -4.863998795839590272, -19.15521520033831493 ) ) ;
#23537 = CARTESIAN_POINT ( 'NONE',  ( 117.0507614775786465, 0.1319031606808879209, -14.10382304977623669 ) ) ;
#23538 = EDGE_LOOP ( 'NONE', ( #22891, #4813, #6861, #44345, #23380 ) ) ;
#23539 = CIRCLE ( 'NONE', #36619, 8.000000000000001776 ) ;
#23540 = ORIENTED_EDGE ( 'NONE', *, *, #1337, .T. ) ;
#23541 = CARTESIAN_POINT ( 'NONE',  ( 126.5241148109119393, -9.565557343593413364, -10.61323700422348004 ) ) ;
#23542 = EDGE_CURVE ( 'NONE', #13571, #40078, #33097, .T. ) ;
#23543 = B_SPLINE_CURVE_WITH_KNOTS ( 'NONE', 3,
 ( #32118, #25068, #38961, #8188, #35071, #14354, #28494, #4072, #4302, #28941 ),
 .UNSPECIFIED., .F., .F.,
 ( 4, 3, 3, 4 ),
 ( 5.356661003234389743E-18, 0.0002476486541971049601, 0.0004952973025691059577, 0.0009610892161188140746 ),
 .UNSPECIFIED. ) ;
#23544 = CARTESIAN_POINT ( 'NONE',  ( 121.8158014775786171, -4.153390946401325223, -8.397313243818185668 ) ) ;
#23545 = DIRECTION ( 'NONE',  ( 0.000000000000000000, -0.9242245927363028635, -0.3818493186865930533 ) ) ;
#23546 = CARTESIAN_POINT ( 'NONE',  ( 123.2339681442453241, -6.344957434206665248, -7.627207830600338134 ) ) ;
#23547 = CARTESIAN_POINT ( 'NONE',  ( 108.4684265045247997, -7.250697342233347165, -19.15521520033831138 ) ) ;
#23548 = CARTESIAN_POINT ( 'NONE',  ( 118.4689281442453392, 0.9020085738987339008, -11.91225656197089222 ) ) ;
#23550 = CARTESIAN_POINT ( 'NONE',  ( 118.5256548109119876, -8.899110576539710493, -16.42337572283490132 ) ) ;
#23549 = CARTESIAN_POINT ( 'NONE',  ( 118.8092881442453290, -9.988377603198976828, -10.36322818467138340 ) ) ;
#23551 = CARTESIAN_POINT ( 'NONE',  ( 123.2339681442453241, -3.505236298600246325, -18.68346056562440793 ) ) ;
#23552 = DIRECTION ( 'NONE',  ( 0.000000000000000000, 0.000000000000000000, 1.000000000000000000 ) ) ;
#23553 = ORIENTED_EDGE ( 'NONE', *, *, #39833, .T. ) ;
#23554 = CARTESIAN_POINT ( 'NONE',  ( 123.3474214775786209, -0.1624402480850797581, -16.17319339645315424 ) ) ;
#23555 = DIRECTION ( 'NONE',  ( 0.000000000000000000, -0.7996358532186280677, -0.6004852223388321697 ) ) ;
#23556 = TOROIDAL_SURFACE ( 'NONE', #35162, 5.500000000000000000, 0.5000000000000000000 ) ;
#23557 = CARTESIAN_POINT ( 'NONE',  ( 69.36136150295220659, -101.1685209014307674, -50.56525720990386219 ) ) ;
#23558 = CARTESIAN_POINT ( 'NONE',  ( 109.6491296295247793, -4.863998795839590272, -19.15521520033831493 ) ) ;
#23559 = AXIS2_PLACEMENT_3D ( 'NONE', #10979, #18267, #38776 ) ;
#23560 = CARTESIAN_POINT ( 'NONE',  ( 111.8021765045248372, -2.791137627527939813, -8.388885654883777576 ) ) ;
#23561 = CARTESIAN_POINT ( 'NONE',  ( 108.1906140045248463, -10.62599879583958717, -11.00651665394454604 ) ) ;
#23562 = CARTESIAN_POINT ( 'NONE',  ( 123.8012348109119642, 0.2603800115204892296, -16.42320221600525088 ) ) ;
#23563 = CARTESIAN_POINT ( 'NONE',  ( 124.3685014775786328, 0.4262465694468514643, -12.03445270309931736 ) ) ;
#23564 = ORIENTED_EDGE ( 'NONE', *, *, #9005, .F. ) ;
#23565 = CARTESIAN_POINT ( 'NONE',  ( 124.0281414775786146, -1.834011780172310813, -8.268836392978581529 ) ) ;
#23566 = CARTESIAN_POINT ( 'NONE',  ( 112.9097148109120070, -9.565557343593413364, -10.61323700422348004 ) ) ;
#23567 = CARTESIAN_POINT ( 'NONE',  ( 59.41474631770697101, -13.68180984308303216, -19.39321520033831803 ) ) ;
#23568 = CARTESIAN_POINT ( 'NONE',  ( 120.4543614775786295, -4.089484607189486809, -7.948022111789456723 ) ) ;
#23569 = CARTESIAN_POINT ( 'NONE',  ( 122.9503348109119827, 0.5811942927096110934, -14.16772938898807510 ) ) ;
#23570 = CARTESIAN_POINT ( 'NONE',  ( 119.3267360609119692, -3.387241619883791355, -18.17469012370385073 ) ) ;
#23571 = CARTESIAN_POINT ( 'NONE',  ( 122.2128881442453263, -7.643976991954077427, -18.09477374809248928 ) ) ;
#23572 = DIRECTION ( 'NONE',  ( -0.9659258262890689783, -0.2588190451025185190, 0.000000000000000000 ) ) ;
#23573 = CARTESIAN_POINT ( 'NONE',  ( 123.0772048109119652, -2.527210466738041728, -8.967976844669124148 ) ) ;
#23574 = VERTEX_POINT ( 'NONE', #26058 ) ;
#23575 = CIRCLE ( 'NONE', #1695, 2.000000000000000444 ) ;
#23576 = CARTESIAN_POINT ( 'NONE',  ( 92.04708369096698561, -26.60966817898065884, -11.90521360603286816 ) ) ;
#23577 = CARTESIAN_POINT ( 'NONE',  ( 123.3474214775786209, -0.1624402480850797581, -16.17319339645315424 ) ) ;
#23578 = CARTESIAN_POINT ( 'NONE',  ( 109.8574890045247940, -9.868328341294098749, -11.32035403202665869 ) ) ;
#23579 = CARTESIAN_POINT ( 'NONE',  ( 112.2188952545247531, -9.868328341294098749, -15.46607636864997204 ) ) ;
#23580 = CARTESIAN_POINT ( 'NONE',  ( 117.3343948109119737, -6.222761293078241884, -8.102969835052219238 ) ) ;
#23581 = CARTESIAN_POINT ( 'NONE',  ( 117.6747548109119919, -7.643976991954077427, -18.09477374809248928 ) ) ;
#23582 = CARTESIAN_POINT ( 'NONE',  ( 123.2339681442453241, -6.344957434206665248, -7.627207830600338134 ) ) ;
#23583 = EDGE_LOOP ( 'NONE', ( #43201, #8026, #19956, #1854, #44094 ) ) ;
#23584 = CARTESIAN_POINT ( 'NONE',  ( 122.0427081442452817, -9.859900752359378018, -12.68260735090039759 ) ) ;
#23585 = CARTESIAN_POINT ( 'NONE',  ( 118.6391081442452986, -4.089484607189486809, -7.948022111789456723 ) ) ;
#23586 = CARTESIAN_POINT ( 'NONE',  ( 125.3895814775786448, -7.893985811506177619, -18.51759400769804742 ) ) ;
#23587 = CARTESIAN_POINT ( 'NONE',  ( 122.3830681442452857, -1.833838273342659697, -17.42832698103878286 ) ) ;
#23588 = ORIENTED_EDGE ( 'NONE', *, *, #35361, .T. ) ;
#23589 = CARTESIAN_POINT ( 'NONE',  ( 121.0630641859119976, -8.321307733199551748, -9.223433127585318303 ) ) ;
#23590 = CIRCLE ( 'NONE', #35094, 2.000000000000000444 ) ;
#23591 = CARTESIAN_POINT ( 'NONE',  ( 125.7866681442452688, -0.4660016031367893996, -10.09054647747474043 ) ) ;
#23592 = CARTESIAN_POINT ( 'NONE',  ( 116.3133148109120043, -2.084020599724406786, -8.691656652584148546 ) ) ;
#23593 = CARTESIAN_POINT ( 'NONE',  ( 124.3685014775786328, -10.63000616557722466, -14.87417383870573495 ) ) ;
#23594 = CARTESIAN_POINT ( 'NONE',  ( 117.6067460002551002, -2.334846009198389805, -18.01015021110788439 ) ) ;
#23595 = CARTESIAN_POINT ( 'NONE',  ( 123.9800954359119771, 0.5291689781388270175, -13.89700978578772705 ) ) ;
#23596 = EDGE_LOOP ( 'NONE', ( #11258, #24413, #36960, #30660, #35329 ) ) ;
#23597 = CYLINDRICAL_SURFACE ( 'NONE', #35359, 1.499999999999998002 ) ;
#23598 = CARTESIAN_POINT ( 'NONE',  ( 110.5520202545248054, 0.1403307496149616695, -11.32035403202665336 ) ) ;
#23599 = AXIS2_PLACEMENT_3D ( 'NONE', #25441, #39343, #35906 ) ;
#23600 = CARTESIAN_POINT ( 'NONE',  ( 122.6009548109119720, 2.250047331442289966, -9.733932798157443500 ) ) ;
#23601 = CARTESIAN_POINT ( 'NONE',  ( 118.1285681442453068, -2.084020599724406786, -8.691656652584148546 ) ) ;
#23602 = CARTESIAN_POINT ( 'NONE',  ( 113.3635281442453504, -0.1624402480850797581, -16.17319339645315424 ) ) ;
#23603 = CARTESIAN_POINT ( 'NONE',  ( 126.4262034846834126, -0.4795738038250874635, -10.78031458779252638 ) ) ;
#23604 = ORIENTED_EDGE ( 'NONE', *, *, #37614, .F. ) ;
#23605 = CARTESIAN_POINT ( 'NONE',  ( 138.2184548109119930, -7.252096815532139473, -18.89748516540533529 ) ) ;
#23606 = CARTESIAN_POINT ( 'NONE',  ( 120.0572748109119772, -6.222761293078241884, -8.102969835052219238 ) ) ;
#23607 = CARTESIAN_POINT ( 'NONE',  ( 112.5126281442453120, 0.1319031606808879209, -14.10382304977623669 ) ) ;
#23608 = CARTESIAN_POINT ( 'NONE',  ( 111.6852908578216983, 0.04929351793716424401, -12.14321520033834467 ) ) ;
#23609 = DIRECTION ( 'NONE',  ( -1.000000000000000000, 0.000000000000000000, 0.000000000000000000 ) ) ;
#23611 = CARTESIAN_POINT ( 'NONE',  ( 87.02785693856107230, -25.99489077589524300, -13.39321520033831447 ) ) ;
#23610 = CARTESIAN_POINT ( 'NONE',  ( 96.46827370896536991, -26.60028948451273223, -14.20056342530837412 ) ) ;
#23612 = CARTESIAN_POINT ( 'NONE',  ( 125.2194014775786286, 0.1319031606808879209, -14.10382304977623669 ) ) ;
#23613 = ORIENTED_EDGE ( 'NONE', *, *, #8588, .F. ) ;
#23614 = CARTESIAN_POINT ( 'NONE',  ( 111.8319081442453182, -5.638512984488999180, -18.83840828888717311 ) ) ;
#23615 = LINE ( 'NONE', #33612, #18751 ) ;
#23616 = CARTESIAN_POINT ( 'NONE',  ( 107.7044421295247929, -9.868328341294093420, -13.39321520033831447 ) ) ;
#23617 = CARTESIAN_POINT ( 'NONE',  ( 112.1155414775786454, 0.9020085738987339008, -11.91225656197089222 ) ) ;
#23618 = CARTESIAN_POINT ( 'NONE',  ( 121.5321681442453183, -0.1624402480850797581, -16.17319339645315424 ) ) ;
#23619 = CARTESIAN_POINT ( 'NONE',  ( 123.9584548109119737, -4.863998795839242995, -13.39321520033831447 ) ) ;
#23620 = CARTESIAN_POINT ( 'NONE',  ( 115.6915515045247531, -6.936859964151250502, -18.39754474579286025 ) ) ;
#23621 = CARTESIAN_POINT ( 'NONE',  ( 109.2296334740164809, -2.305094363982043593, -17.76548269841391203 ) ) ;
#23622 = CARTESIAN_POINT ( 'NONE',  ( 113.8740681442453138, -9.859900752359374465, -12.68260735090039404 ) ) ;
#23623 = CARTESIAN_POINT ( 'NONE',  ( 108.8156921295247912, 0.8980012041604618078, -13.39321520033831447 ) ) ;
#23624 = B_SPLINE_CURVE_WITH_KNOTS ( 'NONE', 3,
 ( #1488, #26349, #40257, #15410, #33384, #29990, #43456, #40488, #29540, #2156 ),
 .UNSPECIFIED., .F., .F.,
 ( 4, 2, 2, 2, 4 ),
 ( 3.469446951953614189E-18, 0.0003217971434675209806, 0.0006435942869350384917, 0.0009653914304025559487, 0.001287188573870073514 ),
 .UNSPECIFIED. ) ;
#23625 = CARTESIAN_POINT ( 'NONE',  ( 119.7434548109119703, -11.97804492312076086, -17.05249760251924229 ) ) ;
#23626 = CARTESIAN_POINT ( 'NONE',  ( 113.5385046295247804, -4.863998795839590272, -7.631215200338315796 ) ) ;
#23627 = CARTESIAN_POINT ( 'NONE',  ( 124.9924948109119924, -4.089484607189486809, -7.948022111789456723 ) ) ;
#23628 = CARTESIAN_POINT ( 'NONE',  ( 121.7023481442452777, -9.261995988541697145, -16.69588392320189030 ) ) ;
#23629 = DIRECTION ( 'NONE',  ( 0.000000000000000000, -0.6004852223388321697, 0.7996358532186280677 ) ) ;
#23630 = CARTESIAN_POINT ( 'NONE',  ( 122.0994348109119443, 0.9020085738987339008, -11.91225656197089222 ) ) ;
#23631 = ADVANCED_FACE ( 'NONE', ( #25614 ), #9469, .T. ) ;
#23632 = CARTESIAN_POINT ( 'NONE',  ( 114.3278814775786429, -10.30919188438810075, -12.61870101168855918 ) ) ;
#23633 = VERTEX_POINT ( 'NONE', #11257 ) ;
#23634 = CARTESIAN_POINT ( 'NONE',  ( 113.7038881442453402, -6.222761293078241884, -8.102969835052219238 ) ) ;
#23635 = CARTESIAN_POINT ( 'NONE',  ( 126.1837548109119211, -10.63000616557722466, -14.87417383870573495 ) ) ;
#23636 = CARTESIAN_POINT ( 'NONE',  ( 123.3474214775786209, -9.988377603198976828, -10.36322818467138340 ) ) ;
#23637 = CARTESIAN_POINT ( 'NONE',  ( 113.3068014775786594, -8.166667518702817929, -8.995218007635859436 ) ) ;
#23638 = CARTESIAN_POINT ( 'NONE',  ( 114.3278814775786429, 0.1319031606808879209, -14.10382304977623669 ) ) ;
#23639 = ORIENTED_EDGE ( 'NONE', *, *, #37070, .F. ) ;
#23640 = CARTESIAN_POINT ( 'NONE',  ( 118.1852948109119836, -4.153390946401325223, -8.397313243818185668 ) ) ;
#23641 = CARTESIAN_POINT ( 'NONE',  ( 112.5126281442453120, -10.30919188438810075, -12.61870101168855918 ) ) ;
#23642 = MECHANICAL_DESIGN_GEOMETRIC_PRESENTATION_REPRESENTATION (  '', ( #13452 ), #29447 ) ;
#23643 = CARTESIAN_POINT ( 'NONE',  ( 109.3713171295247832, 0.1403307496149613920, -13.39321520033831447 ) ) ;
#23644 = CARTESIAN_POINT ( 'NONE',  ( 122.0427081442452817, -9.859900752359378018, -12.68260735090039759 ) ) ;
#23645 = CARTESIAN_POINT ( 'NONE',  ( 116.8582369479724719, -0.4338739127440741083, -16.23602533977254581 ) ) ;
#23646 = CARTESIAN_POINT ( 'NONE',  ( 111.7327233795247849, -8.938348069036489818, -17.46756447353520159 ) ) ;
#23647 = EDGE_LOOP ( 'NONE', ( #3295, #25848, #36886, #21318, #38310 ) ) ;
#23648 = AXIS2_PLACEMENT_3D ( 'NONE', #17750, #20733, #34613 ) ;
#23649 = DIRECTION ( 'NONE',  ( 1.000000000000000000, 0.000000000000000000, 0.000000000000000000 ) ) ;
#23650 = CARTESIAN_POINT ( 'NONE',  ( 112.8421051332721845, 0.2334052082820642360, -14.64321520033830026 ) ) ;
#23651 = EDGE_CURVE ( 'NONE', #31450, #10427, #8281, .T. ) ;
#23652 = CARTESIAN_POINT ( 'NONE',  ( 59.24641515291911986, -13.72835195454734247, -19.39321520033831447 ) ) ;
#23653 = CARTESIAN_POINT ( 'NONE',  ( 122.5215798109119874, -2.173413727453597843, -8.297982527556802879 ) ) ;
#23654 = DIRECTION ( 'NONE',  ( 0.000000000000000000, 0.000000000000000000, 1.000000000000000000 ) ) ;
#23655 = ADVANCED_FACE ( 'NONE', ( #39063 ), #36079, .F. ) ;
#23656 = CARTESIAN_POINT ( 'NONE',  ( 108.6767858795247861, -8.402594152722688392, -9.854619843455216355 ) ) ;
#23657 = CARTESIAN_POINT ( 'NONE',  ( 123.2331352477523723, -1.220279397241712971, -16.99638242193887194 ) ) ;
#23658 = CARTESIAN_POINT ( 'NONE',  ( 116.7671281442453335, -1.834011780172310813, -8.268836392978581529 ) ) ;
#23659 = LINE ( 'NONE', #38000, #25296 ) ;
#23660 = ADVANCED_FACE ( 'NONE', ( #39962, #28811 ), #25392, .T. ) ;
#23661 = CARTESIAN_POINT ( 'NONE',  ( 125.1048602609374001, -2.479354771058042584, -17.81771518891497763 ) ) ;
#23662 = CARTESIAN_POINT ( 'NONE',  ( 124.1221766859119811, -0.6978242514987066381, -9.938897388174217085 ) ) ;
#23663 = CARTESIAN_POINT ( 'NONE',  ( 122.4965214775786251, 0.1319031606808879209, -14.10382304977623669 ) ) ;
#23664 = CARTESIAN_POINT ( 'NONE',  ( 119.7434548109119561, -5.045040375314679082, -19.05184332167395667 ) ) ;
#23665 = ORIENTED_EDGE ( 'NONE', *, *, #14501, .T. ) ;
#23666 = CARTESIAN_POINT ( 'NONE',  ( 135.4522060580443394, -9.608978949641880263, -9.721040106140581116 ) ) ;
#23667 = CARTESIAN_POINT ( 'NONE',  ( 119.6034614775786196, -6.344957434206665248, -7.627207830600338134 ) ) ;
#23668 = CARTESIAN_POINT ( 'NONE',  ( 68.07789357685331311, -68.58957386525776201, -38.44539312525988350 ) ) ;
#23669 = CARTESIAN_POINT ( 'NONE',  ( 115.6325948109119821, -9.565557343593413364, -10.61323700422348004 ) ) ;
#23670 = EDGE_CURVE ( 'NONE', #15605, #31742, #15124, .T. ) ;
#23671 = CARTESIAN_POINT ( 'NONE',  ( 123.9146881442452894, 0.9020085738987339008, -11.91225656197089222 ) ) ;
#23672 = CARTESIAN_POINT ( 'NONE',  ( 109.9963952545248134, 0.8980012041604421569, -11.00651665394454071 ) ) ;
#23673 = CARTESIAN_POINT ( 'NONE',  ( 106.3153796295248412, -4.863998795839590272, -8.388885654883775800 ) ) ;
#23674 = CARTESIAN_POINT ( 'NONE',  ( 83.25049447561245586, -31.94586068832097681, -23.46952294068349332 ) ) ;
#23675 = VECTOR ( 'NONE', #41045, 1000.000000000000000 ) ;
#23676 = CARTESIAN_POINT ( 'NONE',  ( 115.1220548109119761, -1.833838273342658809, -17.42832698103878286 ) ) ;
#23677 = CARTESIAN_POINT ( 'NONE',  ( 116.3700414775786527, -4.153390946401321671, -8.397313243818183892 ) ) ;
#23678 = FACE_OUTER_BOUND ( 'NONE', #20827, .T. ) ;
#23679 = CARTESIAN_POINT ( 'NONE',  ( 114.1635827545248389, -6.936859964151250502, -8.388885654883777576 ) ) ;
#23680 = ORIENTED_EDGE ( 'NONE', *, *, #13189, .F. ) ;
#23681 = EDGE_CURVE ( 'NONE', #41698, #1633, #26259, .T. ) ;
#23682 = LINE ( 'NONE', #20256, #25512 ) ;
#23683 = CARTESIAN_POINT ( 'NONE',  ( 113.1933481442453058, -4.089484607189486809, -7.948022111789456723 ) ) ;
#23684 = CARTESIAN_POINT ( 'NONE',  ( 79.39504145264901069, 5.044464786489276875, -6.294580001266408154 ) ) ;
#23685 = CARTESIAN_POINT ( 'NONE',  ( 123.2161110609119703, -6.340755971794695078, -8.611740276972781771 ) ) ;
#23686 = CARTESIAN_POINT ( 'NONE',  ( 119.2572829359120021, -5.367793381288652910, -18.78638297431638904 ) ) ;
#23687 = EDGE_CURVE ( 'NONE', #21740, #25821, #23087, .T. ) ;
#23688 = EDGE_CURVE ( 'NONE', #2128, #39376, #30380, .T. ) ;
#23689 = ORIENTED_EDGE ( 'NONE', *, *, #3274, .T. ) ;
#23690 = CARTESIAN_POINT ( 'NONE',  ( 113.8163171295247764, -10.62599879583958540, -13.39321520033831803 ) ) ;
#23691 = CIRCLE ( 'NONE', #3988, 2.999999999999999556 ) ;
#23692 = CARTESIAN_POINT ( 'NONE',  ( 111.4739159103406223, -1.291319350021640888, -16.90178210349550625 ) ) ;
#23693 = ORIENTED_EDGE ( 'NONE', *, *, #31684, .T. ) ;
#23694 = CARTESIAN_POINT ( 'NONE',  ( 117.1074881442453233, -10.63000616557722466, -14.87417383870573495 ) ) ;
#23695 = CARTESIAN_POINT ( 'NONE',  ( 112.0020881442453344, 0.2603800115204892296, -16.42320221600525088 ) ) ;
#23696 = CARTESIAN_POINT ( 'NONE',  ( 117.1642148109119859, -0.8288870151387760510, -10.36305467784173118 ) ) ;
#23697 = CARTESIAN_POINT ( 'NONE',  ( 122.6009548109119720, 3.074545301078819737, -12.40350937470759973 ) ) ;
#23698 = CARTESIAN_POINT ( 'NONE',  ( 121.5888948109119809, -10.30919188438810075, -12.61870101168855918 ) ) ;
#23699 = CARTESIAN_POINT ( 'NONE',  ( 119.6601881442453106, -8.166667518702819706, -8.995218007635861213 ) ) ;
#23700 = CARTESIAN_POINT ( 'NONE',  ( 109.3713171295247832, 0.1403307496149613920, -13.39321520033831447 ) ) ;
#23701 = CARTESIAN_POINT ( 'NONE',  ( 114.4413348109119823, -0.8288870151387760510, -10.36305467784173118 ) ) ;
#23702 = CARTESIAN_POINT ( 'NONE',  ( 83.82415148905927538, -46.76310523276723785, -23.89321520033831803 ) ) ;
#23703 = ORIENTED_EDGE ( 'NONE', *, *, #34491, .F. ) ;
#23704 = CARTESIAN_POINT ( 'NONE',  ( 118.9227414775786400, -10.63000616557722466, -14.87417383870573495 ) ) ;
#23705 = CARTESIAN_POINT ( 'NONE',  ( 120.5074391859119913, -8.844754642576884152, -8.592115655440050404 ) ) ;
#23706 = CARTESIAN_POINT ( 'NONE',  ( 116.2565881442452991, -9.261995988541697145, -16.69588392320189030 ) ) ;
#23707 = AXIS2_PLACEMENT_3D ( 'NONE', #1753, #4952, #15677 ) ;
#23708 = ORIENTED_EDGE ( 'NONE', *, *, #6757, .F. ) ;
#23709 = CARTESIAN_POINT ( 'NONE',  ( 122.3263414775786373, -6.344957434206665248, -7.627207830600338134 ) ) ;
#23710 = DIRECTION ( 'NONE',  ( 0.000000000000000000, 0.6004852223388318366, -0.7996358532186281787 ) ) ;
#23711 = CARTESIAN_POINT ( 'NONE',  ( 112.8529881442453302, -7.894159318335828068, -9.358103419637847864 ) ) ;
#23712 = DIRECTION ( 'NONE',  ( 0.000000000000000000, 0.4669533266896290225, 0.8842819633428516957 ) ) ;
#23713 = CARTESIAN_POINT ( 'NONE',  ( 114.6115148109119986, -6.222761293078241884, -8.102969835052219238 ) ) ;
#23714 = CARTESIAN_POINT ( 'NONE',  ( 74.19189222814998175, -41.76310523276723785, -4.893215200338314474 ) ) ;
#23715 = AXIS2_PLACEMENT_3D ( 'NONE', #16537, #37948, #20184 ) ;
#23716 = CARTESIAN_POINT ( 'NONE',  ( 118.9794681442453026, -0.8288870151387760510, -10.36305467784173118 ) ) ;
#23717 = CARTESIAN_POINT ( 'NONE',  ( 151.2860562277021472, -3.719473736431747390, -16.16631137400202078 ) ) ;
#23718 = CARTESIAN_POINT ( 'NONE',  ( 114.6115148109119986, -6.222761293078241884, -8.102969835052219238 ) ) ;
#23719 = CARTESIAN_POINT ( 'NONE',  ( 114.0442481442453300, -1.834011780172310813, -8.268836392978581529 ) ) ;
#23720 = CARTESIAN_POINT ( 'NONE',  ( 123.4244704359119709, -10.25716656981731489, -12.88942061488890545 ) ) ;
#23721 = CARTESIAN_POINT ( 'NONE',  ( 126.3539348109119800, -4.153390946401325223, -8.397313243818185668 ) ) ;
#23722 = CARTESIAN_POINT ( 'NONE',  ( 116.5402214775786405, -9.565557343593413364, -10.61323700422348004 ) ) ;
#23723 = CARTESIAN_POINT ( 'NONE',  ( 113.0231681442453180, -10.15424416112533912, -14.75197769757731336 ) ) ;
#23724 = CARTESIAN_POINT ( 'NONE',  ( 117.3343948109119737, -6.222761293078241884, -8.102969835052219238 ) ) ;
#23725 = ORIENTED_EDGE ( 'NONE', *, *, #40662, .T. ) ;
#23726 = CARTESIAN_POINT ( 'NONE',  ( 111.7184548109119788, -9.261995988541697145, -16.69588392320189030 ) ) ;
#23727 = EDGE_CURVE ( 'NONE', #29197, #8760, #37114, .T. ) ;
#23728 = CARTESIAN_POINT ( 'NONE',  ( 109.4407702545248355, -10.62599879583958717, -15.77991374673208469 ) ) ;
#23729 = CARTESIAN_POINT ( 'NONE',  ( 104.9957702545248566, 0.1403307496149616695, -11.32035403202665336 ) ) ;
#23730 = LINE ( 'NONE', #30781, #15905 ) ;
#23731 = CARTESIAN_POINT ( 'NONE',  ( 109.8889130180080826, 0.7607806665037644134, -14.64321520033833757 ) ) ;
#23732 = CARTESIAN_POINT ( 'NONE',  ( 117.6747548109119919, -1.834011780172310813, -8.268836392978581529 ) ) ;
#23733 = ORIENTED_EDGE ( 'NONE', *, *, #24219, .F. ) ;
#23734 = CARTESIAN_POINT ( 'NONE',  ( 125.8433948109119456, -1.834011780172310813, -8.268836392978581529 ) ) ;
#23735 = PLANE ( 'NONE',  #27791 ) ;
#23736 = B_SPLINE_CURVE_WITH_KNOTS ( 'NONE', 3,
 ( #18333, #35413, #4189, #14686, #14914, #15364, #29268, #43183, #44319, #44089, #2109, #1884, #26755, #5754, #40437, #15811, #9416, #33335, #12854, #5535, #30172, #12399, #29945, #37214, #12630, #16037, #23107, #23328, #36316, #43858, #5086, #26528 ),
 .UNSPECIFIED., .F., .F.,
 ( 4, 2, 2, 2, 1, 1, 1, 1, 2, 2, 2, 2, 1, 1, 1, 1, 2, 2, 2, 4 ),
 ( 0.000000000000000000, 0.1249999999996142253, 0.1874999999994223787, 0.2187499999993277600, 0.2343749999992789101, 0.2421874999992546795, 0.2460937499992454647, 0.2480468749992408850, 0.2490234374992384980, 0.2499999999992360555, 0.3749999999992827404, 0.4374999999993081645, 0.4687499999993228195, 0.4843749999993324229, 0.4921874999993394173, 0.4960937499993454125, 0.4980468749993482436, 0.4999999999993510746, 0.7499999999996754818, 1.000000000000000000 ),
 .UNSPECIFIED. ) ;
#23737 = CARTESIAN_POINT ( 'NONE',  ( 119.5467348109119712, -5.574606645277164318, -18.38911715685844683 ) ) ;
#23738 = DIRECTION ( 'NONE',  ( -1.000000000000000000, 0.000000000000000000, -0.000000000000000000 ) ) ;
#23739 = CARTESIAN_POINT ( 'NONE',  ( 124.9357681442453014, -1.834011780172310813, -8.268836392978581529 ) ) ;
#23740 = CARTESIAN_POINT ( 'NONE',  ( 115.6915515045247531, -6.936859964151250502, -18.39754474579286025 ) ) ;
#23741 = CARTESIAN_POINT ( 'NONE',  ( 127.7184548109119788, -4.863998795839242995, -13.39321520033831447 ) ) ;
#23742 = ORIENTED_EDGE ( 'NONE', *, *, #6657, .F. ) ;
#23743 = PLANE ( 'NONE',  #10697 ) ;
#23744 = CARTESIAN_POINT ( 'NONE',  ( 124.3685014775786328, 0.4262465694468514643, -12.03445270309931736 ) ) ;
#23745 = CARTESIAN_POINT ( 'NONE',  ( 120.1707281442453166, 0.2603800115204892296, -16.42320221600525088 ) ) ;
#23746 = CARTESIAN_POINT ( 'NONE',  ( 113.5904348109119866, -2.084020599724406786, -8.691656652584148546 ) ) ;
#23747 = CARTESIAN_POINT ( 'NONE',  ( 117.7314814775786260, -4.089484607189486809, -7.948022111789456723 ) ) ;
#23748 = CARTESIAN_POINT ( 'NONE',  ( 61.63318325272354770, -19.46990085680238636, -10.89321520033831447 ) ) ;
#23749 = ADVANCED_FACE ( 'NONE', ( #33780 ), #8993, .T. ) ;
#23750 = CARTESIAN_POINT ( 'NONE',  ( 127.0553483106876058, -1.260408809135023178, -9.346765518329249289 ) ) ;
#23751 = CARTESIAN_POINT ( 'NONE',  ( 123.5743281442453139, -2.084020599724406786, -8.691656652584148546 ) ) ;
#23752 = VERTEX_POINT ( 'NONE', #1083 ) ;
#23753 = AXIS2_PLACEMENT_3D ( 'NONE', #34717, #27008, #82 ) ;
#23754 = CARTESIAN_POINT ( 'NONE',  ( 85.70315449690899356, -26.74675748045603996, -18.39321520033831803 ) ) ;
#23755 = CARTESIAN_POINT ( 'NONE',  ( 118.1852948109119836, -5.638512984488999180, -18.83840828888717311 ) ) ;
#23756 = CARTESIAN_POINT ( 'NONE',  ( 120.1140014775786398, -7.894159318335828068, -9.358103419637847864 ) ) ;
#23757 = VERTEX_POINT ( 'NONE', #43037 ) ;
#23758 = CARTESIAN_POINT ( 'NONE',  ( 122.3132204359119868, -10.25716656981731489, -12.88942061488890545 ) ) ;
#23759 = CARTESIAN_POINT ( 'NONE',  ( 62.93574133341893173, -12.59213563260223800, -10.20028763956079132 ) ) ;
#23760 = CARTESIAN_POINT ( 'NONE',  ( 119.4900081442453086, -1.834011780172310813, -8.268836392978581529 ) ) ;
#23761 = CARTESIAN_POINT ( 'NONE',  ( 112.3578015045248861, -2.477300249445798297, -7.631215200338321125 ) ) ;
#23762 = CARTESIAN_POINT ( 'NONE',  ( 115.8027748109119841, -8.899110576539710493, -16.42337572283490132 ) ) ;
#23763 = ORIENTED_EDGE ( 'NONE', *, *, #24486, .F. ) ;
#23764 = ORIENTED_EDGE ( 'NONE', *, *, #9323, .F. ) ;
#23765 = CARTESIAN_POINT ( 'NONE',  ( 125.5030348109119558, -6.222761293078241884, -8.102969835052219238 ) ) ;
#23766 = VECTOR ( 'NONE', #35870, 999.9999999999998863 ) ;
#23767 = CARTESIAN_POINT ( 'NONE',  ( 124.0848681442452772, -5.574606645277164318, -18.38911715685844683 ) ) ;
#23768 = CARTESIAN_POINT ( 'NONE',  ( 87.14323352029596492, -24.14644159042263993, -12.62951656296512937 ) ) ;
#23769 = DIRECTION ( 'NONE',  ( 1.000000000000000000, 0.000000000000000000, -0.000000000000000000 ) ) ;
#23770 = CARTESIAN_POINT ( 'NONE',  ( 120.8514481442452961, -7.893985811506177619, -18.51759400769804742 ) ) ;
#23771 = CARTESIAN_POINT ( 'NONE',  ( 85.38561350750011059, -9.917550408422661334, -13.24321520033830879 ) ) ;
#23772 = CARTESIAN_POINT ( 'NONE',  ( 117.0734209221557336, -2.372251574601226043, -17.96033910819752322 ) ) ;
#23773 = CARTESIAN_POINT ( 'NONE',  ( 119.2631014775786298, 0.2603800115204892296, -16.42320221600525088 ) ) ;
#23775 = CARTESIAN_POINT ( 'NONE',  ( 118.6958348109119754, -3.505236298600246325, -18.68346056562440793 ) ) ;
#23774 = CARTESIAN_POINT ( 'NONE',  ( 120.5110881442453206, -6.344957434206665248, -7.627207830600338134 ) ) ;
#23776 = CARTESIAN_POINT ( 'NONE',  ( 124.2550481442452792, -0.1624402480850797581, -16.17319339645315424 ) ) ;
#23777 = CARTESIAN_POINT ( 'NONE',  ( 113.0798948109119948, -0.4660016031367893996, -10.09054647747474043 ) ) ;
#23778 = ORIENTED_EDGE ( 'NONE', *, *, #16992, .T. ) ;
#23779 = EDGE_CURVE ( 'NONE', #13698, #15215, #38404, .T. ) ;
#23780 = VECTOR ( 'NONE', #35994, 999.9999999999998863 ) ;
#23781 = CARTESIAN_POINT ( 'NONE',  ( 122.1561614775786353, -8.899110576539710493, -16.42337572283490132 ) ) ;
#23782 = CARTESIAN_POINT ( 'NONE',  ( 122.4040527111058339, -1.267766418764731728, -16.93314635290706605 ) ) ;
#23783 = DIRECTION ( 'NONE',  ( -0.9495615000563050190, 0.3135808629537517600, 0.000000000000000000 ) ) ;
#23784 = CARTESIAN_POINT ( 'NONE',  ( 107.7044421295247929, 0.8980012041604618078, -13.39321520033831447 ) ) ;
#23785 = CARTESIAN_POINT ( 'NONE',  ( 113.8857702545248003, 0.1403307496149616695, -11.32035403202665336 ) ) ;
#23786 = CARTESIAN_POINT ( 'NONE',  ( 108.7462390045248242, 0.8980012041604421569, -15.77991374673208469 ) ) ;
#23787 = CARTESIAN_POINT ( 'NONE',  ( 123.9714148109119805, -0.4660016031367893996, -10.09054647747474043 ) ) ;
#23788 = CARTESIAN_POINT ( 'NONE',  ( 122.0427081442452817, -9.859900752359378018, -12.68260735090039759 ) ) ;
#23789 = ORIENTED_EDGE ( 'NONE', *, *, #5890, .T. ) ;
#23790 = CARTESIAN_POINT ( 'NONE',  ( 124.8790414775786246, -0.4660016031367893996, -10.09054647747474043 ) ) ;
#23791 = CARTESIAN_POINT ( 'NONE',  ( 114.2711548109119803, -0.1624402480850797581, -16.17319339645315424 ) ) ;
#23792 = CARTESIAN_POINT ( 'NONE',  ( 59.75121349346655109, -13.58877957849837870, -19.38162691376808411 ) ) ;
#23793 = CARTESIAN_POINT ( 'NONE',  ( 122.2696148109119889, -4.089484607189486809, -7.948022111789456723 ) ) ;
#23794 =( BOUNDED_SURFACE ( )  B_SPLINE_SURFACE ( 1, 2, ( 
 ( #43976, #15705, #25744, #43295, #12065, #15934, #43068, #29833, #22538, #19348, #15248, #40098, #25967, #43750, #8857, #19571, #29155, #4980, #19121, #12517, #5202, #26415, #1779, #16159, #4754, #8187, #33005, #11836, #30063, #5431, #33235, #40325, #36658, #12291, #2230, #9089, #22991, #39872, #12740, #36881, #29383, #5651, #2008, #33450, #26642, #29607, #22096, #35983, #26189, #36435, #18675, #32567, #39650, #1555, #22758, #1334, #8413, #18892, #22318, #36213, #32783, #15477, #30284, #9774, #33685 ),
 ( #2460, #23686, #37575, #19800, #17070, #6346, #3149, #27328, #27098, #30962, #41245, #23456, #10004, #23913, #44210, #37795, #2685, #20260, #26868, #44886, #34146, #5879, #27552, #41020, #23225, #6570, #16382, #13424, #20488, #2915, #12972, #13643, #20032, #41464, #37104, #16846, #40783, #37341, #9541, #6113, #33914, #34367, #30738, #16616, #10223, #40556, #9316, #30509, #44430, #13198, #44661, #12430, #1918, #26330, #32920, #26787, #32700, #1471, #9006, #8551, #29742, #11978, #2139, #8771, #43654 ) ),
 .UNSPECIFIED., .F., .F., .T. ) 
 B_SPLINE_SURFACE_WITH_KNOTS ( ( 2, 2 ),
 ( 3, 2, 2, 2, 2, 2, 2, 2, 2, 2, 2, 2, 2, 2, 2, 2, 2, 2, 2, 2, 2, 2, 2, 2, 2, 2, 2, 2, 2, 2, 2, 2, 3 ),
 ( 0.000000000000000000, 1.000000000000000000 ),
 ( 0.000000000000000000, 0.03125000000000000000, 0.06250000000000000000, 0.09375000000000000000, 0.1250000000000000000, 0.1562500000000000000, 0.1875000000000000000, 0.2187500000000000000, 0.2500000000000000000, 0.2812500000000000000, 0.3125000000000000000, 0.3437500000000000000, 0.3750000000000000000, 0.4062500000000000000, 0.4375000000000000000, 0.4687500000000000000, 0.5000000000000000000, 0.5312500000000000000, 0.5625000000000000000, 0.5937500000000000000, 0.6250000000000000000, 0.6562500000000000000, 0.6875000000000000000, 0.7187500000000000000, 0.7500000000000000000, 0.7812500000000000000, 0.8125000000000000000, 0.8437500000000000000, 0.8750000000000000000, 0.9062500000000000000, 0.9375000000000000000, 0.9687500000000000000, 1.000000000000000000 ),
 .UNSPECIFIED. ) 
 GEOMETRIC_REPRESENTATION_ITEM ( )  RATIONAL_B_SPLINE_SURFACE ( (
 ( 1.000000000000000000, 0.9238795325112869605, 1.000000000000000000, 0.9238795325112869605, 1.000000000000000000, 0.9238795325112869605, 1.000000000000000000, 0.9238795325112869605, 1.000000000000000000, 0.9238795325112869605, 1.000000000000000000, 0.9238795325112869605, 1.000000000000000000, 0.9238795325112869605, 1.000000000000000000, 0.9238795325112869605, 1.000000000000000000, 0.9238795325112869605, 1.000000000000000000, 0.9238795325112869605, 1.000000000000000000, 0.9238795325112869605, 1.000000000000000000, 0.9238795325112869605, 1.000000000000000000, 0.9238795325112869605, 1.000000000000000000, 0.9238795325112869605, 1.000000000000000000, 0.9238795325112869605, 1.000000000000000000, 0.9238795325112869605, 1.000000000000000000, 0.9238795325112869605, 1.000000000000000000, 0.9238795325112869605, 1.000000000000000000, 0.9238795325112869605, 1.000000000000000000, 0.9238795325112869605, 1.000000000000000000, 0.9238795325112869605, 1.000000000000000000, 0.9238795325112869605, 1.000000000000000000, 0.9238795325112869605, 1.000000000000000000, 0.9238795325112869605, 1.000000000000000000, 0.9238795325112869605, 1.000000000000000000, 0.9238795325112869605, 1.000000000000000000, 0.9238795325112869605, 1.000000000000000000, 0.9238795325112869605, 1.000000000000000000, 0.9238795325112869605, 1.000000000000000000, 0.9238795325112869605, 1.000000000000000000, 0.9238795325112869605, 1.000000000000000000, 0.9238795325112869605, 1.000000000000000000),
 ( 1.000000000000000000, 0.9238795325112869605, 1.000000000000000000, 0.9238795325112869605, 1.000000000000000000, 0.9238795325112869605, 1.000000000000000000, 0.9238795325112869605, 1.000000000000000000, 0.9238795325112869605, 1.000000000000000000, 0.9238795325112869605, 1.000000000000000000, 0.9238795325112869605, 1.000000000000000000, 0.9238795325112869605, 1.000000000000000000, 0.9238795325112869605, 1.000000000000000000, 0.9238795325112869605, 1.000000000000000000, 0.9238795325112869605, 1.000000000000000000, 0.9238795325112869605, 1.000000000000000000, 0.9238795325112869605, 1.000000000000000000, 0.9238795325112869605, 1.000000000000000000, 0.9238795325112869605, 1.000000000000000000, 0.9238795325112869605, 1.000000000000000000, 0.9238795325112869605, 1.000000000000000000, 0.9238795325112869605, 1.000000000000000000, 0.9238795325112869605, 1.000000000000000000, 0.9238795325112869605, 1.000000000000000000, 0.9238795325112869605, 1.000000000000000000, 0.9238795325112869605, 1.000000000000000000, 0.9238795325112869605, 1.000000000000000000, 0.9238795325112869605, 1.000000000000000000, 0.9238795325112869605, 1.000000000000000000, 0.9238795325112869605, 1.000000000000000000, 0.9238795325112869605, 1.000000000000000000, 0.9238795325112869605, 1.000000000000000000, 0.9238795325112869605, 1.000000000000000000, 0.9238795325112869605, 1.000000000000000000, 0.9238795325112869605, 1.000000000000000000, 0.9238795325112869605, 1.000000000000000000) ) ) 
 REPRESENTATION_ITEM ( '' )  SURFACE ( )  );
#23795 = CARTESIAN_POINT ( 'NONE',  ( 121.3619881442452879, -4.089484607189486809, -7.948022111789456723 ) ) ;
#23796 = CARTESIAN_POINT ( 'NONE',  ( 119.7402798109119715, -2.529232162391097383, -8.971805383624054997 ) ) ;
#23797 = CARTESIAN_POINT ( 'NONE',  ( 111.9453614775786434, -1.561330072975668060, -17.79121239304076596 ) ) ;
#23798 = CARTESIAN_POINT ( 'NONE',  ( 122.7993923109119692, -0.4387604401700512802, -15.73000352943951619 ) ) ;
#23799 = CARTESIAN_POINT ( 'NONE',  ( 114.3024890045248156, -9.868328341294098749, -11.32035403202665869 ) ) ;
#23800 = ORIENTED_EDGE ( 'NONE', *, *, #42891, .F. ) ;
#23801 = CARTESIAN_POINT ( 'NONE',  ( 124.8286333359170186, -2.311015703046761960, -18.04188382666269774 ) ) ;
#23802 = CARTESIAN_POINT ( 'NONE',  ( 113.1366214775786432, -7.643976991954077427, -18.09477374809248928 ) ) ;
#23803 = CARTESIAN_POINT ( 'NONE',  ( 125.5030348109119558, -6.222761293078241884, -8.102969835052219238 ) ) ;
#23804 = EDGE_CURVE ( 'NONE', #1801, #14918, #22064, .T. ) ;
#23805 = CIRCLE ( 'NONE', #29602, 5.999999999999997335 ) ;
#23806 = CARTESIAN_POINT ( 'NONE',  ( 107.1488171295247867, 0.1403307496149613920, -13.39321520033831447 ) ) ;
#23807 = CARTESIAN_POINT ( 'NONE',  ( 109.8574890045248509, -9.868328341294098749, -11.32035403202665869 ) ) ;
#23808 = CARTESIAN_POINT ( 'NONE',  ( 122.7801548109119665, -6.222761293078241884, -8.102969835052219238 ) ) ;
#23809 = LINE ( 'NONE', #24627, #39030 ) ;
#23810 = CARTESIAN_POINT ( 'NONE',  ( 115.4056881442453459, -2.084020599724406786, -8.691656652584148546 ) ) ;
#23811 = CARTESIAN_POINT ( 'NONE',  ( 124.4252281442452812, -9.261995988541697145, -16.69588392320189030 ) ) ;
#23812 = VERTEX_POINT ( 'NONE', #35729 ) ;
#23813 = VECTOR ( 'NONE', #1280, 999.9999999999998863 ) ;
#23814 = CARTESIAN_POINT ( 'NONE',  ( 123.1772414775786189, -5.574606645277164318, -18.38911715685844683 ) ) ;
#23815 = CARTESIAN_POINT ( 'NONE',  ( 118.8092881442453290, -9.988377603198976828, -10.36322818467138340 ) ) ;
#23816 = CARTESIAN_POINT ( 'NONE',  ( 124.1983214775786166, -8.166667518702819706, -8.995218007635861213 ) ) ;
#23817 = LINE ( 'NONE', #35149, #35326 ) ;
#23818 = ORIENTED_EDGE ( 'NONE', *, *, #15561, .T. ) ;
#23819 = CARTESIAN_POINT ( 'NONE',  ( 128.2184548109119930, -4.863998795839242995, -13.39321520033831447 ) ) ;
#23820 = CIRCLE ( 'NONE', #1241, 2.999999999999999556 ) ;
#23821 = CARTESIAN_POINT ( 'NONE',  ( 123.4041481442452834, -10.30919188438810075, -12.61870101168855918 ) ) ;
#23822 = ADVANCED_FACE ( 'NONE', ( #32537, #25935 ), #32086, .F. ) ;
#23823 = CARTESIAN_POINT ( 'NONE',  ( 116.0864081442453113, -0.1624402480850797581, -16.17319339645315424 ) ) ;
#23824 = CARTESIAN_POINT ( 'NONE',  ( 113.7606148109119886, -7.894159318335828068, -9.358103419637847864 ) ) ;
#23825 = DIRECTION ( 'NONE',  ( -0.7871354856660162103, -0.4483307682966942709, -0.4235767337848251879 ) ) ;
#23826 = CARTESIAN_POINT ( 'NONE',  ( 121.4797829359119987, -5.367793381288652910, -18.78638297431638904 ) ) ;
#23827 = ORIENTED_EDGE ( 'NONE', *, *, #2188, .F. ) ;
#23828 = CARTESIAN_POINT ( 'NONE',  ( 89.78938736644981589, -26.75858941326842810, -11.54476601486570964 ) ) ;
#23829 = CARTESIAN_POINT ( 'NONE',  ( 125.2231329858083910, 1.832718407601616750, -10.45069729728725605 ) ) ;
#23830 = CARTESIAN_POINT ( 'NONE',  ( 115.3442858795247759, -0.7896495226426338832, -17.46756447353520159 ) ) ;
#23831 = TOROIDAL_SURFACE ( 'NONE', #36904, 6.132259260909269649, 1.000000000000000000 ) ;
#23832 = DIRECTION ( 'NONE',  ( 0.000000000000000000, 0.000000000000000000, -1.000000000000000000 ) ) ;
#23833 = CARTESIAN_POINT ( 'NONE',  ( 122.6099748109119929, -0.8288870151387760510, -10.36305467784173118 ) ) ;
#23834 = CARTESIAN_POINT ( 'NONE',  ( 113.8740681442453138, -9.859900752359374465, -12.68260735090039404 ) ) ;
#23835 = ORIENTED_EDGE ( 'NONE', *, *, #469, .F. ) ;
#23836 = FACE_OUTER_BOUND ( 'NONE', #29280, .T. ) ;
#23837 = CARTESIAN_POINT ( 'NONE',  ( 114.3846081442453197, 0.4262465694468514643, -12.03445270309931736 ) ) ;
#23838 = VECTOR ( 'NONE', #39591, 1000.000000000000000 ) ;
#23839 = CARTESIAN_POINT ( 'NONE',  ( 70.19189222814998175, -100.0979043305785581, -53.24182196210380624 ) ) ;
#23840 = CARTESIAN_POINT ( 'NONE',  ( -1.307700928565892706, -16.07486664983353819, -18.19321520033831519 ) ) ;
#23842 = FACE_OUTER_BOUND ( 'NONE', #44215, .T. ) ;
#23841 = CARTESIAN_POINT ( 'NONE',  ( 66.04840902401572578, -36.51491089899629827, -5.214988841577086198 ) ) ;
#23843 = CARTESIAN_POINT ( 'NONE',  ( 126.0135748109119902, -1.833838273342660141, -17.42832698103878286 ) ) ;
#23844 = ORIENTED_EDGE ( 'NONE', *, *, #36698, .T. ) ;
#23845 = CARTESIAN_POINT ( 'NONE',  ( 113.3068014775786594, -8.166667518702817929, -8.995218007635859436 ) ) ;
#23846 = CARTESIAN_POINT ( 'NONE',  ( 113.5449902882355104, -1.135392229370320694, -17.10942237759953954 ) ) ;
#23847 = CARTESIAN_POINT ( 'NONE',  ( 107.5655358795247736, -8.402594152722688392, -9.854619843455216355 ) ) ;
#23848 = CARTESIAN_POINT ( 'NONE',  ( 125.3328548109119964, -0.8288870151387760510, -10.36305467784173118 ) ) ;
#23849 = AXIS2_PLACEMENT_3D ( 'NONE', #42822, #29579, #11808 ) ;
#23850 = CARTESIAN_POINT ( 'NONE',  ( 122.2696148109119889, -5.574606645277164318, -18.38911715685844683 ) ) ;
#23851 = CARTESIAN_POINT ( 'NONE',  ( 73.07463722459043254, -52.71812238298048214, -33.39556644922822670 ) ) ;
#23852 = CARTESIAN_POINT ( 'NONE',  ( 114.0246765045248196, -2.791137627527939813, -8.388885654883777576 ) ) ;
#23853 = DIRECTION ( 'NONE',  ( 0.8636456077245089347, -0.5040994586965590329, 0.000000000000000000 ) ) ;
#23854 = CARTESIAN_POINT ( 'NONE',  ( 85.82015659721905365, -25.99489077589524300, -13.39321520033831625 ) ) ;
#23855 = CARTESIAN_POINT ( 'NONE',  ( 113.9875214775786532, -8.899110576539710493, -16.42337572283490132 ) ) ;
#23856 = ADVANCED_FACE ( 'NONE', ( #19087 ), #35956, .T. ) ;
#23857 = CARTESIAN_POINT ( 'NONE',  ( 108.4684265045247997, -7.250697342233347165, -19.15521520033831138 ) ) ;
#23858 = DIRECTION ( 'NONE',  ( 0.000000000000000000, 0.000000000000000000, -1.000000000000000000 ) ) ;
#23859 = CARTESIAN_POINT ( 'NONE',  ( 113.6774108795247997, -8.938348069036489818, -9.318865927141430916 ) ) ;
#23860 = CARTESIAN_POINT ( 'NONE',  ( 123.4041481442452834, -10.30919188438810075, -12.61870101168855918 ) ) ;
#23861 = CARTESIAN_POINT ( 'NONE',  ( 124.7088614775786226, 0.2603800115204892296, -16.42320221600525088 ) ) ;
#23862 = CARTESIAN_POINT ( 'NONE',  ( 115.1359265045248321, -7.250697342233347165, -19.15521520033830427 ) ) ;
#23863 = CARTESIAN_POINT ( 'NONE',  ( 119.7169148109119874, -9.988377603198976828, -10.36322818467138340 ) ) ;
#23864 = CARTESIAN_POINT ( 'NONE',  ( 70.19189222814998175, -84.91840466455968794, -47.17007500872661296 ) ) ;
#23865 = ORIENTED_EDGE ( 'NONE', *, *, #23937, .T. ) ;
#23866 = CARTESIAN_POINT ( 'NONE',  ( 113.1366214775786432, -7.643976991954077427, -18.09477374809248928 ) ) ;
#23867 = CARTESIAN_POINT ( 'NONE',  ( 124.7655881442452852, 0.5811942927096110934, -14.16772938898807510 ) ) ;
#23868 = CARTESIAN_POINT ( 'NONE',  ( 123.0637881442452937, -0.4660016031367893996, -10.09054647747474043 ) ) ;
#23869 = CARTESIAN_POINT ( 'NONE',  ( 113.9307948109119906, 0.9020085738987339008, -11.91225656197089222 ) ) ;
#23870 = CIRCLE ( 'NONE', #19479, 1.610000000000000986 ) ;
#23871 = CARTESIAN_POINT ( 'NONE',  ( 112.2289948109119848, -7.643976991954077427, -18.09477374809248928 ) ) ;
#23872 = ORIENTED_EDGE ( 'NONE', *, *, #34917, .F. ) ;
#23873 = CARTESIAN_POINT ( 'NONE',  ( 116.5402214775786405, -9.565557343593413364, -10.61323700422348004 ) ) ;
#23874 = CARTESIAN_POINT ( 'NONE',  ( 106.5237390045248418, 0.8980012041604421569, -15.77991374673208469 ) ) ;
#23875 = CARTESIAN_POINT ( 'NONE',  ( 123.9146881442452894, -10.15424416112533912, -14.75197769757731336 ) ) ;
#23876 = CARTESIAN_POINT ( 'NONE',  ( 116.8280838815325495, -1.500009456265160912, -17.40504711518565628 ) ) ;
#23877 = CARTESIAN_POINT ( 'NONE',  ( 113.6774108795247997, -8.938348069036489818, -9.318865927141430916 ) ) ;
#23878 = EDGE_LOOP ( 'NONE', ( #9542, #38560, #30739, #7087 ) ) ;
#23879 = TOROIDAL_SURFACE ( 'NONE', #21671, 2.200000000000000178, 0.2000000000000000111 ) ;
#23880 = DIRECTION ( 'NONE',  ( -0.000000000000000000, -0.9284778069183721172, -0.3713878862591650232 ) ) ;
#23881 = CARTESIAN_POINT ( 'NONE',  ( 125.2761281442453054, -10.63000616557722466, -14.87417383870573495 ) ) ;
#23882 = DIRECTION ( 'NONE',  ( 1.000000000000000000, 0.000000000000000000, -0.000000000000000000 ) ) ;
#23883 =( LENGTH_UNIT ( ) NAMED_UNIT ( * ) SI_UNIT ( .MILLI., .METRE. ) );
#23884 = CARTESIAN_POINT ( 'NONE',  ( 116.3388580172722584, 2.269312398334672132, -6.503032629903105821 ) ) ;
#23885 = CARTESIAN_POINT ( 'NONE',  ( 124.6336743332493313, -9.305111785269604141, -15.72189022787271284 ) ) ;
#23886 = CARTESIAN_POINT ( 'NONE',  ( 105.2735827545248810, -6.936859964151250502, -8.388885654883777576 ) ) ;
#23887 = CARTESIAN_POINT ( 'NONE',  ( 115.5559231242421703, -1.016270020561755860, -17.26805140881366896 ) ) ;
#23888 = CARTESIAN_POINT ( 'NONE',  ( 119.8870948109119752, -9.261995988541697145, -16.69588392320189030 ) ) ;
#23889 = CARTESIAN_POINT ( 'NONE',  ( 122.7993923109119692, -0.4387604401700486711, -15.73000352943951263 ) ) ;
#23890 = CARTESIAN_POINT ( 'NONE',  ( 88.28425963449632263, -11.60945497031996787, -18.64321520033831803 ) ) ;
#23892 = CARTESIAN_POINT ( 'NONE',  ( 125.4463081442452932, -5.638512984488999180, -18.83840828888717311 ) ) ;
#23891 = AXIS2_PLACEMENT_3D ( 'NONE', #17051, #34568, #37778 ) ;
#23893 = CARTESIAN_POINT ( 'NONE',  ( 119.7736414775786358, 0.1319031606808879209, -14.10382304977623669 ) ) ;
#23894 = VERTEX_POINT ( 'NONE', #11805 ) ;
#23895 = CARTESIAN_POINT ( 'NONE',  ( 71.49305703095983233, -68.66289132450961574, -45.53212498594413660 ) ) ;
#23896 = CARTESIAN_POINT ( 'NONE',  ( 118.5256548109119876, -0.4660016031367893996, -10.09054647747474043 ) ) ;
#23897 = CARTESIAN_POINT ( 'NONE',  ( 125.7299414775786346, 0.9020085738987339008, -11.91225656197089222 ) ) ;
#23898 = CARTESIAN_POINT ( 'NONE',  ( 115.1220548109119761, -1.833838273342658809, -17.42832698103878286 ) ) ;
#23899 = CARTESIAN_POINT ( 'NONE',  ( 113.1366214775786432, -7.643976991954077427, -18.09477374809248928 ) ) ;
#23900 = CARTESIAN_POINT ( 'NONE',  ( 109.2324108795247923, -8.938348069036489818, -9.318865927141430916 ) ) ;
#23901 = CARTESIAN_POINT ( 'NONE',  ( 105.6208483795248299, -8.402594152722688392, -16.93181055722141792 ) ) ;
#23902 = CARTESIAN_POINT ( 'NONE',  ( 115.6915515045247531, -2.477300249445798297, -7.631215200338321125 ) ) ;
#23903 = CARTESIAN_POINT ( 'NONE',  ( 117.9583881442453048, 0.1319031606808879209, -14.10382304977623669 ) ) ;
#23904 = CARTESIAN_POINT ( 'NONE',  ( 119.7736414775786358, 0.1319031606808879209, -14.10382304977623669 ) ) ;
#23905 = CARTESIAN_POINT ( 'NONE',  ( 124.1190016859119680, -0.6942167230862511529, -9.935906262978004833 ) ) ;
#23906 = CARTESIAN_POINT ( 'NONE',  ( 119.7434548109119703, -7.554583864224885481, -18.48844787311982785 ) ) ;
#23907 = CARTESIAN_POINT ( 'NONE',  ( 108.3989733795247759, -1.325403438956436419, -9.854619843455211026 ) ) ;
#23908 = ORIENTED_EDGE ( 'NONE', *, *, #18626, .F. ) ;
#23909 = DIRECTION ( 'NONE',  ( 0.000000000000000000, 0.000000000000000000, -1.000000000000000000 ) ) ;
#23910 = CARTESIAN_POINT ( 'NONE',  ( 112.6828081442453282, -7.893985811506177619, -18.51759400769804742 ) ) ;
#23911 = DIRECTION ( 'NONE',  ( 0.000000000000000000, 0.000000000000000000, 1.000000000000000000 ) ) ;
#23912 = DIRECTION ( 'NONE',  ( -0.9498278979187092519, -0.3127730236694430399, 0.000000000000000000 ) ) ;
#23913 = CARTESIAN_POINT ( 'NONE',  ( 120.0907204359119760, -10.25716656981731489, -12.88942061488890545 ) ) ;
#23914 = EDGE_LOOP ( 'NONE', ( #17417, #13491, #20997, #35372, #10145 ) ) ;
#23915 = CARTESIAN_POINT ( 'NONE',  ( 113.8857702545248145, -10.62599879583958540, -15.77991374673209179 ) ) ;
#23916 = EDGE_CURVE ( 'NONE', #20552, #7363, #43708, .T. ) ;
#23917 = ORIENTED_EDGE ( 'NONE', *, *, #34668, .F. ) ;
#23918 = CARTESIAN_POINT ( 'NONE',  ( 121.7023481442452777, -9.261995988541697145, -16.69588392320189030 ) ) ;
#23919 = CARTESIAN_POINT ( 'NONE',  ( 111.7184548109119788, -9.261995988541697145, -16.69588392320189030 ) ) ;
#23920 = CARTESIAN_POINT ( 'NONE',  ( 117.2776681442452968, -4.153390946401321671, -8.397313243818183892 ) ) ;
#23921 = SURFACE_STYLE_FILL_AREA ( #2694 ) ;
#23922 = DIRECTION ( 'NONE',  ( 1.000000000000000000, 0.000000000000000000, 0.000000000000000000 ) ) ;
#23923 = CARTESIAN_POINT ( 'NONE',  ( 123.3474214775786209, -9.988377603198976828, -10.36322818467138340 ) ) ;
#23924 = CARTESIAN_POINT ( 'NONE',  ( 119.4332814775786318, -0.4660016031367893996, -10.09054647747474043 ) ) ;
#23925 = EDGE_CURVE ( 'NONE', #1444, #39549, #2154, .T. ) ;
#23926 = CARTESIAN_POINT ( 'NONE',  ( 107.0793640045248196, 0.1403307496149616695, -15.46607636864997204 ) ) ;
#23927 = TOROIDAL_SURFACE ( 'NONE', #10092, 1.500000000000000000, 0.5000000000000000000 ) ;
#23928 = CARTESIAN_POINT ( 'NONE',  ( 112.1155414775786454, -10.15424416112533912, -14.75197769757731336 ) ) ;
#23929 = FACE_OUTER_BOUND ( 'NONE', #37670, .T. ) ;
#23930 = ORIENTED_EDGE ( 'NONE', *, *, #17514, .F. ) ;
#23931 = CARTESIAN_POINT ( 'NONE',  ( 118.1285681442453068, -7.893985811506177619, -18.51759400769804742 ) ) ;
#23932 = CARTESIAN_POINT ( 'NONE',  ( 120.9241579359119925, -5.444069387712269226, -19.60292469916370450 ) ) ;
#23933 = CARTESIAN_POINT ( 'NONE',  ( 116.9940348109119839, -9.988377603198976828, -10.36322818467138340 ) ) ;
#23934 = ORIENTED_EDGE ( 'NONE', *, *, #30046, .T. ) ;
#23935 = DIRECTION ( 'NONE',  ( -0.9908103287288504424, 0.1352586133457950590, 0.000000000000000000 ) ) ;
#23936 = CARTESIAN_POINT ( 'NONE',  ( 113.8173414775786512, -9.565557343593413364, -10.61323700422348004 ) ) ;
#23937 = EDGE_CURVE ( 'NONE', #13343, #6245, #26156, .T. ) ;
#23938 = CARTESIAN_POINT ( 'NONE',  ( 78.10590893225656828, -57.76403841489356239, -0.8923062931455548741 ) ) ;
#23939 = CARTESIAN_POINT ( 'NONE',  ( 114.9518748109119883, -7.643976991954077427, -18.09477374809248928 ) ) ;
#23940 = EDGE_CURVE ( 'NONE', #29903, #17270, #4503, .T. ) ;
#23941 = EDGE_CURVE ( 'NONE', #16862, #26433, #26434, .T. ) ;
#23942 = CARTESIAN_POINT ( 'NONE',  ( 70.19189222814998175, -54.26662894631272849, -34.90947156805651019 ) ) ;
#23943 = CARTESIAN_POINT ( 'NONE',  ( 117.5613014775786525, -10.15424416112533912, -14.75197769757731336 ) ) ;
#23944 = CARTESIAN_POINT ( 'NONE',  ( 70.19189222814998175, -67.83330054016514055, -40.33609291459782753 ) ) ;
#23945 = CARTESIAN_POINT ( 'NONE',  ( 116.4834948109119779, -7.894159318335828068, -9.358103419637847864 ) ) ;
#23946 = CARTESIAN_POINT ( 'NONE',  ( 114.6682414775786469, -1.561330072975668060, -17.79121239304076596 ) ) ;
#23947 = CARTESIAN_POINT ( 'NONE',  ( 123.7022829359119811, -4.283928203966213211, -7.183505701512925334 ) ) ;
#23948 = CARTESIAN_POINT ( 'NONE',  ( 116.9373081442452929, -8.166667518702817929, -8.995218007635861213 ) ) ;
#23949 = CARTESIAN_POINT ( 'NONE',  ( 112.3424481442453384, -3.505236298600246325, -18.68346056562440793 ) ) ;
#23950 = CARTESIAN_POINT ( 'NONE',  ( 118.0151148109119816, 0.4262465694468514643, -12.03445270309931736 ) ) ;
#23951 = ORIENTED_EDGE ( 'NONE', *, *, #43477, .T. ) ;
#23952 = CARTESIAN_POINT ( 'NONE',  ( 113.5904348109119866, -7.893985811506177619, -18.51759400769804742 ) ) ;
#23953 = CARTESIAN_POINT ( 'NONE',  ( 107.0793640045248196, -10.62599879583958717, -11.00651665394454604 ) ) ;
#23954 = CARTESIAN_POINT ( 'NONE',  ( 104.9263171295248327, 0.1403307496149613920, -13.39321520033831447 ) ) ;
#23955 = CARTESIAN_POINT ( 'NONE',  ( 72.75524511225664526, -29.99489077589588959, -12.39321520033834645 ) ) ;
#23956 = CARTESIAN_POINT ( 'NONE',  ( 70.19189222814998175, -53.54563792646638376, -34.62107767336419073 ) ) ;
#23957 = CARTESIAN_POINT ( 'NONE',  ( 117.9583881442453048, -10.30919188438810075, -12.61870101168855918 ) ) ;
#23958 = VERTEX_POINT ( 'NONE', #42819 ) ;
#23959 = LINE ( 'NONE', #17116, #2291 ) ;
#23960 = CARTESIAN_POINT ( 'NONE',  ( 118.3554748109119998, -9.565557343593413364, -10.61323700422348004 ) ) ;
#23961 = DIRECTION ( 'NONE',  ( -1.000000000000000000, 1.156482317317869950E-15, 0.000000000000000000 ) ) ;
#23962 = CARTESIAN_POINT ( 'NONE',  ( 122.4965214775786251, -10.30919188438810075, -12.61870101168855918 ) ) ;
#23963 = CARTESIAN_POINT ( 'NONE',  ( 106.7320983795247855, -0.7896495226426338832, -9.318865927141430916 ) ) ;
#23964 = CARTESIAN_POINT ( 'NONE',  ( 89.23646529747401246, -10.12233672812908480, -13.85167412278761923 ) ) ;
#23965 = ORIENTED_EDGE ( 'NONE', *, *, #9969, .T. ) ;
#23966 = CARTESIAN_POINT ( 'NONE',  ( 125.4463081442452932, -4.153390946401325223, -8.397313243818185668 ) ) ;
#23967 = CARTESIAN_POINT ( 'NONE',  ( 125.2194014775786286, -10.30919188438810075, -12.61870101168855918 ) ) ;
#23968 = CARTESIAN_POINT ( 'NONE',  ( 117.3343948109119737, -6.222761293078241884, -8.102969835052219238 ) ) ;
#23969 = CARTESIAN_POINT ( 'NONE',  ( 82.89134431723762475, -31.13449359622123680, -21.94632144483577818 ) ) ;
#23970 = CARTESIAN_POINT ( 'NONE',  ( 120.3976348109119812, -1.834011780172310813, -8.268836392978581529 ) ) ;
#23971 = CARTESIAN_POINT ( 'NONE',  ( 87.02785693856107230, -26.75858941326842810, -11.54476601486570964 ) ) ;
#23972 = CARTESIAN_POINT ( 'NONE',  ( 126.4162218615806950, -1.128033623988350831, -9.922867115873357236 ) ) ;
#23973 = CARTESIAN_POINT ( 'NONE',  ( 122.4397948109119767, -0.1624402480850797581, -16.17319339645315424 ) ) ;
#23974 = ORIENTED_EDGE ( 'NONE', *, *, #36448, .T. ) ;
#23975 = EDGE_CURVE ( 'NONE', #2531, #24941, #4727, .T. ) ;
#23976 = DIRECTION ( 'NONE',  ( -0.000000000000000000, -0.9284778069183721172, -0.3713878862591650232 ) ) ;
#23977 = CARTESIAN_POINT ( 'NONE',  ( 116.7671281442453335, -1.834011780172310813, -8.268836392978581529 ) ) ;
#23978 = CARTESIAN_POINT ( 'NONE',  ( 125.7299414775786346, -10.15424416112533912, -14.75197769757731336 ) ) ;
#23979 = EDGE_LOOP ( 'NONE', ( #25577, #13532, #7264, #20963 ) ) ;
#23980 = CARTESIAN_POINT ( 'NONE',  ( 121.6881423109119709, -9.959231468620755479, -10.70263013195267199 ) ) ;
#23981 = ADVANCED_FACE ( 'NONE', ( #12033 ), #36400, .T. ) ;
#23982 = CARTESIAN_POINT ( 'NONE',  ( 135.9690293846647364, -1.212003134032930030, -8.725841475540576653 ) ) ;
#23983 = CARTESIAN_POINT ( 'NONE',  ( 121.2485348109119769, -0.4660016031367893996, -10.09054647747474043 ) ) ;
#23984 = CARTESIAN_POINT ( 'NONE',  ( 109.7185827545247889, -2.477300249445798297, -19.15521520033831138 ) ) ;
#23985 = CARTESIAN_POINT ( 'NONE',  ( 119.3198281442452924, -9.859900752359374465, -12.68260735090039404 ) ) ;
#23986 = VERTEX_POINT ( 'NONE', #44628 ) ;
#23987 = ORIENTED_EDGE ( 'NONE', *, *, #12196, .T. ) ;
#23988 = CARTESIAN_POINT ( 'NONE',  ( 112.3424481442453384, -6.344957434206662583, -7.627207830600332805 ) ) ;
#23989 = LINE ( 'NONE', #27179, #26943 ) ;
#23990 = AXIS2_PLACEMENT_3D ( 'NONE', #317, #6270, #20190 ) ;
#23991 = LINE ( 'NONE', #37427, #30238 ) ;
#23992 = EDGE_CURVE ( 'NONE', #23245, #44431, #33419, .T. ) ;
#23993 = CARTESIAN_POINT ( 'NONE',  ( 59.62174278132244609, -14.86814543204979344, -18.19321520033831519 ) ) ;
#23994 = CARTESIAN_POINT ( 'NONE',  ( 120.7379948109119709, -10.63000616557722466, -14.87417383870573495 ) ) ;
#23995 = DIRECTION ( 'NONE',  ( 0.000000000000000000, 0.000000000000000000, 1.000000000000000000 ) ) ;
#23996 = CARTESIAN_POINT ( 'NONE',  ( 94.20708369096698220, -26.81768470319947184, -13.17593392366846672 ) ) ;
#23997 = CARTESIAN_POINT ( 'NONE',  ( 120.7379948109119709, -10.63000616557722466, -14.87417383870573495 ) ) ;
#23999 = CARTESIAN_POINT ( 'NONE',  ( 119.4900081442453086, -7.643976991954077427, -18.09477374809248928 ) ) ;
#23998 = CARTESIAN_POINT ( 'NONE',  ( 118.3554748109119998, 0.2603800115204892296, -16.42320221600525088 ) ) ;
#24000 = EDGE_CURVE ( 'NONE', #34550, #19575, #43078, .T. ) ;
#24001 = FACE_OUTER_BOUND ( 'NONE', #14034, .T. ) ;
#24002 = CARTESIAN_POINT ( 'NONE',  ( 115.7460481442453357, 0.9020085738987339008, -11.91225656197089222 ) ) ;
#24003 = ORIENTED_EDGE ( 'NONE', *, *, #13050, .T. ) ;
#24004 = CARTESIAN_POINT ( 'NONE',  ( 126.5241148109119393, -9.565557343593413364, -10.61323700422348004 ) ) ;
#24005 = FACE_OUTER_BOUND ( 'NONE', #14200, .T. ) ;
#24006 = CARTESIAN_POINT ( 'NONE',  ( 107.9128015045248219, -2.477300249445798297, -7.631215200338321125 ) ) ;
#24007 = CARTESIAN_POINT ( 'NONE',  ( 110.7603796295247918, -4.863998795839590272, -8.388885654883775800 ) ) ;
#24008 = CARTESIAN_POINT ( 'NONE',  ( 106.8710046295248759, -4.863998795839590272, -7.631215200338315796 ) ) ;
#24009 = CARTESIAN_POINT ( 'NONE',  ( 122.0427081442452817, 0.5811942927096110934, -14.16772938898807510 ) ) ;
#24010 = CARTESIAN_POINT ( 'NONE',  ( 123.6877814775786533, -6.222761293078241884, -8.102969835052219238 ) ) ;
#24011 = ORIENTED_EDGE ( 'NONE', *, *, #13042, .F. ) ;
#24012 = CARTESIAN_POINT ( 'NONE',  ( 125.9568481442452850, -6.344957434206665248, -7.627207830600338134 ) ) ;
#24013 = CARTESIAN_POINT ( 'NONE',  ( 110.2742077545248094, -7.250697342233347165, -7.631215200338321125 ) ) ;
#24014 = CARTESIAN_POINT ( 'NONE',  ( 59.62174278132245320, -14.86814543204979344, -19.39321520033831803 ) ) ;
#24015 = CARTESIAN_POINT ( 'NONE',  ( 124.2550481442452792, -9.988377603198980381, -10.36322818467138518 ) ) ;
#24016 = CARTESIAN_POINT ( 'NONE',  ( 119.7169148109119874, -9.988377603198976828, -10.36322818467138340 ) ) ;
#24017 = CARTESIAN_POINT ( 'NONE',  ( 69.36136150295220659, -55.33724551716493067, -32.23290681585656614 ) ) ;
#24018 = CARTESIAN_POINT ( 'NONE',  ( 112.0588148109119828, 0.5811942927096154232, -14.16772938898807155 ) ) ;
#24019 = CARTESIAN_POINT ( 'NONE',  ( 123.0077516859119839, -0.6942167230862511529, -9.935906262978006609 ) ) ;
#24020 = CARTESIAN_POINT ( 'NONE',  ( 114.9275671295247889, 0.1403307496149613920, -13.39321520033831447 ) ) ;
#24021 = EDGE_LOOP ( 'NONE', ( #4651, #32161, #15972, #21492, #27775 ) ) ;
#24022 = DIRECTION ( 'NONE',  ( 0.000000000000000000, -0.3713878862591650232, 0.9284778069183718952 ) ) ;
#24023 = CARTESIAN_POINT ( 'NONE',  ( 112.1722681442453222, -8.899110576539710493, -16.42337572283490132 ) ) ;
#24024 = CARTESIAN_POINT ( 'NONE',  ( 122.6667014775786413, -2.084020599724406786, -8.691656652584148546 ) ) ;
#24025 = CARTESIAN_POINT ( 'NONE',  ( 109.7185827545247889, -6.936859964151250502, -8.388885654883777576 ) ) ;
#24026 = CARTESIAN_POINT ( 'NONE',  ( 106.0375671295248310, 0.1403307496149613920, -13.39321520033831447 ) ) ;
#24028 = AXIS2_PLACEMENT_3D ( 'NONE', #37837, #16888, #26911 ) ;
#24027 = CARTESIAN_POINT ( 'NONE',  ( 122.2128881442453263, -7.643976991954077427, -18.09477374809248928 ) ) ;
#24029 = CARTESIAN_POINT ( 'NONE',  ( 115.9162281442453093, -5.574606645277164318, -18.38911715685844683 ) ) ;
#24030 = CARTESIAN_POINT ( 'NONE',  ( 113.5904348109119866, -2.084020599724406786, -8.691656652584148546 ) ) ;
#24031 = EDGE_LOOP ( 'NONE', ( #38908, #19859, #29780, #44623, #30733, #42040 ) ) ;
#24032 = CARTESIAN_POINT ( 'NONE',  ( 121.2019704359119743, -10.25716656981731489, -12.88942061488890545 ) ) ;
#24033 = CARTESIAN_POINT ( 'NONE',  ( 119.4332814775786318, -0.4660016031367893996, -10.09054647747474043 ) ) ;
#24034 = DIRECTION ( 'NONE',  ( 0.000000000000000000, -0.9242245927363028635, -0.3818493186865930533 ) ) ;
#24035 = ORIENTED_EDGE ( 'NONE', *, *, #10852, .T. ) ;
#24036 = VECTOR ( 'NONE', #42720, 1000.000000000000000 ) ;
#24037 = CARTESIAN_POINT ( 'NONE',  ( 125.4584548109119737, -4.863998795839242995, -13.39321520033831447 ) ) ;
#24038 = EDGE_CURVE ( 'NONE', #36181, #24368, #21832, .T. ) ;
#24039 = ORIENTED_EDGE ( 'NONE', *, *, #37414, .T. ) ;
#24040 = CARTESIAN_POINT ( 'NONE',  ( 113.5904348109119866, -2.084020599724406786, -8.691656652584148546 ) ) ;
#24041 = CARTESIAN_POINT ( 'NONE',  ( 115.2922348109119781, 0.4262465694468514643, -12.03445270309931736 ) ) ;
#24042 = DIRECTION ( 'NONE',  ( 1.000000000000000000, 0.000000000000000000, -0.000000000000000000 ) ) ;
#24043 = CARTESIAN_POINT ( 'NONE',  ( 120.2296266859119953, -0.06289925094097943703, -9.412459353600674206 ) ) ;
#24044 = ORIENTED_EDGE ( 'NONE', *, *, #9731, .F. ) ;
#24045 = CARTESIAN_POINT ( 'NONE',  ( 60.06931813437628875, -14.72076136720887085, -8.603412892520118760 ) ) ;
#24046 = CARTESIAN_POINT ( 'NONE',  ( 62.79048817247115721, -3.396818809258673966, -7.619046670169436375 ) ) ;
#24047 = CARTESIAN_POINT ( 'NONE',  ( 106.6626452545248611, -9.868328341294098749, -15.46607636864997204 ) ) ;
#24048 = ADVANCED_FACE ( 'NONE', ( #6076 ), #16351, .T. ) ;
#24049 = VECTOR ( 'NONE', #43518, 1000.000000000000114 ) ;
#24050 = DIRECTION ( 'NONE',  ( 0.000000000000000000, 1.000000000000000000, 0.000000000000000000 ) ) ;
#24051 = CARTESIAN_POINT ( 'NONE',  ( 124.6521348109119884, -7.894159318335828068, -9.358103419637847864 ) ) ;
#24052 = CARTESIAN_POINT ( 'NONE',  ( 114.5547881442453217, -4.153390946401321671, -8.397313243818183892 ) ) ;
#24053 = CARTESIAN_POINT ( 'NONE',  ( 72.54180985774836188, -54.15757082072580175, -34.13667568191001322 ) ) ;
#24054 = VERTEX_POINT ( 'NONE', #19317 ) ;
#24055 = DIRECTION ( 'NONE',  ( -0.4225728684367167642, 0.9063289528979890930, 0.000000000000000000 ) ) ;
#24056 = CARTESIAN_POINT ( 'NONE',  ( 112.2857214775786474, -5.574606645277164318, -18.38911715685844683 ) ) ;
#24057 = AXIS2_PLACEMENT_3D ( 'NONE', #17493, #31177, #6566 ) ;
#24058 = CARTESIAN_POINT ( 'NONE',  ( 61.69189222814998175, -40.21211973637273474, -4.893215200338314474 ) ) ;
#24059 = CARTESIAN_POINT ( 'NONE',  ( 116.5944421295247793, -4.863998795839590272, -8.393215200338314474 ) ) ;
#24061 = CARTESIAN_POINT ( 'NONE',  ( 125.9568481442452850, -6.344957434206665248, -7.627207830600338134 ) ) ;
#24060 = DIRECTION ( 'NONE',  ( 1.387778780781445676E-17, -0.9284778069183720062, -0.3713878862591650232 ) ) ;
#24062 = CARTESIAN_POINT ( 'NONE',  ( 125.1626748109119802, -0.1624402480850797581, -16.17319339645315424 ) ) ;
#24063 = ORIENTED_EDGE ( 'NONE', *, *, #9731, .T. ) ;
#24064 = AXIS2_PLACEMENT_3D ( 'NONE', #22349, #29865, #5681 ) ;
#24065 = CARTESIAN_POINT ( 'NONE',  ( 113.3635281442453504, -9.988377603198976828, -10.36322818467138340 ) ) ;
#24066 = DIRECTION ( 'NONE',  ( 0.000000000000000000, 0.000000000000000000, -1.000000000000000000 ) ) ;
#24067 = CARTESIAN_POINT ( 'NONE',  ( 115.2748327545248657, -2.477300249445798297, -19.15521520033831138 ) ) ;
#24068 = CARTESIAN_POINT ( 'NONE',  ( 126.1837548109119496, 0.4262465694468514643, -12.03445270309931736 ) ) ;
#24069 = CARTESIAN_POINT ( 'NONE',  ( 124.3117748109119844, 0.1319031606808879209, -14.10382304977623669 ) ) ;
#24070 = CARTESIAN_POINT ( 'NONE',  ( 110.7603796295247918, -4.863998795839590272, -8.388885654883775800 ) ) ;
#24071 = DIRECTION ( 'NONE',  ( -0.000000000000000000, -0.9284778069183721172, -0.3713878862591650232 ) ) ;
#24072 = CARTESIAN_POINT ( 'NONE',  ( 119.7434548109119703, -2.527210466738042172, -8.967976844669124148 ) ) ;
#24073 = CARTESIAN_POINT ( 'NONE',  ( 114.1009748109119784, -5.574606645277164318, -18.38911715685844683 ) ) ;
#24074 = CARTESIAN_POINT ( 'NONE',  ( 106.6626452545248611, 0.8980012041604421569, -11.00651665394454071 ) ) ;
#24075 = CARTESIAN_POINT ( 'NONE',  ( 117.2294421295247844, -9.690077956319688823, -4.893215200338314474 ) ) ;
#24076 = CARTESIAN_POINT ( 'NONE',  ( 108.2600671295247992, -10.62599879583958540, -13.39321520033831447 ) ) ;
#24077 = CARTESIAN_POINT ( 'NONE',  ( 124.8790414775786246, -0.4660016031367893996, -10.09054647747474043 ) ) ;
#24078 = CARTESIAN_POINT ( 'NONE',  ( 112.1722681442453222, -8.899110576539710493, -16.42337572283490132 ) ) ;
#24079 = CARTESIAN_POINT ( 'NONE',  ( 72.69189222814998175, -41.76310523276723785, -24.39321520033831447 ) ) ;
#24080 = CARTESIAN_POINT ( 'NONE',  ( 120.2274548109119934, 0.5811942927096110934, -14.16772938898807510 ) ) ;
#24081 = CARTESIAN_POINT ( 'NONE',  ( 117.2776681442452968, -5.638512984488999180, -18.83840828888717311 ) ) ;
#24082 = VERTEX_POINT ( 'NONE', #29802 ) ;
#24083 = CARTESIAN_POINT ( 'NONE',  ( 125.1626748109119802, -9.988377603198980381, -10.36322818467138518 ) ) ;
#24084 = CARTESIAN_POINT ( 'NONE',  ( 123.0070614775786169, 0.9020085738987339008, -11.91225656197089222 ) ) ;
#24085 = AXIS2_PLACEMENT_3D ( 'NONE', #17111, #6613, #31001 ) ;
#24086 = CARTESIAN_POINT ( 'NONE',  ( 114.6682414775786469, -1.561330072975668060, -17.79121239304076596 ) ) ;
#24087 = CARTESIAN_POINT ( 'NONE',  ( 114.7816948109119863, -9.859900752359374465, -12.68260735090039404 ) ) ;
#24088 = ORIENTED_EDGE ( 'NONE', *, *, #30782, .F. ) ;
#24089 = CARTESIAN_POINT ( 'NONE',  ( 117.0507614775786465, 0.1319031606808879209, -14.10382304977623669 ) ) ;
#24090 = CIRCLE ( 'NONE', #8061, 2.999999999999998224 ) ;
#24091 = CARTESIAN_POINT ( 'NONE',  ( 116.2565881442452991, -9.261995988541697145, -16.69588392320189030 ) ) ;
#24092 = CARTESIAN_POINT ( 'NONE',  ( 124.1983214775786166, -1.833838273342659697, -17.42832698103878286 ) ) ;
#24093 = CARTESIAN_POINT ( 'NONE',  ( 116.8579880548923029, -0.4409650872748420158, -16.24658638300725499 ) ) ;
#24094 = CARTESIAN_POINT ( 'NONE',  ( 115.6915515045247531, -2.477300249445798297, -7.631215200338321125 ) ) ;
#24095 = VERTEX_POINT ( 'NONE', #34115 ) ;
#24096 = VECTOR ( 'NONE', #2166, 1000.000000000000000 ) ;
#24097 = DIRECTION ( 'NONE',  ( -0.000000000000000000, -0.9284778069183718952, -0.3713878862591649677 ) ) ;
#24098 = CARTESIAN_POINT ( 'NONE',  ( 125.5030348109119558, -3.383040157471821630, -19.15922257007629170 ) ) ;
#24099 = CARTESIAN_POINT ( 'NONE',  ( 116.5944421295247793, -9.868328341294093420, -13.39321520033831447 ) ) ;
#24100 = DIRECTION ( 'NONE',  ( 0.000000000000000000, -0.3818493186865927203, 0.9242245927363029745 ) ) ;
#24101 = ADVANCED_FACE ( 'NONE', ( #30252 ), #21106, .T. ) ;
#24102 = CARTESIAN_POINT ( 'NONE',  ( 116.3077641307500301, 2.279349991481241400, -6.542802709738571920 ) ) ;
#24103 = CARTESIAN_POINT ( 'NONE',  ( 112.2857214775786474, -5.574606645277164318, -18.38911715685844683 ) ) ;
#24104 = CARTESIAN_POINT ( 'NONE',  ( 107.6349890045248401, -9.868328341294098749, -11.32035403202665869 ) ) ;
#24105 = LINE ( 'NONE', #20902, #27331 ) ;
#24106 = CARTESIAN_POINT ( 'NONE',  ( 118.0718414775786300, -9.261995988541697145, -16.69588392320189030 ) ) ;
#24107 = CARTESIAN_POINT ( 'NONE',  ( 136.5266930377887888, -4.268568095932804951, -19.09868834485503442 ) ) ;
#24108 = AXIS2_PLACEMENT_3D ( 'NONE', #28603, #11273, #25181 ) ;
#24109 = CYLINDRICAL_SURFACE ( 'NONE', #4832, 11.00000000000000000 ) ;
#24110 = DIRECTION ( 'NONE',  ( -0.5735764363510450492, -0.3127926500124816878, 0.7570804645221038687 ) ) ;
#24111 = CARTESIAN_POINT ( 'NONE',  ( 120.8514481442452961, -2.084020599724406786, -8.691656652584148546 ) ) ;
#24112 = ORIENTED_EDGE ( 'NONE', *, *, #38229, .T. ) ;
#24113 = CARTESIAN_POINT ( 'NONE',  ( 125.1059481442452750, -8.166667518702819706, -8.995218007635861213 ) ) ;
#24114 = CARTESIAN_POINT ( 'NONE',  ( 120.6245414775786458, -9.988377603198976828, -10.36322818467138340 ) ) ;
#24115 = CARTESIAN_POINT ( 'NONE',  ( 88.46631044337289040, -25.99489077589524300, -13.39321520033831625 ) ) ;
#24116 = CARTESIAN_POINT ( 'NONE',  ( 117.1074881442453233, 0.4262465694468514643, -12.03445270309931736 ) ) ;
#24117 = CARTESIAN_POINT ( 'NONE',  ( 112.1722681442453222, -8.899110576539710493, -16.42337572283490132 ) ) ;
#24118 = CARTESIAN_POINT ( 'NONE',  ( 109.4407702545248355, -10.62599879583958717, -15.77991374673208469 ) ) ;
#24119 = CARTESIAN_POINT ( 'NONE',  ( 105.6903015045248253, -6.936859964151250502, -18.39754474579286025 ) ) ;
#24120 = CARTESIAN_POINT ( 'NONE',  ( 82.78592324864024476, -31.79260405195279304, -23.13461678765773044 ) ) ;
#24121 = CARTESIAN_POINT ( 'NONE',  ( 118.1852948109119836, -4.153390946401325223, -8.397313243818185668 ) ) ;
#24122 = CIRCLE ( 'NONE', #20477, 8.800000000000000711 ) ;
#24123 = CARTESIAN_POINT ( 'NONE',  ( 121.3052614775786111, -7.643976991954077427, -18.09477374809248928 ) ) ;
#24124 = DIRECTION ( 'NONE',  ( 0.000000000000000000, -0.3818493186865936084, 0.9242245927363024194 ) ) ;
#24125 = CARTESIAN_POINT ( 'NONE',  ( 120.4379860609119675, -6.564341423271550902, -7.887810678476487425 ) ) ;
#24126 = CARTESIAN_POINT ( 'NONE',  ( 107.7738952545248310, -9.868328341294098749, -15.46607636864997204 ) ) ;
#24127 = AXIS2_PLACEMENT_3D ( 'NONE', #17582, #13273, #31036 ) ;
#24128 = CARTESIAN_POINT ( 'NONE',  ( 65.19189222814998175, -41.76310523276723785, -4.893215200338314474 ) ) ;
#24129 = CARTESIAN_POINT ( 'NONE',  ( 115.0653281442453277, -6.344957434206662583, -7.627207830600332805 ) ) ;
#24130 = CARTESIAN_POINT ( 'NONE',  ( 114.1009748109119784, -4.089484607189486809, -7.948022111789456723 ) ) ;
#24131 = CARTESIAN_POINT ( 'NONE',  ( 71.02242295334774269, -99.02728775972636299, -55.91838671430374319 ) ) ;
#24132 = ORIENTED_EDGE ( 'NONE', *, *, #43997, .F. ) ;
#24133 = CARTESIAN_POINT ( 'NONE',  ( 123.4428756873493569, -2.767871776335191658, -14.93546065993297667 ) ) ;
#24134 = VERTEX_POINT ( 'NONE', #2652 ) ;
#24135 = CARTESIAN_POINT ( 'NONE',  ( 122.0994348109119443, 0.9020085738987339008, -11.91225656197089222 ) ) ;
#24136 = CARTESIAN_POINT ( 'NONE',  ( 126.6942948109119840, -8.899110576539710493, -16.42337572283490132 ) ) ;
#24137 = CARTESIAN_POINT ( 'NONE',  ( 118.1852948109119836, -4.153390946401325223, -8.397313243818185668 ) ) ;
#24138 = FILL_AREA_STYLE ('',( #3807 ) ) ;
#24139 = CARTESIAN_POINT ( 'NONE',  ( 71.02242295334774269, -49.68958793485906256, -36.18347876678663511 ) ) ;
#24140 = CARTESIAN_POINT ( 'NONE',  ( 123.2906948109119867, -8.166667518702819706, -8.995218007635861213 ) ) ;
#24141 = CARTESIAN_POINT ( 'NONE',  ( 117.6180281442453150, -0.4660016031367893996, -10.09054647747474043 ) ) ;
#24142 = CARTESIAN_POINT ( 'NONE',  ( 109.6491296295247793, -4.863998795839590272, -8.388885654883775800 ) ) ;
#24143 = AXIS2_PLACEMENT_3D ( 'NONE', #22903, #15394, #19485 ) ;
#24144 = CARTESIAN_POINT ( 'NONE',  ( 112.3424481442453384, -3.505236298600246325, -18.68346056562440793 ) ) ;
#24145 = PRODUCT_DEFINITION ( 'UNKNOWN', '', #26417, #17842 ) ;
#24146 = LINE ( 'NONE', #7241, #36652 ) ;
#24147 = EDGE_LOOP ( 'NONE', ( #35830, #39970, #20242, #28684, #5615, #30243 ) ) ;
#24148 = CARTESIAN_POINT ( 'NONE',  ( 116.8238548109119819, -4.089484607189486809, -7.948022111789456723 ) ) ;
#24149 = LINE ( 'NONE', #41700, #3812 ) ;
#24150 = CARTESIAN_POINT ( 'NONE',  ( 116.3700414775786527, -5.638512984488999180, -18.83840828888717311 ) ) ;
#24151 = ORIENTED_EDGE ( 'NONE', *, *, #42337, .F. ) ;
#24152 = CARTESIAN_POINT ( 'NONE',  ( 106.4542858795248179, -8.402594152722688392, -9.854619843455216355 ) ) ;
#24153 = AXIS2_PLACEMENT_3D ( 'NONE', #8464, #22367, #12115 ) ;
#24154 = CARTESIAN_POINT ( 'NONE',  ( 125.5030348109119558, -3.383040157471821630, -19.15922257007629170 ) ) ;
#24155 = DIRECTION ( 'NONE',  ( 1.000000000000000000, 0.000000000000000000, -0.000000000000000000 ) ) ;
#24156 = CARTESIAN_POINT ( 'NONE',  ( 113.2500748109119968, -3.505236298600246325, -18.68346056562440793 ) ) ;
#24157 = CARTESIAN_POINT ( 'NONE',  ( 89.12784890491134604, -25.23119213852205789, -15.24166438581092109 ) ) ;
#24158 = CARTESIAN_POINT ( 'NONE',  ( 116.5402214775786405, -9.565557343593413364, -10.61323700422348004 ) ) ;
#24159 = CARTESIAN_POINT ( 'NONE',  ( 120.1730908535611491, -2.239543233855044946, -18.13706010537467606 ) ) ;
#24160 = CARTESIAN_POINT ( 'NONE',  ( 118.1852948109119836, -4.153390946401325223, -8.397313243818185668 ) ) ;
#24161 = DIRECTION ( 'NONE',  ( -0.000000000000000000, -0.3818493186865896671, 0.9242245927363040847 ) ) ;
#24162 = CARTESIAN_POINT ( 'NONE',  ( 118.5823814775786360, -7.643976991954077427, -18.09477374809248928 ) ) ;
#24163 = CARTESIAN_POINT ( 'NONE',  ( 120.9241579359119925, -5.444069387712269226, -19.60292469916370450 ) ) ;
#24164 = CARTESIAN_POINT ( 'NONE',  ( 116.0296814775786345, -8.166667518702817929, -8.995218007635861213 ) ) ;
#24165 = CARTESIAN_POINT ( 'NONE',  ( 125.9001214775786224, -4.089484607189486809, -7.948022111789456723 ) ) ;
#24166 = CARTESIAN_POINT ( 'NONE',  ( 118.6958348109119754, -3.505236298600246325, -18.68346056562440793 ) ) ;
#24167 = VERTEX_POINT ( 'NONE', #33882 ) ;
#24168 = CARTESIAN_POINT ( 'NONE',  ( 117.3911214775786505, -1.561330072975668504, -17.79121239304076951 ) ) ;
#24169 = CARTESIAN_POINT ( 'NONE',  ( 109.3018640045248304, -10.62599879583958717, -11.00651665394454604 ) ) ;
#24170 = DIRECTION ( 'NONE',  ( 0.5735764363510499342, 0.3127926500124801890, -0.7570804645221008711 ) ) ;
#24171 = LINE ( 'NONE', #23955, #44396 ) ;
#24172 = CARTESIAN_POINT ( 'NONE',  ( 61.69189222814998175, -49.76310523276723785, -19.39321520033831447 ) ) ;
#24173 = B_SPLINE_CURVE_WITH_KNOTS ( 'NONE', 3,
 ( #15669, #19991, #2422, #37067, #29348, #29797, #29571, #16120, #26379, #16346 ),
 .UNSPECIFIED., .F., .F.,
 ( 4, 3, 3, 4 ),
 ( 0.000000000000000000, 0.0001671877548681284921, 0.0003343755096277730159, 0.0006463528481650619413 ),
 .UNSPECIFIED. ) ;
#24174 = CARTESIAN_POINT ( 'NONE',  ( 120.7379948109119709, -10.63000616557722466, -14.87417383870573495 ) ) ;
#24175 = ORIENTED_EDGE ( 'NONE', *, *, #34484, .T. ) ;
#24176 = CARTESIAN_POINT ( 'NONE',  ( 126.3063647503472851, -8.168462963394901521, -9.582415806495719224 ) ) ;
#24177 = CARTESIAN_POINT ( 'NONE',  ( 116.5969481442453031, -9.859900752359374465, -12.68260735090039404 ) ) ;
#24178 = CARTESIAN_POINT ( 'NONE',  ( 124.8223148109119904, -10.15424416112542083, -14.75197769757788713 ) ) ;
#24179 = CARTESIAN_POINT ( 'NONE',  ( 124.4252281442452812, -9.261995988541697145, -16.69588392320189030 ) ) ;
#24180 = CARTESIAN_POINT ( 'NONE',  ( 111.8716296295247901, -4.863998795839590272, -8.388885654883775800 ) ) ;
#24181 = CARTESIAN_POINT ( 'NONE',  ( 123.9584548109119737, -4.863998795839242995, -13.39321520033831447 ) ) ;
#24182 = ORIENTED_EDGE ( 'NONE', *, *, #2301, .F. ) ;
#24183 = CARTESIAN_POINT ( 'NONE',  ( 112.7962614775786676, -3.383040157471821630, -19.15922257007629170 ) ) ;
#24184 = CARTESIAN_POINT ( 'NONE',  ( 111.7751814775786556, -7.893985811506177619, -18.51759400769804742 ) ) ;
#24185 = CARTESIAN_POINT ( 'NONE',  ( 121.6456214775786293, -10.63000616557722466, -14.87417383870573495 ) ) ;
#24186 = CARTESIAN_POINT ( 'NONE',  ( 116.1998614775786507, 0.4262465694468514643, -12.03445270309931736 ) ) ;
#24187 = DIRECTION ( 'NONE',  ( 1.000000000000000000, 0.000000000000000000, -0.000000000000000000 ) ) ;
#24188 = CARTESIAN_POINT ( 'NONE',  ( 120.7379948109119709, -10.63000616557722466, -14.87417383870573495 ) ) ;
#24189 = EDGE_CURVE ( 'NONE', #38773, #37700, #16583, .T. ) ;
#24190 = DIRECTION ( 'NONE',  ( 1.000000000000000000, 0.000000000000000000, 0.000000000000000000 ) ) ;
#24191 = CARTESIAN_POINT ( 'NONE',  ( 122.4965214775786251, 0.1319031606808879209, -14.10382304977623669 ) ) ;
#24192 = VERTEX_POINT ( 'NONE', #23652 ) ;
#24193 = EDGE_CURVE ( 'NONE', #17457, #42907, #27680, .T. ) ;
#24194 = ADVANCED_FACE ( 'NONE', ( #6310 ), #44440, .T. ) ;
#24195 = CARTESIAN_POINT ( 'NONE',  ( 67.30914723170953096, -55.81513550964497483, -36.42337668688479368 ) ) ;
#24196 = CARTESIAN_POINT ( 'NONE',  ( 115.6893214775786447, 0.5811942927096154232, -14.16772938898807155 ) ) ;
#24197 = CARTESIAN_POINT ( 'NONE',  ( 135.9373687277985425, -8.517831521581461729, -18.06820524589254262 ) ) ;
#24198 = ORIENTED_EDGE ( 'NONE', *, *, #6922, .F. ) ;
#24199 = CARTESIAN_POINT ( 'NONE',  ( 124.1884548109119777, -7.554583864224885481, -18.48844787311982785 ) ) ;
#24200 = CARTESIAN_POINT ( 'NONE',  ( 61.69189222814998175, -57.16572941273946640, -4.036072343195455936 ) ) ;
#24201 = CARTESIAN_POINT ( 'NONE',  ( 123.1205148109119563, -1.834011780172310813, -8.268836392978581529 ) ) ;
#24202 = CARTESIAN_POINT ( 'NONE',  ( 107.4960827545248350, -2.477300249445798297, -19.15521520033831138 ) ) ;
#24203 = CARTESIAN_POINT ( 'NONE',  ( 119.7169148109119874, -0.1624402480850797581, -16.17319339645315424 ) ) ;
#24204 = EDGE_LOOP ( 'NONE', ( #12276, #12756, #24284, #41293, #4723, #17305, #28574, #10073, #25110, #8861, #42299, #44963, #28387, #17396, #33274, #10461, #37654, #7060, #12823, #2310, #12173, #37345, #37384, #4379, #44701, #8755, #37909, #28238, #36283, #15515, #44616, #26691, #3929, #10816, #20128, #1331, #34622, #17405, #24385, #14908, #31695, #22723, #30963, #40762, #9775 ) ) ;
#24205 = VERTEX_POINT ( 'NONE', #1977 ) ;
#24206 = AXIS2_PLACEMENT_3D ( 'NONE', #10980, #38777, #4348 ) ;
#24207 = CARTESIAN_POINT ( 'NONE',  ( 113.0798948109119948, -0.4660016031367893996, -10.09054647747474043 ) ) ;
#24208 = CARTESIAN_POINT ( 'NONE',  ( 122.8936081442453059, -9.565557343593413364, -10.61323700422348004 ) ) ;
#24209 = DIRECTION ( 'NONE',  ( -0.7962509850245453880, -0.6049664196031389052, 0.000000000000000000 ) ) ;
#24210 = CARTESIAN_POINT ( 'NONE',  ( 122.4397948109119767, -9.988377603198976828, -10.36322818467138340 ) ) ;
#24211 = EDGE_CURVE ( 'NONE', #37424, #10826, #2885, .T. ) ;
#24212 = CARTESIAN_POINT ( 'NONE',  ( 111.2647102085435193, -8.897589485953298905, -16.42540022429002633 ) ) ;
#24213 = CARTESIAN_POINT ( 'NONE',  ( 117.0341443147880511, -2.395992375830784837, -17.92872468182854107 ) ) ;
#24214 = CARTESIAN_POINT ( 'NONE',  ( 119.4900081442453086, -1.834011780172310813, -8.268836392978581529 ) ) ;
#24216 = CARTESIAN_POINT ( 'NONE',  ( 119.0361948109119652, -2.084020599724406786, -8.691656652584148546 ) ) ;
#24215 = CARTESIAN_POINT ( 'NONE',  ( 119.6034614775786196, -6.344957434206665248, -7.627207830600338134 ) ) ;
#24217 = CARTESIAN_POINT ( 'NONE',  ( 69.87170781386352303, -25.28162009068048732, -5.721420406450495655 ) ) ;
#24218 = CARTESIAN_POINT ( 'NONE',  ( 117.0507614775786465, -10.30919188438810075, -12.61870101168855918 ) ) ;
#24219 = EDGE_CURVE ( 'NONE', #10084, #18111, #43715, .T. ) ;
#24220 = VERTEX_POINT ( 'NONE', #15902 ) ;
#24221 = CARTESIAN_POINT ( 'NONE',  ( 112.6260814775786514, -9.261995988541697145, -16.69588392320189030 ) ) ;
#24222 = EDGE_CURVE ( 'NONE', #12877, #219, #43944, .T. ) ;
#24223 = CARTESIAN_POINT ( 'NONE',  ( 125.7194014775786286, -9.814174330883794539, -12.68911139247586739 ) ) ;
#24224 = CARTESIAN_POINT ( 'NONE',  ( 109.0935046295247872, -4.863998795839590272, -7.631215200338315796 ) ) ;
#24225 = CARTESIAN_POINT ( 'NONE',  ( 108.1211608795247798, -1.325403438956436419, -16.93181055722141792 ) ) ;
#24226 = CARTESIAN_POINT ( 'NONE',  ( 107.1488171295247867, -10.62599879583958540, -13.39321520033831447 ) ) ;
#24227 = CARTESIAN_POINT ( 'NONE',  ( 79.79010115959992788, 5.106172230548759572, -19.89321520033831447 ) ) ;
#24228 = CARTESIAN_POINT ( 'NONE',  ( 113.1933481442453058, -4.089484607189486809, -7.948022111789456723 ) ) ;
#24229 = ORIENTED_EDGE ( 'NONE', *, *, #31988, .F. ) ;
#24230 = CARTESIAN_POINT ( 'NONE',  ( 126.2404814775786264, -9.261995988541697145, -16.69588392320189030 ) ) ;
#24231 = CARTESIAN_POINT ( 'NONE',  ( 110.3436608795247764, -8.938348069036489818, -9.318865927141430916 ) ) ;
#24232 = DIRECTION ( 'NONE',  ( -0.000000000000000000, -0.9284778069183721172, -0.3713878862591650232 ) ) ;
#24233 = CARTESIAN_POINT ( 'NONE',  ( 124.3685014775786328, -10.63000616557722466, -14.87417383870573495 ) ) ;
#24234 = CARTESIAN_POINT ( 'NONE',  ( 123.6310548109119765, -5.638512984488999180, -18.83840828888717311 ) ) ;
#24235 = CARTESIAN_POINT ( 'NONE',  ( 70.19189222814998175, -65.04786711941002864, -39.22192925581976652 ) ) ;
#24236 = CARTESIAN_POINT ( 'NONE',  ( 112.2857214775786474, -4.089484607189486809, -7.948022111789456723 ) ) ;
#24237 = DIRECTION ( 'NONE',  ( 0.9609149988134843001, -0.1028163501681632064, 0.2570431154366505933 ) ) ;
#24238 = CARTESIAN_POINT ( 'NONE',  ( 115.4137390045248566, -9.868328341294098749, -11.32035403202665869 ) ) ;
#24239 = ORIENTED_EDGE ( 'NONE', *, *, #17797, .T. ) ;
#24240 = CARTESIAN_POINT ( 'NONE',  ( 123.7184548109119788, -4.863998795839242995, -13.39321520033831447 ) ) ;
#24241 = CARTESIAN_POINT ( 'NONE',  ( 114.1577014775786552, -3.505236298600246325, -18.68346056562440793 ) ) ;
#24242 = VECTOR ( 'NONE', #10715, 1000.000000000000000 ) ;
#24243 = CARTESIAN_POINT ( 'NONE',  ( 111.8319081442453182, -5.638512984488999180, -18.83840828888717311 ) ) ;
#24244 = CARTESIAN_POINT ( 'NONE',  ( 115.3442858795247759, -0.7896495226426338832, -17.46756447353520159 ) ) ;
#24245 = CARTESIAN_POINT ( 'NONE',  ( 106.3153796295248412, -4.863998795839590272, -8.388885654883775800 ) ) ;
#24246 = EDGE_CURVE ( 'NONE', #7134, #19765, #26199, .T. ) ;
#24247 = CARTESIAN_POINT ( 'NONE',  ( 120.6245414775786458, -0.1624402480850797581, -16.17319339645315424 ) ) ;
#24248 = CARTESIAN_POINT ( 'NONE',  ( 116.5969481442453031, -9.859900752359374465, -12.68260735090039404 ) ) ;
#24249 = CARTESIAN_POINT ( 'NONE',  ( 125.3895814775786448, -7.893985811506177619, -18.51759400769804742 ) ) ;
#24250 = VERTEX_POINT ( 'NONE', #358 ) ;
#24251 = EDGE_CURVE ( 'NONE', #39662, #17122, #30591, .T. ) ;
#24252 = EDGE_CURVE ( 'NONE', #13605, #29406, #6540, .T. ) ;
#24253 = AXIS2_PLACEMENT_3D ( 'NONE', #28897, #36388, #22051 ) ;
#24254 = CARTESIAN_POINT ( 'NONE',  ( 121.7575954359119805, 0.5291689781388270175, -13.89700978578772705 ) ) ;
#24255 = CIRCLE ( 'NONE', #8220, 2.999999999999999556 ) ;
#24256 = LINE ( 'NONE', #16971, #9116 ) ;
#24257 = CARTESIAN_POINT ( 'NONE',  ( 113.3635281442453504, -0.1624402480850797581, -16.17319339645315424 ) ) ;
#24258 = ORIENTED_EDGE ( 'NONE', *, *, #32827, .T. ) ;
#24259 = CARTESIAN_POINT ( 'NONE',  ( 61.63318325272354770, -19.46990085680238636, -12.39321520033831447 ) ) ;
#24260 = ORIENTED_EDGE ( 'NONE', *, *, #21137, .T. ) ;
#24261 = CARTESIAN_POINT ( 'NONE',  ( 120.0005481442453146, -4.153390946401325223, -8.397313243818185668 ) ) ;
#24262 = B_SPLINE_CURVE_WITH_KNOTS ( 'NONE', 3,
 ( #6405, #13911, #24399, #16668, #9831, #34197, #1731, #22711, #38503, #36609 ),
 .UNSPECIFIED., .F., .F.,
 ( 4, 3, 3, 4 ),
 ( 1.226634733346699927E-18, 0.0002476486808869855175, 0.0004952973797228700211, 0.0009368823381787680761 ),
 .UNSPECIFIED. ) ;
#24263 = CARTESIAN_POINT ( 'NONE',  ( 114.8384214775786489, -10.15424416112533912, -14.75197769757731336 ) ) ;
#24264 = CARTESIAN_POINT ( 'NONE',  ( 69.69189222814998175, -41.76310523276723785, -6.393215200338315363 ) ) ;
#24265 = CARTESIAN_POINT ( 'NONE',  ( 123.5633766859119760, -9.033780868592240054, -16.85052413769862056 ) ) ;
#24266 = EDGE_LOOP ( 'NONE', ( #13008, #34161, #27813, #25747, #6730 ) ) ;
#24267 = CIRCLE ( 'NONE', #15529, 20.00000000000000355 ) ;
#24268 = CARTESIAN_POINT ( 'NONE',  ( 59.24641515291911986, -13.72835195454734425, -7.393215200338313586 ) ) ;
#24269 = CARTESIAN_POINT ( 'NONE',  ( 63.36814607564562607, -3.176177366285224846, -7.750926265059984388 ) ) ;
#24270 = CARTESIAN_POINT ( 'NONE',  ( 106.5237390045248418, -9.868328341294098749, -11.32035403202665869 ) ) ;
#24271 = VECTOR ( 'NONE', #6267, 1000.000000000000000 ) ;
#24272 = DIRECTION ( 'NONE',  ( -0.000000000000000000, -0.9284778069183721172, -0.3713878862591650232 ) ) ;
#24273 = CARTESIAN_POINT ( 'NONE',  ( 123.8012348109119642, -9.565557343593413364, -10.61323700422348004 ) ) ;
#24274 = CARTESIAN_POINT ( 'NONE',  ( 117.2776681442452968, -4.153390946401325223, -8.397313243818185668 ) ) ;
#24275 = CARTESIAN_POINT ( 'NONE',  ( 119.8259526359456260, -1.179503403430467667, -17.05068175419387089 ) ) ;
#24276 = EDGE_LOOP ( 'NONE', ( #14348, #27928, #11580, #40827 ) ) ;
#24277 = DIRECTION ( 'NONE',  ( 0.000000000000000000, 0.000000000000000000, 1.000000000000000000 ) ) ;
#24278 = CARTESIAN_POINT ( 'NONE',  ( 119.1496481442453046, -6.222761293078241884, -8.102969835052219238 ) ) ;
#24279 = CARTESIAN_POINT ( 'NONE',  ( 115.2922348109119781, 0.4262465694468514643, -12.03445270309931736 ) ) ;
#24280 = CIRCLE ( 'NONE', #6067, 15.90000000000000036 ) ;
#24281 = DIRECTION ( 'NONE',  ( 1.000000000000000000, 0.000000000000000000, 0.000000000000000000 ) ) ;
#24282 = LINE ( 'NONE', #10151, #38530 ) ;
#24283 = CARTESIAN_POINT ( 'NONE',  ( 112.3424481442453384, -6.344957434206662583, -7.627207830600332805 ) ) ;
#24284 = ORIENTED_EDGE ( 'NONE', *, *, #9401, .F. ) ;
#24285 = CARTESIAN_POINT ( 'NONE',  ( 115.1787814775786387, -9.988377603198976828, -10.36322818467138340 ) ) ;
#24286 = CARTESIAN_POINT ( 'NONE',  ( 114.1577014775786552, -6.344957434206662583, -7.627207830600333693 ) ) ;
#24287 = CARTESIAN_POINT ( 'NONE',  ( 107.0099108795247815, -1.325403438956436419, -16.93181055722141792 ) ) ;
#24288 = CARTESIAN_POINT ( 'NONE',  ( 112.9664414775786412, 0.5811942927096154232, -14.16772938898807155 ) ) ;
#24289 = ADVANCED_FACE ( 'NONE', ( #17257 ), #17690, .T. ) ;
#24290 = CARTESIAN_POINT ( 'NONE',  ( 115.7460481442453357, 0.9020085738987339008, -11.91225656197089222 ) ) ;
#24291 = CARTESIAN_POINT ( 'NONE',  ( 123.2339681442453241, -3.505236298600246325, -18.68346056562440793 ) ) ;
#24292 = CARTESIAN_POINT ( 'NONE',  ( 112.6609831777918913, -0.01829820670813664396, -14.64321520033831447 ) ) ;
#24293 = CARTESIAN_POINT ( 'NONE',  ( 109.4407702545248355, 0.1403307496149616695, -11.32035403202665336 ) ) ;
#24294 = CARTESIAN_POINT ( 'NONE',  ( 111.1770983795247787, -0.7896495226427380221, -9.318865927141420258 ) ) ;
#24295 = CARTESIAN_POINT ( 'NONE',  ( 109.2294563837206312, -5.167320247529568533, -18.58757576157646696 ) ) ;
#24296 = CARTESIAN_POINT ( 'NONE',  ( 118.0718414775786442, -0.8288870151387760510, -10.36305467784173118 ) ) ;
#24297 = DIRECTION ( 'NONE',  ( -0.000000000000000000, -0.9284778069183721172, -0.3713878862591650232 ) ) ;
#24298 = CARTESIAN_POINT ( 'NONE',  ( 120.5468302440515203, -2.467220198592778413, -17.83387418641524391 ) ) ;
#24299 = CARTESIAN_POINT ( 'NONE',  ( 110.2742077545248094, -7.250697342233347165, -7.631215200338321125 ) ) ;
#24300 = CARTESIAN_POINT ( 'NONE',  ( 123.1772414775786189, -4.089484607189486809, -7.948022111789456723 ) ) ;
#24301 = CARTESIAN_POINT ( 'NONE',  ( 125.8433948109119456, -1.834011780172310813, -8.268836392978581529 ) ) ;
#24302 = CARTESIAN_POINT ( 'NONE',  ( 119.9438214775786520, -2.084020599724394796, -8.691656652584146769 ) ) ;
#24303 = B_SPLINE_CURVE_WITH_KNOTS ( 'NONE', 3,
 ( #16499, #30399, #38499, #7276, #21191, #33564, #26757, #2341 ),
 .UNSPECIFIED., .F., .F.,
 ( 4, 2, 2, 4 ),
 ( 0.000000000000000000, 0.5000000000000193179, 0.7500000000000096589, 1.000000000000000000 ),
 .UNSPECIFIED. ) ;
#24304 = CARTESIAN_POINT ( 'NONE',  ( 120.1140014775786398, -1.561330072975668504, -17.79121239304076951 ) ) ;
#24305 = CARTESIAN_POINT ( 'NONE',  ( 116.7671281442453335, -1.834011780172310813, -8.268836392978581529 ) ) ;
#24306 = EDGE_LOOP ( 'NONE', ( #9999, #11625, #18273, #8436 ) ) ;
#24307 = CONICAL_SURFACE ( 'NONE', #41072, 1.610000000000000986, 0.9599310885968765916 ) ;
#24308 = CARTESIAN_POINT ( 'NONE',  ( 115.4056881442453459, -2.084020599724406786, -8.691656652584148546 ) ) ;
#24309 = CARTESIAN_POINT ( 'NONE',  ( 125.4463081442452932, -5.638512984488999180, -18.83840828888717311 ) ) ;
#24310 = CARTESIAN_POINT ( 'NONE',  ( 113.4769814775786330, -10.63000616557722466, -14.87417383870573495 ) ) ;
#24311 = CARTESIAN_POINT ( 'NONE',  ( 116.8805814775786445, -3.505236298600246325, -18.68346056562440793 ) ) ;
#24312 = EDGE_LOOP ( 'NONE', ( #40175, #31415, #8424, #21273 ) ) ;
#24313 = ADVANCED_FACE ( 'NONE', ( #34554 ), #24322, .F. ) ;
#24314 = CARTESIAN_POINT ( 'NONE',  ( 121.5321681442453183, -0.1624402480850797581, -16.17319339645315424 ) ) ;
#24315 = AXIS2_PLACEMENT_3D ( 'NONE', #749, #538, #21512 ) ;
#24316 = CARTESIAN_POINT ( 'NONE',  ( 116.0296814775786345, -8.166667518702817929, -8.995218007635861213 ) ) ;
#24317 = CARTESIAN_POINT ( 'NONE',  ( 123.7295344654666991, -4.681376030475591143, -18.56985183333092237 ) ) ;
#24318 = CARTESIAN_POINT ( 'NONE',  ( 114.7886608795247696, -8.938348069036489818, -9.318865927141430916 ) ) ;
#24319 = ORIENTED_EDGE ( 'NONE', *, *, #42051, .T. ) ;
#24320 = LINE ( 'NONE', #9738, #16240 ) ;
#24321 = CARTESIAN_POINT ( 'NONE',  ( 125.4463081442452932, -5.638512984488999180, -18.83840828888717311 ) ) ;
#24322 = PLANE ( 'NONE',  #34226 ) ;
#24323 = CARTESIAN_POINT ( 'NONE',  ( 115.2922348109119781, -10.63000616557722466, -14.87417383870573495 ) ) ;
#24324 = CARTESIAN_POINT ( 'NONE',  ( 135.9373687278040563, -10.75336585672390299, -14.11528246583558577 ) ) ;
#24325 = CARTESIAN_POINT ( 'NONE',  ( 113.4769814775786330, 0.4262465694468514643, -12.03445270309931736 ) ) ;
#24326 = CARTESIAN_POINT ( 'NONE',  ( 62.88020800785245967, -12.58185084616640204, -16.61333427033593679 ) ) ;
#24327 = CARTESIAN_POINT ( 'NONE',  ( 74.19189222814998175, -41.76310523276723785, -24.39321520033831447 ) ) ;
#24328 = CARTESIAN_POINT ( 'NONE',  ( 116.5249890045247980, -9.868328341294098749, -11.32035403202665869 ) ) ;
#24329 = CARTESIAN_POINT ( 'NONE',  ( 117.2776681442452968, -5.638512984488999180, -18.83840828888717311 ) ) ;
#24330 = AXIS2_PLACEMENT_3D ( 'NONE', #3223, #31699, #24870 ) ;
#24331 = DIRECTION ( 'NONE',  ( -0.000000000000000000, -0.9284778069183721172, -0.3713878862591650232 ) ) ;
#24332 = CARTESIAN_POINT ( 'NONE',  ( 70.19189222814998175, -70.61873396092025246, -41.45025657337532010 ) ) ;
#24333 = CARTESIAN_POINT ( 'NONE',  ( 46.47434218039879283, -17.93412427487546523, -19.39321520033831447 ) ) ;
#24334 = CARTESIAN_POINT ( 'NONE',  ( 122.6099748109119929, -0.8288870151387760510, -10.36305467784173118 ) ) ;
#24335 = VERTEX_POINT ( 'NONE', #34771 ) ;
#24336 = CARTESIAN_POINT ( 'NONE',  ( 125.8433948109119456, -1.834011780172310813, -8.268836392978581529 ) ) ;
#24337 = CARTESIAN_POINT ( 'NONE',  ( 120.2841814775786276, 0.9020085738987339008, -11.91225656197089222 ) ) ;
#24338 = CARTESIAN_POINT ( 'NONE',  ( 116.8028015045247940, -6.936859964151250502, -18.39754474579286025 ) ) ;
#24339 = CARTESIAN_POINT ( 'NONE',  ( 117.4478481442453131, -9.565557343593413364, -10.61323700422348004 ) ) ;
#24340 = CARTESIAN_POINT ( 'NONE',  ( 112.0588148109119828, -9.859900752359374465, -12.68260735090039404 ) ) ;
#24341 = DIRECTION ( 'NONE',  ( 1.000000000000000000, 0.000000000000000000, 0.000000000000000000 ) ) ;
#24342 = CARTESIAN_POINT ( 'NONE',  ( 112.0105358795247810, -0.7896495226426338832, -17.46756447353520159 ) ) ;
#24343 = CARTESIAN_POINT ( 'NONE',  ( 121.8158014775786171, -4.153390946401325223, -8.397313243818185668 ) ) ;
#24344 = CARTESIAN_POINT ( 'NONE',  ( 119.0929214775786278, -4.153390946401325223, -8.397313243818185668 ) ) ;
#24345 = CARTESIAN_POINT ( 'NONE',  ( 109.2294627447761144, -0.4939093571603179744, -10.30950732205088016 ) ) ;
#24346 = CARTESIAN_POINT ( 'NONE',  ( 122.5910329359119970, -4.283928203966213211, -7.183505701512925334 ) ) ;
#24347 = CARTESIAN_POINT ( 'NONE',  ( 107.4266296295248821, -4.863998795839590272, -8.388885654883775800 ) ) ;
#24348 = CARTESIAN_POINT ( 'NONE',  ( 113.8173414775786512, 0.2603800115204892296, -16.42320221600525088 ) ) ;
#24349 = CARTESIAN_POINT ( 'NONE',  ( 113.7606148109119886, -1.561330072975668060, -17.79121239304076596 ) ) ;
#24350 = CARTESIAN_POINT ( 'NONE',  ( 61.76986277844709861, -39.32091226840162079, -23.89321520033831803 ) ) ;
#24351 = VERTEX_POINT ( 'NONE', #31146 ) ;
#24352 = CARTESIAN_POINT ( 'NONE',  ( 61.69189222814998175, -49.76310523276723785, -19.39321520033831447 ) ) ;
#24353 = CARTESIAN_POINT ( 'NONE',  ( 121.3619881442452879, -4.089484607189486809, -7.948022111789456723 ) ) ;
#24354 = CARTESIAN_POINT ( 'NONE',  ( 112.5693548109119888, -10.63000616557722466, -14.87417383870573495 ) ) ;
#24355 = EDGE_CURVE ( 'NONE', #12871, #4353, #17465, .T. ) ;
#24356 = CARTESIAN_POINT ( 'NONE',  ( 116.8805814775786445, -3.505236298600246325, -18.68346056562440793 ) ) ;
#24357 = B_SPLINE_CURVE_WITH_KNOTS ( 'NONE', 3,
 ( #9745, #3119, #44634, #6544, #41216, #34560, #2657, #141, #44404, #27524 ),
 .UNSPECIFIED., .F., .F.,
 ( 4, 3, 3, 4 ),
 ( 0.000000000000000000, 0.0002476487219222849707, 0.0004952974148303580099, 0.0009534114850261900384 ),
 .UNSPECIFIED. ) ;
#24358 = CARTESIAN_POINT ( 'NONE',  ( 125.3895814775786448, -7.893985811506177619, -18.51759400769804742 ) ) ;
#24359 = CARTESIAN_POINT ( 'NONE',  ( 119.3198281442452924, 0.5811942927096110934, -14.16772938898807510 ) ) ;
#24360 = AXIS2_PLACEMENT_3D ( 'NONE', #918, #25098, #32595 ) ;
#24361 = CARTESIAN_POINT ( 'NONE',  ( 109.0240515045248202, -6.936859964151250502, -18.39754474579286025 ) ) ;
#24362 = CARTESIAN_POINT ( 'NONE',  ( 112.9664414775786412, -9.859900752359374465, -12.68260735090039404 ) ) ;
#24363 = DIRECTION ( 'NONE',  ( 0.000000000000000000, 0.000000000000000000, 1.000000000000000000 ) ) ;
#24364 = ORIENTED_EDGE ( 'NONE', *, *, #23099, .F. ) ;
#24365 = CARTESIAN_POINT ( 'NONE',  ( 116.7671281442453335, -1.834011780172310813, -8.268836392978581529 ) ) ;
#24366 = CARTESIAN_POINT ( 'NONE',  ( 119.7434548109119703, -7.554583864224885481, -18.48844787311982785 ) ) ;
#24367 = CARTESIAN_POINT ( 'NONE',  ( 116.0296814775786345, -8.166667518702817929, -8.995218007635861213 ) ) ;
#24368 = VERTEX_POINT ( 'NONE', #38207 ) ;
#24369 = CARTESIAN_POINT ( 'NONE',  ( 106.5237390045248418, -9.868328341294098749, -11.32035403202665869 ) ) ;
#24370 = CARTESIAN_POINT ( 'NONE',  ( -13.55927693411048196, -4.790939057849996630, -8.800639967176238088 ) ) ;
#24371 = EDGE_CURVE ( 'NONE', #13043, #5648, #17468, .T. ) ;
#24372 = DIRECTION ( 'NONE',  ( 0.9387755102040818977, -0.3445294493088592036, 0.000000000000000000 ) ) ;
#24373 = CARTESIAN_POINT ( 'NONE',  ( 124.9928017464362426, -6.058968105182603203, -18.37591834006149938 ) ) ;
#24374 = CARTESIAN_POINT ( 'NONE',  ( 70.19189222814998175, -56.33107134722149567, -35.73524133214168330 ) ) ;
#24375 = CARTESIAN_POINT ( 'NONE',  ( 119.8870948109119752, -0.8288870151387760510, -10.36305467784173118 ) ) ;
#24376 = CARTESIAN_POINT ( 'NONE',  ( 70.19189222814998175, -51.48119552555760947, -33.79530790927901052 ) ) ;
#24377 = CARTESIAN_POINT ( 'NONE',  ( 119.2631014775786298, -9.565557343593413364, -10.61323700422348004 ) ) ;
#24378 = AXIS2_PLACEMENT_3D ( 'NONE', #19279, #44586, #40482 ) ;
#24379 = DIRECTION ( 'NONE',  ( 0.000000000000000000, 0.000000000000000000, 1.000000000000000000 ) ) ;
#24380 = CARTESIAN_POINT ( 'NONE',  ( 120.7947214775786193, -0.8288870151387760510, -10.36305467784173118 ) ) ;
#24381 = CARTESIAN_POINT ( 'NONE',  ( 111.8319081442453182, -5.638512984488999180, -18.83840828888717311 ) ) ;
#24382 = CARTESIAN_POINT ( 'NONE',  ( 116.3700414775786527, -5.638512984488999180, -18.83840828888717311 ) ) ;
#24383 = AXIS2_PLACEMENT_3D ( 'NONE', #31594, #14724, #32039 ) ;
#24384 = CARTESIAN_POINT ( 'NONE',  ( 117.0507614775786465, 0.1319031606808879209, -14.10382304977623669 ) ) ;
#24385 = ORIENTED_EDGE ( 'NONE', *, *, #40070, .F. ) ;
#24386 = CARTESIAN_POINT ( 'NONE',  ( 116.0296814775786345, -8.166667518702817929, -8.995218007635861213 ) ) ;
#24387 = CARTESIAN_POINT ( 'NONE',  ( 109.1629577545248395, -7.250697342233347165, -7.631215200338321125 ) ) ;
#24388 = DIRECTION ( 'NONE',  ( 1.000000000000000000, 0.000000000000000000, -0.000000000000000000 ) ) ;
#24389 = CARTESIAN_POINT ( 'NONE',  ( 76.69189222814998175, -40.21211973637274184, -6.893215200338315363 ) ) ;
#24390 = CARTESIAN_POINT ( 'NONE',  ( 123.2768159103642063, -8.454079026182057532, -17.47208793939445215 ) ) ;
#24391 = CARTESIAN_POINT ( 'NONE',  ( 122.3263414775786373, -6.344957434206665248, -7.627207830600338134 ) ) ;
#24392 = VERTEX_POINT ( 'NONE', #27519 ) ;
#24393 = CARTESIAN_POINT ( 'NONE',  ( 127.0915067942438839, -8.936375571992021705, -9.791582253908270417 ) ) ;
#24394 = CARTESIAN_POINT ( 'NONE',  ( 119.2631014775786298, -9.565557343593413364, -10.61323700422348004 ) ) ;
#24395 = LINE ( 'NONE', #37453, #24242 ) ;
#24396 = DIRECTION ( 'NONE',  ( 0.000000000000000000, -0.4669533266896289669, -0.8842819633428519177 ) ) ;
#24397 = CARTESIAN_POINT ( 'NONE',  ( 123.2906948109119867, -8.166667518702819706, -8.995218007635861213 ) ) ;
#24398 = CARTESIAN_POINT ( 'NONE',  ( 113.1217858795247935, -8.402594152722688392, -9.854619843455216355 ) ) ;
#24399 = CARTESIAN_POINT ( 'NONE',  ( 124.2451922641554489, -8.548534124195539263, -17.65096007659765220 ) ) ;
#24400 = VERTEX_POINT ( 'NONE', #14048 ) ;
#24401 = DIRECTION ( 'NONE',  ( -0.9908103287288504424, 0.1352586133457950313, 0.000000000000000000 ) ) ;
#24402 = CARTESIAN_POINT ( 'NONE',  ( 112.7395348109119766, -5.638512984488999180, -18.83840828888717311 ) ) ;
#24403 = CARTESIAN_POINT ( 'NONE',  ( 123.5176014775786228, -9.261995988541697145, -16.69588392320189030 ) ) ;
#24404 = CARTESIAN_POINT ( 'NONE',  ( 118.4122014775786340, -9.859900752359374465, -12.68260735090039404 ) ) ;
#24405 = DIRECTION ( 'NONE',  ( 0.000000000000000000, 0.4669533266896289669, 0.8842819633428518067 ) ) ;
#24406 = CARTESIAN_POINT ( 'NONE',  ( 120.0572748109119772, -3.383040157471821630, -19.15922257007629170 ) ) ;
#24407 = CARTESIAN_POINT ( 'NONE',  ( 87.44708369096657918, -25.99489077589588604, -13.39321520033831447 ) ) ;
#24408 = CARTESIAN_POINT ( 'NONE',  ( 122.3830681442452857, -1.833838273342659697, -17.42832698103878286 ) ) ;
#24409 = ORIENTED_EDGE ( 'NONE', *, *, #15292, .F. ) ;
#24410 = CARTESIAN_POINT ( 'NONE',  ( 116.5971529312752892, -9.866503804269289191, -13.43859147813565436 ) ) ;
#24411 = CARTESIAN_POINT ( 'NONE',  ( 118.4122014775786340, 0.5811942927096110934, -14.16772938898807510 ) ) ;
#24412 = CARTESIAN_POINT ( 'NONE',  ( 135.7778351054865595, -8.526057075361061166, -18.10094121367604814 ) ) ;
#24413 = ORIENTED_EDGE ( 'NONE', *, *, #13888, .T. ) ;
#24414 = DIRECTION ( 'NONE',  ( 0.5735764363510498232, -0.3127926500124802445, 0.7570804645221007600 ) ) ;
#24415 = CARTESIAN_POINT ( 'NONE',  ( 62.63983398123977508, -12.53686781608317524, -10.05482766178462306 ) ) ;
#24416 = CARTESIAN_POINT ( 'NONE',  ( 120.9649014775786355, -3.383040157471821630, -19.15922257007629170 ) ) ;
#24417 = VECTOR ( 'NONE', #34726, 1000.000000000000114 ) ;
#24418 = CARTESIAN_POINT ( 'NONE',  ( 109.7880358795247986, -0.7896495226426338832, -17.46756447353520159 ) ) ;
#24419 = CARTESIAN_POINT ( 'NONE',  ( 121.2485348109119769, -8.899110576539710493, -16.42337572283490132 ) ) ;
#24420 = ORIENTED_EDGE ( 'NONE', *, *, #27017, .F. ) ;
#24421 = ORIENTED_EDGE ( 'NONE', *, *, #13048, .T. ) ;
#24422 = CARTESIAN_POINT ( 'NONE',  ( 114.1577014775786552, -6.344957434206662583, -7.627207830600332805 ) ) ;
#24423 = CARTESIAN_POINT ( 'NONE',  ( 125.1059481442452750, -1.833838273342660141, -17.42832698103878286 ) ) ;
#24424 = DIRECTION ( 'NONE',  ( 0.000000000000000000, 0.000000000000000000, 1.000000000000000000 ) ) ;
#24425 = CARTESIAN_POINT ( 'NONE',  ( 121.9859814775786333, 0.2603800115204892296, -16.42320221600525088 ) ) ;
#24426 = CARTESIAN_POINT ( 'NONE',  ( 109.3272331777918822, -0.01829820670803256055, -14.64321520033831447 ) ) ;
#24427 = DIRECTION ( 'NONE',  ( 0.2768435750659113959, 0.3568721902840756854, -0.8921882507333144252 ) ) ;
#24428 = CARTESIAN_POINT ( 'NONE',  ( 124.7655881442452852, 0.5811942927096110934, -14.16772938898807510 ) ) ;
#24430 = CARTESIAN_POINT ( 'NONE',  ( 122.8368814775786291, -7.894159318335828068, -9.358103419637847864 ) ) ;
#24429 = CARTESIAN_POINT ( 'NONE',  ( 120.0572748109119772, -3.383040157471821630, -19.15922257007629170 ) ) ;
#24431 = CARTESIAN_POINT ( 'NONE',  ( 121.1350814775786233, -9.859900752359378018, -12.68260735090039759 ) ) ;
#24432 =( BOUNDED_SURFACE ( )  B_SPLINE_SURFACE ( 3, 2, ( 
 ( #11184, #31912, #43085 ),
 ( #677, #32137, #905 ),
 ( #14825, #28736, #42640 ),
 ( #32797, #11409, #42864 ),
 ( #7975, #21883, #4547 ),
 ( #18474, #15047, #11624 ) ),
 .UNSPECIFIED., .F., .F., .F. ) 
 B_SPLINE_SURFACE_WITH_KNOTS ( ( 4, 2, 4 ),
 ( 3, 3 ),
 ( 4.712388980384689674, 5.119002572906850013, 5.525616165429000581 ),
 ( 0.000000000000000000, 1.000000000000000000 ),
 .UNSPECIFIED. ) 
 GEOMETRIC_REPRESENTATION_ITEM ( )  RATIONAL_B_SPLINE_SURFACE ( (
 ( 1.000000000000000000, 0.7071067811865480168, 1.000000000000000000),
 ( 1.000000000000000000, 0.6811935452788959733, 1.000000000000000000),
 ( 1.000000000000000000, 0.6537392461962540091, 1.000000000000000000),
 ( 1.000000000000000000, 0.5999941409395589398, 1.000000000000000000),
 ( 1.000000000000000000, 0.5737032816804560342, 1.000000000000000000),
 ( 1.000000000000000000, 0.5507978985089549973, 1.000000000000000000) ) ) 
 REPRESENTATION_ITEM ( '' )  SURFACE ( )  );
#24433 = DIRECTION ( 'NONE',  ( 0.000000000000000000, 1.000000000000000000, 0.000000000000000000 ) ) ;
#24434 = CARTESIAN_POINT ( 'NONE',  ( 115.9162281442453235, -4.089484607189486809, -7.948022111789456723 ) ) ;
#24435 = EDGE_CURVE ( 'NONE', #16272, #816, #13826, .T. ) ;
#24436 = ORIENTED_EDGE ( 'NONE', *, *, #19165, .T. ) ;
#24437 = CARTESIAN_POINT ( 'NONE',  ( 125.4924948109119924, -4.159894987976798575, -8.443039665293765594 ) ) ;
#24438 = CARTESIAN_POINT ( 'NONE',  ( 108.2600671295247992, -10.62599879583958540, -13.39321520033831447 ) ) ;
#24439 = CARTESIAN_POINT ( 'NONE',  ( 106.8710046295248759, -4.863998795839590272, -18.39754474579285315 ) ) ;
#24440 = CARTESIAN_POINT ( 'NONE',  ( 108.4684265045247997, -7.250697342233347165, -19.15521520033831138 ) ) ;
#24441 = CARTESIAN_POINT ( 'NONE',  ( 124.9819548109120291, -7.618532446444632455, -18.05174138884769874 ) ) ;
#24442 = CARTESIAN_POINT ( 'NONE',  ( 111.9453614775786434, -1.561330072975668060, -17.79121239304076596 ) ) ;
#24443 = ORIENTED_EDGE ( 'NONE', *, *, #22496, .F. ) ;
#24444 = CARTESIAN_POINT ( 'NONE',  ( 112.6260814775786514, -0.8288870151387760510, -10.36305467784173118 ) ) ;
#24445 = CARTESIAN_POINT ( 'NONE',  ( 110.6214733795247867, -8.938348069036489818, -17.46756447353520159 ) ) ;
#24446 = DIRECTION ( 'NONE',  ( 0.000000000000000000, -0.3818493186865927203, 0.9242245927363029745 ) ) ;
#24447 = CARTESIAN_POINT ( 'NONE',  ( 122.6099748109119929, -9.261995988541697145, -16.69588392320189030 ) ) ;
#24448 = CARTESIAN_POINT ( 'NONE',  ( 123.5176014775786228, -9.261995988541697145, -16.69588392320189030 ) ) ;
#24449 = DIRECTION ( 'NONE',  ( -0.9908103287288505534, 0.1352586133457951978, 0.000000000000000000 ) ) ;
#24450 = CARTESIAN_POINT ( 'NONE',  ( 113.4769814775786330, -10.63000616557722466, -14.87417383870573495 ) ) ;
#24451 = DIRECTION ( 'NONE',  ( 0.000000000000000000, 0.9242245927363027524, 0.3818493186865928868 ) ) ;
#24452 = CARTESIAN_POINT ( 'NONE',  ( 115.3442858795247759, -8.402594152722688392, -9.854619843455216355 ) ) ;
#24453 = VERTEX_POINT ( 'NONE', #20897 ) ;
#24454 = DIRECTION ( 'NONE',  ( 0.4225728684367169308, -0.9063289528979889820, 0.000000000000000000 ) ) ;
#24455 = CARTESIAN_POINT ( 'NONE',  ( 115.6893214775786447, -9.859900752359374465, -12.68260735090039404 ) ) ;
#24456 = CARTESIAN_POINT ( 'NONE',  ( 126.0703014775786102, -0.1624402480850797581, -16.17319339645315424 ) ) ;
#24457 = CARTESIAN_POINT ( 'NONE',  ( 113.7468640045248236, -10.62599879583958717, -11.00651665394454604 ) ) ;
#24458 = CARTESIAN_POINT ( 'NONE',  ( 108.1906140045248463, 0.1403307496149616695, -15.46607636864997204 ) ) ;
#24459 = CARTESIAN_POINT ( 'NONE',  ( 121.9859814775786333, -9.565557343593413364, -10.61323700422348004 ) ) ;
#24460 = CARTESIAN_POINT ( 'NONE',  ( 119.4900081442453086, -7.643976991954077427, -18.09477374809248928 ) ) ;
#24461 = CARTESIAN_POINT ( 'NONE',  ( 125.7866681442452688, -0.4660016031367893996, -10.09054647747474043 ) ) ;
#24462 = ORIENTED_EDGE ( 'NONE', *, *, #3633, .F. ) ;
#24463 = ADVANCED_FACE ( 'NONE', ( #35218, #31588 ), #3338, .T. ) ;
#24464 = CARTESIAN_POINT ( 'NONE',  ( 125.0492214775786266, -3.505236298600246325, -18.68346056562440793 ) ) ;
#24465 = CIRCLE ( 'NONE', #10634, 5.000000000000002665 ) ;
#24466 = CARTESIAN_POINT ( 'NONE',  ( 125.4463081442452932, -4.153390946401325223, -8.397313243818185668 ) ) ;
#24467 = CARTESIAN_POINT ( 'NONE',  ( 113.9307948109119764, -10.15424416112533912, -14.75197769757731336 ) ) ;
#24468 = EDGE_LOOP ( 'NONE', ( #28737, #683, #42532, #25712 ) ) ;
#24469 = CARTESIAN_POINT ( 'NONE',  ( 69.69189222815028018, -41.76310523276638520, -19.39321520033831447 ) ) ;
#24470 = EDGE_CURVE ( 'NONE', #13199, #39770, #40095, .T. ) ;
#24471 = EDGE_CURVE ( 'NONE', #40625, #21740, #42093, .T. ) ;
#24472 = CARTESIAN_POINT ( 'NONE',  ( 109.1629577545248395, -2.791137627527939813, -18.39754474579286025 ) ) ;
#24473 = EDGE_LOOP ( 'NONE', ( #5795, #373, #35286, #10580 ) ) ;
#24474 = CARTESIAN_POINT ( 'NONE',  ( 117.1074881442453233, 0.4262465694468514643, -12.03445270309931736 ) ) ;
#24475 = CARTESIAN_POINT ( 'NONE',  ( 113.4202548109119846, 0.1319031606808879209, -14.10382304977623669 ) ) ;
#24476 = CARTESIAN_POINT ( 'NONE',  ( 143.3676850761856940, -69.76310523276724496, -16.89321520033831447 ) ) ;
#24477 = CONICAL_SURFACE ( 'NONE', #5557, 2.000000000000000444, 0.9599310885968830309 ) ;
#24478 = CARTESIAN_POINT ( 'NONE',  ( 75.63675420052337017, -42.57465691284114939, -19.39321520033831447 ) ) ;
#24479 = ORIENTED_EDGE ( 'NONE', *, *, #2876, .T. ) ;
#24480 = ADVANCED_FACE ( 'NONE', ( #24537 ), #20049, .T. ) ;
#24481 = CARTESIAN_POINT ( 'NONE',  ( 112.1599289911621327, -8.918981166868261923, -16.37818325645714168 ) ) ;
#24482 = CARTESIAN_POINT ( 'NONE',  ( 124.9801526047678664, -2.353188836694182218, -6.221245728286003640 ) ) ;
#24483 = CARTESIAN_POINT ( 'NONE',  ( 106.7320983795247855, -8.402594152722688392, -16.93181055722141792 ) ) ;
#24484 = AXIS2_PLACEMENT_3D ( 'NONE', #29025, #26275, #22623 ) ;
#24485 = CARTESIAN_POINT ( 'NONE',  ( 113.1933481442453058, -4.089484607189486809, -7.948022111789456723 ) ) ;
#24486 = EDGE_CURVE ( 'NONE', #26292, #17071, #21862, .T. ) ;
#24487 = CARTESIAN_POINT ( 'NONE',  ( 122.0427081442452817, -9.859900752359378018, -12.68260735090039759 ) ) ;
#24488 = CARTESIAN_POINT ( 'NONE',  ( 116.1998614775786507, 0.4262465694468514643, -12.03445270309931736 ) ) ;
#24489 = CARTESIAN_POINT ( 'NONE',  ( 113.9875214775786532, -8.899110576539717599, -16.42337572283489067 ) ) ;
#24490 = EDGE_CURVE ( 'NONE', #6307, #12500, #26506, .T. ) ;
#24491 = ADVANCED_FACE ( 'NONE', ( #19653 ), #8951, .T. ) ;
#24492 = ORIENTED_EDGE ( 'NONE', *, *, #27807, .F. ) ;
#24493 = CARTESIAN_POINT ( 'NONE',  ( 116.7341483858831737, -6.008534230275574650, -18.41440645892366490 ) ) ;
#24494 = CARTESIAN_POINT ( 'NONE',  ( 117.5613014775786525, -10.15424416112533912, -14.75197769757731336 ) ) ;
#24495 = CARTESIAN_POINT ( 'NONE',  ( 125.2194014775786286, 0.1319031606808879209, -14.10382304977623669 ) ) ;
#24496 = DIRECTION ( 'NONE',  ( 1.000000000000000000, 0.000000000000000000, 0.000000000000000000 ) ) ;
#24497 = DIRECTION ( 'NONE',  ( 1.000000000000000000, 0.000000000000000000, -0.000000000000000000 ) ) ;
#24498 = CIRCLE ( 'NONE', #25961, 2.999999999999999556 ) ;
#24499 = CARTESIAN_POINT ( 'NONE',  ( 116.0296814775786345, -8.166667518702817929, -8.995218007635861213 ) ) ;
#24500 = VERTEX_POINT ( 'NONE', #40415 ) ;
#24501 = CARTESIAN_POINT ( 'NONE',  ( 113.1366214775786432, -1.834011780172310813, -8.268836392978581529 ) ) ;
#24502 = CARTESIAN_POINT ( 'NONE',  ( 70.19189222814998175, -52.04917782255280656, -34.02249884819201498 ) ) ;
#24503 = CARTESIAN_POINT ( 'NONE',  ( 111.0381921295247878, 0.8980012041604618078, -13.39321520033831447 ) ) ;
#24504 = CARTESIAN_POINT ( 'NONE',  ( 126.1270281442452870, 0.1319031606808879209, -14.10382304977623669 ) ) ;
#24505 = CARTESIAN_POINT ( 'NONE',  ( 112.2857214775786474, -4.089484607189486809, -7.948022111789456723 ) ) ;
#24506 = CARTESIAN_POINT ( 'NONE',  ( 122.3263414775786373, -3.505236298600246325, -18.68346056562440793 ) ) ;
#24507 = DIRECTION ( 'NONE',  ( 1.000000000000000000, 0.000000000000000000, -0.000000000000000000 ) ) ;
#24508 = CARTESIAN_POINT ( 'NONE',  ( 111.6632702545248605, 0.1403307496149616695, -11.32035403202665336 ) ) ;
#24509 = AXIS2_PLACEMENT_3D ( 'NONE', #37547, #13173, #20687 ) ;
#24510 = FACE_OUTER_BOUND ( 'NONE', #5956, .T. ) ;
#24511 = CARTESIAN_POINT ( 'NONE',  ( 109.2294418913466103, -8.121613810544367595, -17.63527159796440813 ) ) ;
#24512 = CARTESIAN_POINT ( 'NONE',  ( 118.4122014775786340, -9.859900752359374465, -12.68260735090039404 ) ) ;
#24513 = CARTESIAN_POINT ( 'NONE',  ( 107.2877233795247776, -8.938348069036489818, -17.46756447353520159 ) ) ;
#24514 = CARTESIAN_POINT ( 'NONE',  ( 122.8560864091100768, -0.9924539043446216624, -17.29976612834909133 ) ) ;
#24515 = CARTESIAN_POINT ( 'NONE',  ( 107.7738952545248310, 0.8980012041604421569, -11.00651665394454071 ) ) ;
#24516 = CARTESIAN_POINT ( 'NONE',  ( 91.23658249893594530, -5.844616714554617509, -18.64321520033831803 ) ) ;
#24517 = CARTESIAN_POINT ( 'NONE',  ( 124.4252281442452812, -9.261995988541697145, -16.69588392320189030 ) ) ;
#24518 = CARTESIAN_POINT ( 'NONE',  ( 120.0947965460471920, -2.191907684172563986, -18.20049396185734025 ) ) ;
#24519 = CARTESIAN_POINT ( 'NONE',  ( 119.6034614775786196, -6.344957434206665248, -7.627207830600338134 ) ) ;
#24520 = CARTESIAN_POINT ( 'NONE',  ( 115.5191414775786569, -3.383040157471821630, -19.15922257007629170 ) ) ;
#24521 = EDGE_LOOP ( 'NONE', ( #23865, #40365, #31411, #8974 ) ) ;
#24522 = AXIS2_PLACEMENT_3D ( 'NONE', #35732, #41705, #24372 ) ;
#24523 = CARTESIAN_POINT ( 'NONE',  ( 116.3700414775786527, -4.153390946401321671, -8.397313243818183892 ) ) ;
#24524 = CARTESIAN_POINT ( 'NONE',  ( 122.7234281442452755, -5.638512984488999180, -18.83840828888717311 ) ) ;
#24525 = CARTESIAN_POINT ( 'NONE',  ( 118.8660148109119774, -10.30919188438810075, -12.61870101168855918 ) ) ;
#24526 =( BOUNDED_SURFACE ( )  B_SPLINE_SURFACE ( 1, 2, ( 
 ( #18749, #18968, #32856, #5281, #12136, #19199, #33076, #36730, #2762, #5722, #2305, #30361, #16459, #30809, #37418, #20331, #33764, #5496, #16687, #41091, #13038, #44285, #26495, #33993, #30580, #12364, #2532, #40400, #9163, #23758, #44501, #13264, #16235, #27170, #9849, #26937, #33303, #20107, #34216, #37648, #26717, #40860, #26264, #43825, #40626, #9383, #9613, #23293, #2989, #12591, #16915, #23532, #6422, #37178, #30138, #44052, #40171, #8935, #2079, #5951, #12817, #22837, #19875, #6187, #23067 ),
 ( #36951, #19417, #16003, #29911, #19640, #33526, #31026, #35949, #18419, #11346, #18638, #31246, #41535, #3439, #25483, #42813, #38090, #10078, #11575, #14769, #34434, #14989, #34654, #39387, #25258, #42585, #18184, #39155, #23980, #7920, #17358, #6645, #8153, #4496, #28903, #847, #4265, #13714, #21829, #32311, #44733, #21605, #27621, #10296, #22057, #35723, #1077, #18, #4721, #13492, #28682, #20553, #27397, #41319, #37867, #13931, #35493, #3213, #44957, #27840, #41753, #32079, #10513, #17139, #24199 ) ),
 .UNSPECIFIED., .F., .F., .T. ) 
 B_SPLINE_SURFACE_WITH_KNOTS ( ( 2, 2 ),
 ( 3, 2, 2, 2, 2, 2, 2, 2, 2, 2, 2, 2, 2, 2, 2, 2, 2, 2, 2, 2, 2, 2, 2, 2, 2, 2, 2, 2, 2, 2, 2, 2, 3 ),
 ( 0.000000000000000000, 1.000000000000000000 ),
 ( 0.000000000000000000, 0.03125000000000000000, 0.06250000000000000000, 0.09375000000000000000, 0.1250000000000000000, 0.1562500000000000000, 0.1875000000000000000, 0.2187500000000000000, 0.2500000000000000000, 0.2812500000000000000, 0.3125000000000000000, 0.3437500000000000000, 0.3750000000000000000, 0.4062500000000000000, 0.4375000000000000000, 0.4687500000000000000, 0.5000000000000000000, 0.5312500000000000000, 0.5625000000000000000, 0.5937500000000000000, 0.6250000000000000000, 0.6562500000000000000, 0.6875000000000000000, 0.7187500000000000000, 0.7500000000000000000, 0.7812500000000000000, 0.8125000000000000000, 0.8437500000000000000, 0.8750000000000000000, 0.9062500000000000000, 0.9375000000000000000, 0.9687500000000000000, 1.000000000000000000 ),
 .UNSPECIFIED. ) 
 GEOMETRIC_REPRESENTATION_ITEM ( )  RATIONAL_B_SPLINE_SURFACE ( (
 ( 1.000000000000000000, 0.9238795325112869605, 1.000000000000000000, 0.9238795325112869605, 1.000000000000000000, 0.9238795325112869605, 1.000000000000000000, 0.9238795325112869605, 1.000000000000000000, 0.9238795325112869605, 1.000000000000000000, 0.9238795325112869605, 1.000000000000000000, 0.9238795325112869605, 1.000000000000000000, 0.9238795325112869605, 1.000000000000000000, 0.9238795325112869605, 1.000000000000000000, 0.9238795325112869605, 1.000000000000000000, 0.9238795325112869605, 1.000000000000000000, 0.9238795325112869605, 1.000000000000000000, 0.9238795325112869605, 1.000000000000000000, 0.9238795325112869605, 1.000000000000000000, 0.9238795325112869605, 1.000000000000000000, 0.9238795325112869605, 1.000000000000000000, 0.9238795325112869605, 1.000000000000000000, 0.9238795325112869605, 1.000000000000000000, 0.9238795325112869605, 1.000000000000000000, 0.9238795325112869605, 1.000000000000000000, 0.9238795325112869605, 1.000000000000000000, 0.9238795325112869605, 1.000000000000000000, 0.9238795325112869605, 1.000000000000000000, 0.9238795325112869605, 1.000000000000000000, 0.9238795325112869605, 1.000000000000000000, 0.9238795325112869605, 1.000000000000000000, 0.9238795325112869605, 1.000000000000000000, 0.9238795325112869605, 1.000000000000000000, 0.9238795325112869605, 1.000000000000000000, 0.9238795325112869605, 1.000000000000000000, 0.9238795325112869605, 1.000000000000000000, 0.9238795325112869605, 1.000000000000000000),
 ( 1.000000000000000000, 0.9238795325112869605, 1.000000000000000000, 0.9238795325112869605, 1.000000000000000000, 0.9238795325112869605, 1.000000000000000000, 0.9238795325112869605, 1.000000000000000000, 0.9238795325112869605, 1.000000000000000000, 0.9238795325112869605, 1.000000000000000000, 0.9238795325112869605, 1.000000000000000000, 0.9238795325112869605, 1.000000000000000000, 0.9238795325112869605, 1.000000000000000000, 0.9238795325112869605, 1.000000000000000000, 0.9238795325112869605, 1.000000000000000000, 0.9238795325112869605, 1.000000000000000000, 0.9238795325112869605, 1.000000000000000000, 0.9238795325112869605, 1.000000000000000000, 0.9238795325112869605, 1.000000000000000000, 0.9238795325112869605, 1.000000000000000000, 0.9238795325112869605, 1.000000000000000000, 0.9238795325112869605, 1.000000000000000000, 0.9238795325112869605, 1.000000000000000000, 0.9238795325112869605, 1.000000000000000000, 0.9238795325112869605, 1.000000000000000000, 0.9238795325112869605, 1.000000000000000000, 0.9238795325112869605, 1.000000000000000000, 0.9238795325112869605, 1.000000000000000000, 0.9238795325112869605, 1.000000000000000000, 0.9238795325112869605, 1.000000000000000000, 0.9238795325112869605, 1.000000000000000000, 0.9238795325112869605, 1.000000000000000000, 0.9238795325112869605, 1.000000000000000000, 0.9238795325112869605, 1.000000000000000000, 0.9238795325112869605, 1.000000000000000000, 0.9238795325112869605, 1.000000000000000000) ) ) 
 REPRESENTATION_ITEM ( '' )  SURFACE ( )  );
#24527 = CARTESIAN_POINT ( 'NONE',  ( 115.8595014775786609, -7.643976991954077427, -18.09477374809248928 ) ) ;
#24528 = ORIENTED_EDGE ( 'NONE', *, *, #2187, .F. ) ;
#24529 = CARTESIAN_POINT ( 'NONE',  ( 121.6456214775786293, 0.4262465694468514643, -12.03445270309931736 ) ) ;
#24530 = EDGE_CURVE ( 'NONE', #41036, #30859, #2950, .T. ) ;
#24531 = CARTESIAN_POINT ( 'NONE',  ( 117.2776681442452968, -5.638512984488999180, -18.83840828888717311 ) ) ;
#24532 = CARTESIAN_POINT ( 'NONE',  ( 136.2190063926907726, 0.5346461494345294829, -15.66526563388532090 ) ) ;
#24533 = CARTESIAN_POINT ( 'NONE',  ( 112.3578015045248861, -2.477300249445798297, -7.631215200338321125 ) ) ;
#24534 = CARTESIAN_POINT ( 'NONE',  ( 67.93084693336861335, 0.8442783687841282081, -9.853887653298288640 ) ) ;
#24535 = CARTESIAN_POINT ( 'NONE',  ( 124.8790414775786246, -0.4660016031367893996, -10.09054647747474043 ) ) ;
#24536 = CIRCLE ( 'NONE', #31078, 20.00000000000000355 ) ;
#24537 = FACE_OUTER_BOUND ( 'NONE', #28121, .T. ) ;
#24538 = CARTESIAN_POINT ( 'NONE',  ( 115.1220548109119761, -8.166667518702817929, -8.995218007635861213 ) ) ;
#24539 = CARTESIAN_POINT ( 'NONE',  ( 135.3184548109119874, -10.81584935473217080, -14.15181583611863303 ) ) ;
#24540 = CARTESIAN_POINT ( 'NONE',  ( 113.3635281442453504, -0.1624402480850797581, -16.17319339645315424 ) ) ;
#24541 = CARTESIAN_POINT ( 'NONE',  ( 60.94960279574944195, -12.50265280191595529, -17.24776159451941382 ) ) ;
#24542 = EDGE_CURVE ( 'NONE', #37423, #36514, #13866, .T. ) ;
#24543 = CARTESIAN_POINT ( 'NONE',  ( 115.5167787682627960, -1.040089454026966287, -17.23633227186632766 ) ) ;
#24544 = CARTESIAN_POINT ( 'NONE',  ( 117.0111608795247946, -1.325403438956436419, -16.93181055722141792 ) ) ;
#24545 = CONICAL_SURFACE ( 'NONE', #7815, 1.610000000000000986, 0.9599310885968765916 ) ;
#24546 = CARTESIAN_POINT ( 'NONE',  ( 117.5045748109119756, 0.5811942927096110934, -14.16772938898807510 ) ) ;
#24547 = DIRECTION ( 'NONE',  ( 0.9908103287288504424, -0.1352586133457950590, 0.000000000000000000 ) ) ;
#24548 = DIRECTION ( 'NONE',  ( -0.2407039305251457151, 0.3604685577742790525, -0.9011792478113758165 ) ) ;
#24549 = DIRECTION ( 'NONE',  ( -0.000000000000000000, -0.9284778069183721172, -0.3713878862591650232 ) ) ;
#24550 = CARTESIAN_POINT ( 'NONE',  ( 124.2550481442452792, -0.1624402480850797581, -16.17319339645315424 ) ) ;
#24551 = CARTESIAN_POINT ( 'NONE',  ( 117.8449348109119938, -1.833838273342659253, -17.42832698103878286 ) ) ;
#24552 = ORIENTED_EDGE ( 'NONE', *, *, #42051, .F. ) ;
#24553 = CARTESIAN_POINT ( 'NONE',  ( 136.2267163767933766, -9.456939161313274056, -9.757884007028398088 ) ) ;
#24554 = EDGE_CURVE ( 'NONE', #30137, #37005, #8772, .T. ) ;
#24555 = CARTESIAN_POINT ( 'NONE',  ( 123.6310548109119765, -5.638512984488999180, -18.83840828888717311 ) ) ;
#24556 = CARTESIAN_POINT ( 'NONE',  ( 115.0664733795247798, -1.325403438956436419, -9.854619843455211026 ) ) ;
#24557 = CARTESIAN_POINT ( 'NONE',  ( 116.8238548109119819, -5.574606645277164318, -18.38911715685844683 ) ) ;
#24558 = CARTESIAN_POINT ( 'NONE',  ( 113.9307948109119764, -10.15424416112533912, -14.75197769757731336 ) ) ;
#24559 = CARTESIAN_POINT ( 'NONE',  ( 86.21536009029834702, -26.71263513348336360, -8.458135821852174274 ) ) ;
#24560 = CARTESIAN_POINT ( 'NONE',  ( 114.5803015045248117, -2.477300249445798297, -7.631215200338321125 ) ) ;
#24561 = CARTESIAN_POINT ( 'NONE',  ( 120.5678148109119832, -1.833838273342659253, -17.42832698103878286 ) ) ;
#24562 = CARTESIAN_POINT ( 'NONE',  ( 119.3198281442452924, -9.859900752359374465, -12.68260735090039404 ) ) ;
#24563 = CARTESIAN_POINT ( 'NONE',  ( 138.2184548109119930, -4.863998795839242995, -13.39321520033831447 ) ) ;
#24564 = CARTESIAN_POINT ( 'NONE',  ( 109.2294415350724393, -1.058881497505862690, -9.579285122087750182 ) ) ;
#24565 = CARTESIAN_POINT ( 'NONE',  ( 121.5492360609119800, -6.564341423271550902, -7.887810678476487425 ) ) ;
#24566 = TOROIDAL_SURFACE ( 'NONE', #3435, 4.500000000000000000, 0.5000000000000000000 ) ;
#24567 = CARTESIAN_POINT ( 'NONE',  ( 109.9963952545248134, -9.868328341294098749, -15.46607636864997204 ) ) ;
#24568 = CARTESIAN_POINT ( 'NONE',  ( 117.1877300385866789, 1.365262974659312123, -21.54737627516459142 ) ) ;
#24569 = CARTESIAN_POINT ( 'NONE',  ( 117.2209414775786485, -7.893985811506177619, -18.51759400769804742 ) ) ;
#24570 = CARTESIAN_POINT ( 'NONE',  ( 114.0442481442453300, -1.834011780172310813, -8.268836392978581529 ) ) ;
#24571 = CARTESIAN_POINT ( 'NONE',  ( 111.7327233795247849, -8.938348069036489818, -17.46756447353520159 ) ) ;
#24572 = CARTESIAN_POINT ( 'NONE',  ( 122.4521266859119635, -9.033780868592240054, -16.85052413769862056 ) ) ;
#24573 = ORIENTED_EDGE ( 'NONE', *, *, #21430, .F. ) ;
#24574 = DIRECTION ( 'NONE',  ( 0.9609149988134839671, -0.1028163501681660097, 0.2570431154366504822 ) ) ;
#24575 = CARTESIAN_POINT ( 'NONE',  ( 121.3052614775786111, -1.834011780172310813, -8.268836392978581529 ) ) ;
#24576 = CARTESIAN_POINT ( 'NONE',  ( 126.5241148109119393, -9.565557343593413364, -10.61323700422348004 ) ) ;
#24577 = CARTESIAN_POINT ( 'NONE',  ( 123.3474214775786209, -0.1624402480850797581, -16.17319339645315424 ) ) ;
#24578 = CARTESIAN_POINT ( 'NONE',  ( 126.0703014775786102, -9.988377603198980381, -10.36322818467138518 ) ) ;
#24579 = CARTESIAN_POINT ( 'NONE',  ( 116.4834948109119779, -1.561330072975668504, -17.79121239304076951 ) ) ;
#24580 = CIRCLE ( 'NONE', #36215, 0.8999999999999980238 ) ;
#24581 = CARTESIAN_POINT ( 'NONE',  ( 107.9822546295247889, -4.863998795839590272, -18.39754474579285315 ) ) ;
#24582 = CARTESIAN_POINT ( 'NONE',  ( 117.2209414775786485, -2.084020599724406786, -8.691656652584148546 ) ) ;
#24583 = FACE_BOUND ( 'NONE', #26117, .T. ) ;
#24584 = VERTEX_POINT ( 'NONE', #17370 ) ;
#24585 = CARTESIAN_POINT ( 'NONE',  ( 121.4187148109119789, -6.344957434206665248, -7.627207830600338134 ) ) ;
#24586 = ADVANCED_FACE ( 'NONE', ( #31259 ), #10091, .T. ) ;
#24587 = CARTESIAN_POINT ( 'NONE',  ( 81.52050388106540879, 0.5255923868638483487, -16.39321520033831447 ) ) ;
#24588 = CARTESIAN_POINT ( 'NONE',  ( 117.3911214775786505, -1.561330072975668504, -17.79121239304076951 ) ) ;
#24589 = ORIENTED_EDGE ( 'NONE', *, *, #5785, .T. ) ;
#24590 = CARTESIAN_POINT ( 'NONE',  ( 106.8015515045248378, -6.936859964151250502, -18.39754474579286025 ) ) ;
#24591 = CARTESIAN_POINT ( 'NONE',  ( 125.8433948109119456, -1.834011780172310813, -8.268836392978581529 ) ) ;
#24593 = DIRECTION ( 'NONE',  ( 0.000000000000000000, -0.3818493186865936084, 0.9242245927363024194 ) ) ;
#24592 = AXIS2_PLACEMENT_3D ( 'NONE', #41151, #9912, #38366 ) ;
#24594 = CARTESIAN_POINT ( 'NONE',  ( 115.9162281442453235, -5.574606645277164318, -18.38911715685844683 ) ) ;
#24595 = CARTESIAN_POINT ( 'NONE',  ( 83.82415148905927538, -46.76310523276723785, -4.893215200338314474 ) ) ;
#24596 = CARTESIAN_POINT ( 'NONE',  ( 120.0005481442453146, -4.153390946401325223, -8.397313243818185668 ) ) ;
#24597 = CARTESIAN_POINT ( 'NONE',  ( 85.04324155394569118, -25.99489077589524300, -13.39321520033831447 ) ) ;
#24598 = CARTESIAN_POINT ( 'NONE',  ( 119.8303681442453126, 0.4262465694468514643, -12.03445270309931736 ) ) ;
#24599 = EDGE_CURVE ( 'NONE', #23245, #39765, #20787, .T. ) ;
#24600 = CARTESIAN_POINT ( 'NONE',  ( 116.8928740015602870, 0.2848729546123598966, -14.64321520033831447 ) ) ;
#24601 = CARTESIAN_POINT ( 'NONE',  ( 117.6180281442453150, -8.899110576539710493, -16.42337572283490132 ) ) ;
#24602 = CARTESIAN_POINT ( 'NONE',  ( 122.3826735609119680, 0.6414057260225851653, -11.69287257290600657 ) ) ;
#24603 = CARTESIAN_POINT ( 'NONE',  ( 117.6180281442453150, -0.4660016031367893996, -10.09054647747474043 ) ) ;
#24604 = CARTESIAN_POINT ( 'NONE',  ( 138.2184548109119930, 0.6402711692277546218, -15.78131322003127579 ) ) ;
#24605 = CARTESIAN_POINT ( 'NONE',  ( 120.1707281442453166, -9.565557343593413364, -10.61323700422348004 ) ) ;
#24606 = ORIENTED_EDGE ( 'NONE', *, *, #41775, .F. ) ;
#24607 = CARTESIAN_POINT ( 'NONE',  ( 115.5758681442453053, -1.561330072975668060, -17.79121239304076951 ) ) ;
#24608 = CARTESIAN_POINT ( 'NONE',  ( 108.3295202545248657, -10.62599879583958717, -15.77991374673208469 ) ) ;
#24609 = DIRECTION ( 'NONE',  ( 0.9908103287288504424, -0.1352586133457950313, 0.000000000000000000 ) ) ;
#24610 = DIRECTION ( 'NONE',  ( -1.000000000000000000, 0.000000000000000000, 0.000000000000000000 ) ) ;
#24611 = CARTESIAN_POINT ( 'NONE',  ( 113.3470697905468825, 0.6938714319018670640, -12.14321520033833579 ) ) ;
#24612 = CARTESIAN_POINT ( 'NONE',  ( 124.1983214775786166, -8.166667518702819706, -8.995218007635861213 ) ) ;
#24613 = ORIENTED_EDGE ( 'NONE', *, *, #3931, .T. ) ;
#24614 = DIRECTION ( 'NONE',  ( 0.000000000000000000, -0.3713878862591641905, 0.9284778069183722282 ) ) ;
#24615 = CARTESIAN_POINT ( 'NONE',  ( 117.2776681442452968, -4.153390946401321671, -8.397313243818183892 ) ) ;
#24616 = CARTESIAN_POINT ( 'NONE',  ( 116.4160804811916989, -3.807985514183284348, -19.09877912889400520 ) ) ;
#24617 = CARTESIAN_POINT ( 'NONE',  ( 66.21635238248168775, -14.64006919827764364, -16.51222081763639338 ) ) ;
#24618 = CARTESIAN_POINT ( 'NONE',  ( 89.40092984481313465, -26.60966817898065884, -11.90521360603286816 ) ) ;
#24619 = CARTESIAN_POINT ( 'NONE',  ( 112.2188952545247531, -9.868328341294098749, -15.46607636864997204 ) ) ;
#24620 = CARTESIAN_POINT ( 'NONE',  ( 89.25811708600326710, -10.04048109355869300, -13.74760083314252768 ) ) ;
#24621 = ORIENTED_EDGE ( 'NONE', *, *, #10263, .T. ) ;
#24622 = CARTESIAN_POINT ( 'NONE',  ( 116.0296814775786345, -8.166667518702817929, -8.995218007635861213 ) ) ;
#24623 = CARTESIAN_POINT ( 'NONE',  ( 124.7655881442452852, -9.859900752359378018, -12.68260735090039759 ) ) ;
#24624 = CARTESIAN_POINT ( 'NONE',  ( 124.7655881442452852, 0.5811942927096110934, -14.16772938898807510 ) ) ;
#24625 = CARTESIAN_POINT ( 'NONE',  ( 116.1431348109119881, 0.1319031606808879209, -14.10382304977623669 ) ) ;
#24626 = CARTESIAN_POINT ( 'NONE',  ( 109.2294421295247844, 0.8460904216231607267, -19.39321520033831447 ) ) ;
#24627 = CARTESIAN_POINT ( 'NONE',  ( 61.43583762032555029, 4.505738898882963639, -14.64321520033831447 ) ) ;
#24628 = CARTESIAN_POINT ( 'NONE',  ( 120.1707281442453166, 0.2603800115204892296, -16.42320221600525088 ) ) ;
#24629 = DIRECTION ( 'NONE',  ( -0.9908103287288511085, 0.1352586133457904793, 0.000000000000000000 ) ) ;
#24630 = CARTESIAN_POINT ( 'NONE',  ( 61.63318325272354770, -19.46990085680238636, -15.89321520033831447 ) ) ;
#24631 = LINE ( 'NONE', #35313, #14264 ) ;
#24632 = CARTESIAN_POINT ( 'NONE',  ( 121.7590748109119687, -2.084020599724406786, -8.691656652584148546 ) ) ;
#24633 = ORIENTED_EDGE ( 'NONE', *, *, #2994, .F. ) ;
#24634 = CARTESIAN_POINT ( 'NONE',  ( 116.5982304348999889, -9.866848165334292986, -13.49403011250934625 ) ) ;
#24635 = CARTESIAN_POINT ( 'NONE',  ( 118.2420214775786320, -3.383040157471821630, -19.15922257007629170 ) ) ;
#24636 = CARTESIAN_POINT ( 'NONE',  ( 124.8223148109119762, -10.15424416112533912, -14.75197769757731336 ) ) ;
#24637 = ORIENTED_EDGE ( 'NONE', *, *, #12793, .F. ) ;
#24638 = CARTESIAN_POINT ( 'NONE',  ( 112.3424481442453384, -6.344957434206662583, -7.627207830600332805 ) ) ;
#24639 = CARTESIAN_POINT ( 'NONE',  ( 123.4041481442452834, -10.30919188438810075, -12.61870101168855918 ) ) ;
#24640 = CARTESIAN_POINT ( 'NONE',  ( 107.2182702545248105, -10.62599879583958717, -15.77991374673208469 ) ) ;
#24641 = CARTESIAN_POINT ( 'NONE',  ( 119.2631014775786298, -9.565557343593413364, -10.61323700422348004 ) ) ;
#24642 = EDGE_LOOP ( 'NONE', ( #41940, #25623, #19125, #20970 ) ) ;
#24643 = ORIENTED_EDGE ( 'NONE', *, *, #25029, .F. ) ;
#24644 = CARTESIAN_POINT ( 'NONE',  ( 115.9729548109119861, -6.344957434206662583, -7.627207830600332805 ) ) ;
#24645 = CARTESIAN_POINT ( 'NONE',  ( 125.1626748109119802, -0.1624402480850797581, -16.17319339645315424 ) ) ;
#24646 = CARTESIAN_POINT ( 'NONE',  ( 79.25282380889900935, 4.987561187848681854, -20.71017453681549725 ) ) ;
#24647 = CARTESIAN_POINT ( 'NONE',  ( 124.3685014775786328, -10.63000616557722466, -14.87417383870573495 ) ) ;
#24648 = CARTESIAN_POINT ( 'NONE',  ( 122.9728284624957553, -6.270977643812233104, -18.77740645536396258 ) ) ;
#24649 = ADVANCED_FACE ( 'NONE', ( #3667 ), #16811, .F. ) ;
#24650 = DIRECTION ( 'NONE',  ( -1.000000000000000000, 1.156482317317869950E-15, 0.000000000000000000 ) ) ;
#24651 = CARTESIAN_POINT ( 'NONE',  ( 122.5532481442453019, -10.63000616557722466, -14.87417383870573495 ) ) ;
#24653 = CARTESIAN_POINT ( 'NONE',  ( 121.9292548109119849, -7.894159318335828068, -9.358103419637847864 ) ) ;
#24652 = CARTESIAN_POINT ( 'NONE',  ( 123.3474214775786209, -9.988377603198976828, -10.36322818467138340 ) ) ;
#24654 = CARTESIAN_POINT ( 'NONE',  ( 119.6034614775786196, -3.505236298600246325, -18.68346056562440793 ) ) ;
#24655 = CARTESIAN_POINT ( 'NONE',  ( 115.0086014775786509, -4.089484607189486809, -7.948022111789456723 ) ) ;
#24656 = ORIENTED_EDGE ( 'NONE', *, *, #4774, .F. ) ;
#24657 = CARTESIAN_POINT ( 'NONE',  ( 124.9357681442453156, -7.643976991953167044, -18.09477374809303285 ) ) ;
#24658 = CARTESIAN_POINT ( 'NONE',  ( 114.6497546295247929, -4.863998795839590272, -18.39754474579285315 ) ) ;
#24659 = CARTESIAN_POINT ( 'NONE',  ( 107.7044421295247929, -9.868328341294093420, -13.39321520033831447 ) ) ;
#24660 = CARTESIAN_POINT ( 'NONE',  ( 113.0523327545247838, -6.936859964151250502, -8.388885654883777576 ) ) ;
#24661 = CARTESIAN_POINT ( 'NONE',  ( 125.2088614775786510, -0.2054726073298613620, -16.14774885094370660 ) ) ;
#24662 = CARTESIAN_POINT ( 'NONE',  ( 112.1722681442453222, -0.4660016031367893996, -10.09054647747474043 ) ) ;
#24663 = ORIENTED_EDGE ( 'NONE', *, *, #22011, .F. ) ;
#24664 = CARTESIAN_POINT ( 'NONE',  ( 113.0231681442453180, -10.15424416112533912, -14.75197769757731336 ) ) ;
#24665 = CARTESIAN_POINT ( 'NONE',  ( 112.8439733795247832, -8.938348069036489818, -17.46756447353520159 ) ) ;
#24666 = CARTESIAN_POINT ( 'NONE',  ( 66.82415148905926117, -30.76310523276723785, -21.89321520033831447 ) ) ;
#24667 = CARTESIAN_POINT ( 'NONE',  ( 121.9859814775786333, 0.2603800115204892296, -16.42320221600525088 ) ) ;
#24668 = CARTESIAN_POINT ( 'NONE',  ( 125.1059481442452750, -8.166667518702819706, -8.995218007635861213 ) ) ;
#24669 = CARTESIAN_POINT ( 'NONE',  ( 60.99435512697147033, -13.32931833351155326, -19.27180043387577157 ) ) ;
#24670 = CARTESIAN_POINT ( 'NONE',  ( 114.6115148109119986, -3.383040157471821630, -19.15922257007629170 ) ) ;
#24671 = CARTESIAN_POINT ( 'NONE',  ( 112.9134265045247645, -7.250697342233347165, -19.15521520033831138 ) ) ;
#24672 = CARTESIAN_POINT ( 'NONE',  ( 106.6626452545248611, 0.8980012041604421569, -11.00651665394454071 ) ) ;
#24673 = ORIENTED_EDGE ( 'NONE', *, *, #29792, .T. ) ;
#24674 = CARTESIAN_POINT ( 'NONE',  ( 127.3434826497568935, -7.118825987476567363, -8.305226122375637843 ) ) ;
#24675 = CARTESIAN_POINT ( 'NONE',  ( 114.5547881442453217, -4.153390946401321671, -8.397313243818183892 ) ) ;
#24676 = CARTESIAN_POINT ( 'NONE',  ( 112.5693548109119888, -10.63000616557722466, -14.87417383870573495 ) ) ;
#24677 = CARTESIAN_POINT ( 'NONE',  ( 115.6220983795247861, -0.7896495226426338832, -9.318865927141430916 ) ) ;
#24678 = CARTESIAN_POINT ( 'NONE',  ( 105.4819421295248247, -9.868328341294093420, -13.39321520033831447 ) ) ;
#24679 = CARTESIAN_POINT ( 'NONE',  ( 122.3830681442452857, -1.833838273342659697, -17.42832698103878286 ) ) ;
#24680 = UNCERTAINTY_MEASURE_WITH_UNIT (LENGTH_MEASURE( 1.000000000000000082E-05 ), #30518, 'distance_accuracy_value', 'NONE');
#24681 = CARTESIAN_POINT ( 'NONE',  ( 119.6034614775786196, -3.505236298600246325, -18.68346056562440793 ) ) ;
#24682 = CARTESIAN_POINT ( 'NONE',  ( 112.3991748109119868, -1.833838273342658809, -17.42832698103878286 ) ) ;
#24683 = ORIENTED_EDGE ( 'NONE', *, *, #22336, .T. ) ;
#24684 = CARTESIAN_POINT ( 'NONE',  ( 124.5386814775786206, -4.153390946401325223, -8.397313243818185668 ) ) ;
#24685 = CARTESIAN_POINT ( 'NONE',  ( 125.6732148109119862, -9.859900752359378018, -12.68260735090039759 ) ) ;
#24686 = CARTESIAN_POINT ( 'NONE',  ( 114.2711548109119803, -0.1624402480850797581, -16.17319339645315424 ) ) ;
#24687 = ORIENTED_EDGE ( 'NONE', *, *, #11706, .T. ) ;
#24688 = DIRECTION ( 'NONE',  ( 0.000000000000000000, 0.9242245927363041957, 0.3818493186865896116 ) ) ;
#24689 = CARTESIAN_POINT ( 'NONE',  ( 106.0375671295248310, -10.62599879583958540, -13.39321520033831447 ) ) ;
#24690 = CARTESIAN_POINT ( 'NONE',  ( 112.8439733795247832, -1.325403438956436419, -9.854619843455211026 ) ) ;
#24691 = ORIENTED_EDGE ( 'NONE', *, *, #31852, .F. ) ;
#24692 = CARTESIAN_POINT ( 'NONE',  ( 119.4332814775786318, -8.899110576539710493, -16.42337572283490132 ) ) ;
#24693 = CARTESIAN_POINT ( 'NONE',  ( 114.4980614775786734, -2.084020599724406786, -8.691656652584148546 ) ) ;
#24694 =( BOUNDED_SURFACE ( )  B_SPLINE_SURFACE ( 1, 2, ( 
 ( #17011, #17230, #20203, #40955, #43915, #44600, #3084, #30902, #2624, #13582, #27492, #30227, #33855, #16557, #6512, #41410, #13134, #13363, #40496, #44149, #27038, #9710, #27268, #12914, #26810, #9479, #30452, #37741, #10166, #41181, #23622, #9942, #23855, #9257, #24073, #37966, #23166, #6742, #37277, #37046, #34528, #3306, #5817, #33621, #2397, #6044, #19967, #44372, #14245, #14694, #17889, #21308, #21532, #771, #332, #38850, #31563, #28608, #3744, #34957, #41849, #4196, #3968, #28377, #39084, #31787, #35191, #4425, #11052, #32007, #38397, #21759, #21080, #42517, #31120, #20867, #24726, #7619, #18114, #45044, #7391, #28161, #13804, #559, #35420, #11277, #17667, #25185, #7853, #3526, #42071, #10829, #35651, #27716, #38614, #14469, #41631, #17444, #42290, #24955, #10387, #31337, #112, #14025, #24296, #38183, #6960, #34745, #27939, #10609, #24512, #7169, #29717, #32679, #8303, #15818, #1448, #8081, #39757, #1669, #1005, #39981, #11953, #36321, #25851, #40212, #22876, #15144, #25638, #25411, #43189, #8527, #15592, #43408, #36100, #32893, #29050, #18789, #22429, #21983, #11507, #8978, #42742, #8745, #14921, #35872, #5091, #19007, #29495, #12176, #28831, #26077, #22652, #36548, #5322, #19238, #4643, #18341, #32234, #18565, #33121, #1889, #43630, #12404, #36770, #26304, #39311, #42958, #32456, #1231, #11725, #39542, #22205, #29273, #4872, #15369, #13309, #34262, #20375, #5995, #23336, #26533, #23114, #2806, #43864, #24024, #19918, #40443, #26983, #44326, #40903, #6466, #30179, #9204, #27216, #2346, #19458, #23577, #33341, #33569, #3037, #16959, #36991, #33803, #16504, #30404, #12861, #26762, #37459, #30853, #5761, #13084, #19682, #44776, #34037, #13535, #27442, #12636, #16276, #9657, #44097, #40671, #41364, #9423, #37221, #6231, #16732, #2575, #20153, #30629, #44545, #41134, #10121, #9893, #5540, #23803, #37693, #2114, #16043, #29950, #31070, #42464, #20817, #4142, #10559, #24456, #283, #27666, #7569, #27887, #35367, #17838, #31287, #21482, #31511, #7340, #11228 ),
 ( #10780, #14416, #24243, #31734, #31954, #37913, #28326, #20602, #6690, #18063, #34477, #3919, #3483, #44998, #3256, #24676, #61, #17181, #38136, #719, #13974, #3697, #42238, #21034, #504, #14641, #28558, #38347, #7124, #13757, #10339, #35138, #41580, #6907, #34907, #34695, #14193, #28111, #42015, #38797, #17399, #41801, #11003, #17618, #38563, #21258, #24903, #8020, #8693, #39933, #28780, #39484, #36048, #4816, #32406, #1176, #43129, #36499, #11455, #18737, #39255, #5268, #8474, #22598, #33063, #18286, #42687, #32630, #32182, #25361, #19185, #21927, #35820, #15311, #22376, #4593, #22155, #25800, #1396, #29220, #1837, #18515, #15766, #43356, #36273, #43580, #11672, #18955, #953, #29667, #15091, #25135, #42910, #25581, #11899, #14870, #39029, #29002, #7800, #5041, #8248, #21709, #39710, #32846, #35596, #12125, #1614, #4366, #15536, #29440, #26027, #12578, #30347, #33980, #43812, #6174, #6409, #16904, #2748, #40161, #12350, #9835, #30796, #23517, #23054, #19405, #26248, #44270, #19628, #22824, #26483, #20317, #5711, #8922, #36715, #29895, #37163, #37405, #20095, #19862, #34201, #16672, #5940, #36940, #30568, #40846, #13027, #33512, #44487, #23745, #5485, #13254, #2293, #33292, #2067, #26925, #16221, #15991, #40387, #2975, #30126, #9148, #44039, #12803, #33751, #27156, #41079, #2520, #26703, #37636, #16447, #40614, #9372, #9601, #23281, #24185, #31674, #10502, #21200, #27827, #7284, #28273, #14360, #6, #17344, #20541, #17125, #41959, #37853, #18002, #13916, #34420, #20981, #38292, #34854, #444, #38077, #3201, #35078, #41523, #13480, #17558, #27383, #27609, #42182, #10942, #31014, #41738, #24403, #7070, #6855, #20762, #31453, #24845, #44944, #3640, #13701, #38737, #28051, #7507, #21422, #6627, #10280, #222, #34641, #3427, #35306, #31234, #14135, #10724, #24624, #38507, #3859, #17781, #4078, #44720, #41305, #10065, #23967, #4985, #43073, #5208, #18461, #25749, #25074, #36441, #14811, #43301, #4537, #32351, #39427, #21646, #1560, #21872, #29388, #11842, #25303 ) ),
 .UNSPECIFIED., .F., .F., .T. ) 
 B_SPLINE_SURFACE_WITH_KNOTS ( ( 2, 2 ),
 ( 3, 2, 2, 2, 2, 2, 2, 2, 2, 2, 2, 2, 2, 2, 2, 2, 2, 2, 2, 2, 2, 2, 2, 2, 2, 2, 2, 2, 2, 2, 2, 2, 2, 2, 2, 2, 2, 2, 2, 2, 2, 2, 2, 2, 2, 2, 2, 2, 2, 2, 2, 2, 2, 2, 2, 2, 2, 2, 2, 2, 2, 2, 2, 2, 2, 2, 2, 2, 2, 2, 2, 2, 2, 2, 2, 2, 2, 2, 2, 2, 2, 2, 2, 2, 2, 2, 2, 2, 2, 2, 2, 2, 2, 2, 2, 2, 2, 2, 2, 2, 2, 2, 2, 2, 2, 2, 2, 2, 2, 2, 2, 2, 2, 2, 2, 2, 2, 2, 2, 2, 2, 2, 2, 2, 2, 2, 2, 2, 3 ),
 ( 0.000000000000000000, 1.000000000000000000 ),
 ( 0.000000000000000000, 0.007812500000000000000, 0.01562500000000000000, 0.02343750000000000000, 0.03125000000000000000, 0.03906250000000000000, 0.04687500000000000000, 0.05468750000000000000, 0.06250000000000000000, 0.07031250000000000000, 0.07812500000000000000, 0.08593750000000000000, 0.09375000000000000000, 0.1015625000000000000, 0.1093750000000000000, 0.1171875000000000000, 0.1250000000000000000, 0.1328125000000000000, 0.1406250000000000000, 0.1484375000000000000, 0.1562500000000000000, 0.1640625000000000000, 0.1718750000000000000, 0.1796875000000000000, 0.1875000000000000000, 0.1953125000000000000, 0.2031250000000000000, 0.2109375000000000000, 0.2187500000000000000, 0.2265625000000000000, 0.2343750000000000000, 0.2421875000000000000, 0.2500000000000000000, 0.2578125000000000000, 0.2656250000000000000, 0.2734375000000000000, 0.2812500000000000000, 0.2890625000000000000, 0.2968750000000000000, 0.3046875000000000000, 0.3125000000000000000, 0.3203125000000000000, 0.3281250000000000000, 0.3359375000000000000, 0.3437500000000000000, 0.3515625000000000000, 0.3593750000000000000, 0.3671875000000000000, 0.3750000000000000000, 0.3828125000000000000, 0.3906250000000000000, 0.3984375000000000000, 0.4062500000000000000, 0.4140625000000000000, 0.4218750000000000000, 0.4296875000000000000, 0.4375000000000000000, 0.4453125000000000000, 0.4531250000000000000, 0.4609375000000000000, 0.4687500000000000000, 0.4765625000000000000, 0.4843750000000000000, 0.4921875000000000000, 0.5000000000000000000, 0.5078125000000000000, 0.5156250000000000000, 0.5234375000000000000, 0.5312500000000000000, 0.5390625000000000000, 0.5468750000000000000, 0.5546875000000000000, 0.5625000000000000000, 0.5703125000000000000, 0.5781250000000000000, 0.5859375000000000000, 0.5937500000000000000, 0.6015625000000000000, 0.6093750000000000000, 0.6171875000000000000, 0.6250000000000000000, 0.6328125000000000000, 0.6406250000000000000, 0.6484375000000000000, 0.6562500000000000000, 0.6640625000000000000, 0.6718750000000000000, 0.6796875000000000000, 0.6875000000000000000, 0.6953125000000000000, 0.7031250000000000000, 0.7109375000000000000, 0.7187500000000000000, 0.7265625000000000000, 0.7343750000000000000, 0.7421875000000000000, 0.7500000000000000000, 0.7578125000000000000, 0.7656250000000000000, 0.7734375000000000000, 0.7812500000000000000, 0.7890625000000000000, 0.7968750000000000000, 0.8046875000000000000, 0.8125000000000000000, 0.8203125000000000000, 0.8281250000000000000, 0.8359375000000000000, 0.8437500000000000000, 0.8515625000000000000, 0.8593750000000000000, 0.8671875000000000000, 0.8750000000000000000, 0.8828125000000000000, 0.8906250000000000000, 0.8984375000000000000, 0.9062500000000000000, 0.9140625000000000000, 0.9218750000000000000, 0.9296875000000000000, 0.9375000000000000000, 0.9453125000000000000, 0.9531250000000000000, 0.9609375000000000000, 0.9687500000000000000, 0.9765625000000000000, 0.9843750000000000000, 0.9921875000000000000, 1.000000000000000000 ),
 .UNSPECIFIED. ) 
 GEOMETRIC_REPRESENTATION_ITEM ( )  RATIONAL_B_SPLINE_SURFACE ( (
 ( 1.000000000000000000, 0.9238795325112869605, 1.000000000000000000, 0.9238795325112869605, 1.000000000000000000, 0.9238795325112869605, 1.000000000000000000, 0.9238795325112869605, 1.000000000000000000, 0.9238795325112869605, 1.000000000000000000, 0.9238795325112869605, 1.000000000000000000, 0.9238795325112869605, 1.000000000000000000, 0.9238795325112869605, 1.000000000000000000, 0.9238795325112869605, 1.000000000000000000, 0.9238795325112869605, 1.000000000000000000, 0.9238795325112869605, 1.000000000000000000, 0.9238795325112869605, 1.000000000000000000, 0.9238795325112869605, 1.000000000000000000, 0.9238795325112869605, 1.000000000000000000, 0.9238795325112869605, 1.000000000000000000, 0.9238795325112869605, 1.000000000000000000, 0.9238795325112869605, 1.000000000000000000, 0.9238795325112869605, 1.000000000000000000, 0.9238795325112869605, 1.000000000000000000, 0.9238795325112869605, 1.000000000000000000, 0.9238795325112869605, 1.000000000000000000, 0.9238795325112869605, 1.000000000000000000, 0.9238795325112869605, 1.000000000000000000, 0.9238795325112869605, 1.000000000000000000, 0.9238795325112869605, 1.000000000000000000, 0.9238795325112869605, 1.000000000000000000, 0.9238795325112869605, 1.000000000000000000, 0.9238795325112869605, 1.000000000000000000, 0.9238795325112869605, 1.000000000000000000, 0.9238795325112869605, 1.000000000000000000, 0.9238795325112869605, 1.000000000000000000, 0.9238795325112869605, 1.000000000000000000, 0.9238795325112869605, 1.000000000000000000, 0.9238795325112869605, 1.000000000000000000, 0.9238795325112869605, 1.000000000000000000, 0.9238795325112869605, 1.000000000000000000, 0.9238795325112869605, 1.000000000000000000, 0.9238795325112869605, 1.000000000000000000, 0.9238795325112869605, 1.000000000000000000, 0.9238795325112869605, 1.000000000000000000, 0.9238795325112869605, 1.000000000000000000, 0.9238795325112869605, 1.000000000000000000, 0.9238795325112869605, 1.000000000000000000, 0.9238795325112869605, 1.000000000000000000, 0.9238795325112869605, 1.000000000000000000, 0.9238795325112869605, 1.000000000000000000, 0.9238795325112869605, 1.000000000000000000, 0.9238795325112869605, 1.000000000000000000, 0.9238795325112869605, 1.000000000000000000, 0.9238795325112869605, 1.000000000000000000, 0.9238795325112869605, 1.000000000000000000, 0.9238795325112869605, 1.000000000000000000, 0.9238795325112869605, 1.000000000000000000, 0.9238795325112869605, 1.000000000000000000, 0.9238795325112869605, 1.000000000000000000, 0.9238795325112869605, 1.000000000000000000, 0.9238795325112869605, 1.000000000000000000, 0.9238795325112869605, 1.000000000000000000, 0.9238795325112869605, 1.000000000000000000, 0.9238795325112869605, 1.000000000000000000, 0.9238795325112869605, 1.000000000000000000, 0.9238795325112869605, 1.000000000000000000, 0.9238795325112869605, 1.000000000000000000, 0.9238795325112869605, 1.000000000000000000, 0.9238795325112869605, 1.000000000000000000, 0.9238795325112869605, 1.000000000000000000, 0.9238795325112869605, 1.000000000000000000, 0.9238795325112869605, 1.000000000000000000, 0.9238795325112869605, 1.000000000000000000, 0.9238795325112869605, 1.000000000000000000, 0.9238795325112869605, 1.000000000000000000, 0.9238795325112869605, 1.000000000000000000, 0.9238795325112869605, 1.000000000000000000, 0.9238795325112869605, 1.000000000000000000, 0.9238795325112869605, 1.000000000000000000, 0.9238795325112869605, 1.000000000000000000, 0.9238795325112869605, 1.000000000000000000, 0.9238795325112869605, 1.000000000000000000, 0.9238795325112869605, 1.000000000000000000, 0.9238795325112869605, 1.000000000000000000, 0.9238795325112869605, 1.000000000000000000, 0.9238795325112869605, 1.000000000000000000, 0.9238795325112869605, 1.000000000000000000, 0.9238795325112869605, 1.000000000000000000, 0.9238795325112869605, 1.000000000000000000, 0.9238795325112869605, 1.000000000000000000, 0.9238795325112869605, 1.000000000000000000, 0.9238795325112869605, 1.000000000000000000, 0.9238795325112869605, 1.000000000000000000, 0.9238795325112869605, 1.000000000000000000, 0.9238795325112869605, 1.000000000000000000, 0.9238795325112869605, 1.000000000000000000, 0.9238795325112869605, 1.000000000000000000, 0.9238795325112869605, 1.000000000000000000, 0.9238795325112869605, 1.000000000000000000, 0.9238795325112869605, 1.000000000000000000, 0.9238795325112869605, 1.000000000000000000, 0.9238795325112869605, 1.000000000000000000, 0.9238795325112869605, 1.000000000000000000, 0.9238795325112869605, 1.000000000000000000, 0.9238795325112869605, 1.000000000000000000, 0.9238795325112869605, 1.000000000000000000, 0.9238795325112869605, 1.000000000000000000, 0.9238795325112869605, 1.000000000000000000, 0.9238795325112869605, 1.000000000000000000, 0.9238795325112869605, 1.000000000000000000, 0.9238795325112869605, 1.000000000000000000, 0.9238795325112869605, 1.000000000000000000, 0.9238795325112869605, 1.000000000000000000, 0.9238795325112869605, 1.000000000000000000, 0.9238795325112869605, 1.000000000000000000, 0.9238795325112869605, 1.000000000000000000, 0.9238795325112869605, 1.000000000000000000, 0.9238795325112869605, 1.000000000000000000, 0.9238795325112869605, 1.000000000000000000, 0.9238795325112869605, 1.000000000000000000, 0.9238795325112869605, 1.000000000000000000, 0.9238795325112869605, 1.000000000000000000, 0.9238795325112869605, 1.000000000000000000, 0.9238795325112869605, 1.000000000000000000, 0.9238795325112869605, 1.000000000000000000, 0.9238795325112869605, 1.000000000000000000, 0.9238795325112869605, 1.000000000000000000, 0.9238795325112869605, 1.000000000000000000, 0.9238795325112869605, 1.000000000000000000, 0.9238795325112869605, 1.000000000000000000, 0.9238795325112869605, 1.000000000000000000, 0.9238795325112869605, 1.000000000000000000),
 ( 1.000000000000000000, 0.9238795325112869605, 1.000000000000000000, 0.9238795325112869605, 1.000000000000000000, 0.9238795325112869605, 1.000000000000000000, 0.9238795325112869605, 1.000000000000000000, 0.9238795325112869605, 1.000000000000000000, 0.9238795325112869605, 1.000000000000000000, 0.9238795325112869605, 1.000000000000000000, 0.9238795325112869605, 1.000000000000000000, 0.9238795325112869605, 1.000000000000000000, 0.9238795325112869605, 1.000000000000000000, 0.9238795325112869605, 1.000000000000000000, 0.9238795325112869605, 1.000000000000000000, 0.9238795325112869605, 1.000000000000000000, 0.9238795325112869605, 1.000000000000000000, 0.9238795325112869605, 1.000000000000000000, 0.9238795325112869605, 1.000000000000000000, 0.9238795325112869605, 1.000000000000000000, 0.9238795325112869605, 1.000000000000000000, 0.9238795325112869605, 1.000000000000000000, 0.9238795325112869605, 1.000000000000000000, 0.9238795325112869605, 1.000000000000000000, 0.9238795325112869605, 1.000000000000000000, 0.9238795325112869605, 1.000000000000000000, 0.9238795325112869605, 1.000000000000000000, 0.9238795325112869605, 1.000000000000000000, 0.9238795325112869605, 1.000000000000000000, 0.9238795325112869605, 1.000000000000000000, 0.9238795325112869605, 1.000000000000000000, 0.9238795325112869605, 1.000000000000000000, 0.9238795325112869605, 1.000000000000000000, 0.9238795325112869605, 1.000000000000000000, 0.9238795325112869605, 1.000000000000000000, 0.9238795325112869605, 1.000000000000000000, 0.9238795325112869605, 1.000000000000000000, 0.9238795325112869605, 1.000000000000000000, 0.9238795325112869605, 1.000000000000000000, 0.9238795325112869605, 1.000000000000000000, 0.9238795325112869605, 1.000000000000000000, 0.9238795325112869605, 1.000000000000000000, 0.9238795325112869605, 1.000000000000000000, 0.9238795325112869605, 1.000000000000000000, 0.9238795325112869605, 1.000000000000000000, 0.9238795325112869605, 1.000000000000000000, 0.9238795325112869605, 1.000000000000000000, 0.9238795325112869605, 1.000000000000000000, 0.9238795325112869605, 1.000000000000000000, 0.9238795325112869605, 1.000000000000000000, 0.9238795325112869605, 1.000000000000000000, 0.9238795325112869605, 1.000000000000000000, 0.9238795325112869605, 1.000000000000000000, 0.9238795325112869605, 1.000000000000000000, 0.9238795325112869605, 1.000000000000000000, 0.9238795325112869605, 1.000000000000000000, 0.9238795325112869605, 1.000000000000000000, 0.9238795325112869605, 1.000000000000000000, 0.9238795325112869605, 1.000000000000000000, 0.9238795325112869605, 1.000000000000000000, 0.9238795325112869605, 1.000000000000000000, 0.9238795325112869605, 1.000000000000000000, 0.9238795325112869605, 1.000000000000000000, 0.9238795325112869605, 1.000000000000000000, 0.9238795325112869605, 1.000000000000000000, 0.9238795325112869605, 1.000000000000000000, 0.9238795325112869605, 1.000000000000000000, 0.9238795325112869605, 1.000000000000000000, 0.9238795325112869605, 1.000000000000000000, 0.9238795325112869605, 1.000000000000000000, 0.9238795325112869605, 1.000000000000000000, 0.9238795325112869605, 1.000000000000000000, 0.9238795325112869605, 1.000000000000000000, 0.9238795325112869605, 1.000000000000000000, 0.9238795325112869605, 1.000000000000000000, 0.9238795325112869605, 1.000000000000000000, 0.9238795325112869605, 1.000000000000000000, 0.9238795325112869605, 1.000000000000000000, 0.9238795325112869605, 1.000000000000000000, 0.9238795325112869605, 1.000000000000000000, 0.9238795325112869605, 1.000000000000000000, 0.9238795325112869605, 1.000000000000000000, 0.9238795325112869605, 1.000000000000000000, 0.9238795325112869605, 1.000000000000000000, 0.9238795325112869605, 1.000000000000000000, 0.9238795325112869605, 1.000000000000000000, 0.9238795325112869605, 1.000000000000000000, 0.9238795325112869605, 1.000000000000000000, 0.9238795325112869605, 1.000000000000000000, 0.9238795325112869605, 1.000000000000000000, 0.9238795325112869605, 1.000000000000000000, 0.9238795325112869605, 1.000000000000000000, 0.9238795325112869605, 1.000000000000000000, 0.9238795325112869605, 1.000000000000000000, 0.9238795325112869605, 1.000000000000000000, 0.9238795325112869605, 1.000000000000000000, 0.9238795325112869605, 1.000000000000000000, 0.9238795325112869605, 1.000000000000000000, 0.9238795325112869605, 1.000000000000000000, 0.9238795325112869605, 1.000000000000000000, 0.9238795325112869605, 1.000000000000000000, 0.9238795325112869605, 1.000000000000000000, 0.9238795325112869605, 1.000000000000000000, 0.9238795325112869605, 1.000000000000000000, 0.9238795325112869605, 1.000000000000000000, 0.9238795325112869605, 1.000000000000000000, 0.9238795325112869605, 1.000000000000000000, 0.9238795325112869605, 1.000000000000000000, 0.9238795325112869605, 1.000000000000000000, 0.9238795325112869605, 1.000000000000000000, 0.9238795325112869605, 1.000000000000000000, 0.9238795325112869605, 1.000000000000000000, 0.9238795325112869605, 1.000000000000000000, 0.9238795325112869605, 1.000000000000000000, 0.9238795325112869605, 1.000000000000000000, 0.9238795325112869605, 1.000000000000000000, 0.9238795325112869605, 1.000000000000000000, 0.9238795325112869605, 1.000000000000000000, 0.9238795325112869605, 1.000000000000000000, 0.9238795325112869605, 1.000000000000000000, 0.9238795325112869605, 1.000000000000000000, 0.9238795325112869605, 1.000000000000000000, 0.9238795325112869605, 1.000000000000000000, 0.9238795325112869605, 1.000000000000000000, 0.9238795325112869605, 1.000000000000000000, 0.9238795325112869605, 1.000000000000000000, 0.9238795325112869605, 1.000000000000000000, 0.9238795325112869605, 1.000000000000000000, 0.9238795325112869605, 1.000000000000000000, 0.9238795325112869605, 1.000000000000000000, 0.9238795325112869605, 1.000000000000000000) ) ) 
 REPRESENTATION_ITEM ( '' )  SURFACE ( )  );
#24695 = CARTESIAN_POINT ( 'NONE',  ( 124.5613353876793639, -9.862207337050596934, -13.58011646024242403 ) ) ;
#24696 = DIRECTION ( 'NONE',  ( 0.000000000000000000, 0.6004852223388321697, -0.7996358532186279566 ) ) ;
#24697 = VERTEX_POINT ( 'NONE', #41767 ) ;
#24698 = CARTESIAN_POINT ( 'NONE',  ( 121.4964260444391755, -1.267766418764731728, -16.93314635290706605 ) ) ;
#24699 = CARTESIAN_POINT ( 'NONE',  ( 125.0211000582876721, -2.337644349080307826, -6.269163357979471662 ) ) ;
#24700 = CARTESIAN_POINT ( 'NONE',  ( 116.5249890045247980, 0.8980012041604421569, -15.77991374673208469 ) ) ;
#24701 = CARTESIAN_POINT ( 'NONE',  ( 114.3846081442453197, -10.63000616557722466, -14.87417383870573495 ) ) ;
#24702 = CARTESIAN_POINT ( 'NONE',  ( 112.0588148109119828, 0.5811942927096154232, -14.16772938898807155 ) ) ;
#24703 = CARTESIAN_POINT ( 'NONE',  ( 116.5402214775786405, -9.565557343593413364, -10.61323700422348004 ) ) ;
#24704 = CARTESIAN_POINT ( 'NONE',  ( 113.3751581415389040, -0.1020945015694913471, -15.74893487844866691 ) ) ;
#24705 = ORIENTED_EDGE ( 'NONE', *, *, #42046, .T. ) ;
#24706 = CARTESIAN_POINT ( 'NONE',  ( 114.4980614775786734, -2.084020599724406786, -8.691656652584148546 ) ) ;
#24707 = FACE_OUTER_BOUND ( 'NONE', #3073, .T. ) ;
#24708 = CARTESIAN_POINT ( 'NONE',  ( 84.90318689630748850, -29.89078148095193654, -11.34622365899691943 ) ) ;
#24709 = LINE ( 'NONE', #28592, #39270 ) ;
#24710 = CONICAL_SURFACE ( 'NONE', #43653, 2.445500000000004448, 0.9599310885968757034 ) ;
#24711 = CARTESIAN_POINT ( 'NONE',  ( 114.2144281442453178, -8.166667518702817929, -8.995218007635859436 ) ) ;
#24712 = EDGE_LOOP ( 'NONE', ( #36310, #24319, #23531, #27449, #8711 ) ) ;
#24713 = CARTESIAN_POINT ( 'NONE',  ( 116.0296814775786345, -8.166667518702817929, -8.995218007635861213 ) ) ;
#24714 = AXIS2_PLACEMENT_3D ( 'NONE', #7842, #28821, #21297 ) ;
#24715 = CARTESIAN_POINT ( 'NONE',  ( 85.75809888461174069, -18.45227461768569199, -19.39321520033831447 ) ) ;
#24716 = CARTESIAN_POINT ( 'NONE',  ( 111.1076452545248259, 0.8980012041604421569, -11.00651665394454071 ) ) ;
#24717 = CARTESIAN_POINT ( 'NONE',  ( 112.8529881442453302, -1.561330072975668060, -17.79121239304076596 ) ) ;
#24718 = CARTESIAN_POINT ( 'NONE',  ( 114.1009748109119784, -4.089484607189486809, -7.948022111789456723 ) ) ;
#24719 = CARTESIAN_POINT ( 'NONE',  ( 124.2550481442452792, -0.1624402480850797581, -16.17319339645315424 ) ) ;
#24720 = EDGE_CURVE ( 'NONE', #38298, #40576, #14312, .T. ) ;
#24721 = CARTESIAN_POINT ( 'NONE',  ( 64.46696884417693241, -15.35047623415474405, -15.89321305673442986 ) ) ;
#24722 = CARTESIAN_POINT ( 'NONE',  ( 107.9822546295247889, -4.863998795839590272, -18.39754474579285315 ) ) ;
#24723 = VERTEX_POINT ( 'NONE', #31480 ) ;
#24724 = CARTESIAN_POINT ( 'NONE',  ( 112.0105358795247810, -0.7896495226426338832, -17.46756447353520159 ) ) ;
#24725 = CARTESIAN_POINT ( 'NONE',  ( 109.2296352495891796, -8.786749211135761684, -17.08468090821677166 ) ) ;
#24726 = CARTESIAN_POINT ( 'NONE',  ( 116.4834948109119779, -7.894159318335828068, -9.358103419637847864 ) ) ;
#24727 = CARTESIAN_POINT ( 'NONE',  ( 107.1488171295247867, -10.62599879583958540, -13.39321520033831447 ) ) ;
#24728 = CARTESIAN_POINT ( 'NONE',  ( 116.6638952545248031, -9.868328341294098749, -15.46607636864997204 ) ) ;
#24729 = CARTESIAN_POINT ( 'NONE',  ( 109.1629577545248395, -7.250697342233347165, -7.631215200338321125 ) ) ;
#24730 = CARTESIAN_POINT ( 'NONE',  ( 124.1773369107181821, -2.467220198592779301, -17.83387418641524391 ) ) ;
#24731 = CARTESIAN_POINT ( 'NONE',  ( 111.6617281442453304, 0.4262465694468514643, -12.03445270309931736 ) ) ;
#24732 = DIRECTION ( 'NONE',  ( -1.000000000000000000, 0.000000000000000000, 0.000000000000000000 ) ) ;
#24733 = CARTESIAN_POINT ( 'NONE',  ( 125.3895814775786448, -7.893985811506177619, -18.51759400769804742 ) ) ;
#24734 = CARTESIAN_POINT ( 'NONE',  ( 116.2565881442452991, -9.261995988541697145, -16.69588392320189030 ) ) ;
#24735 = EDGE_LOOP ( 'NONE', ( #13598, #23689, #44434, #28282 ) ) ;
#24736 = CARTESIAN_POINT ( 'NONE',  ( 113.2500748109119968, -3.505236298600246325, -18.68346056562440793 ) ) ;
#24737 = CARTESIAN_POINT ( 'NONE',  ( 125.6732148109119862, 0.5811942927096110934, -14.16772938898807510 ) ) ;
#24738 = CARTESIAN_POINT ( 'NONE',  ( 116.4267681442453153, -3.383040157471821630, -19.15922257007629170 ) ) ;
#24739 = CARTESIAN_POINT ( 'NONE',  ( 117.7882081442453170, -3.505236298600246325, -18.68346056562440793 ) ) ;
#24740 = ORIENTED_EDGE ( 'NONE', *, *, #3275, .F. ) ;
#24741 = EDGE_CURVE ( 'NONE', #23514, #27457, #40820, .T. ) ;
#24742 = CARTESIAN_POINT ( 'NONE',  ( 123.1205148109119563, -7.643976991954077427, -18.09477374809248928 ) ) ;
#24743 = EDGE_CURVE ( 'NONE', #32138, #44381, #27412, .T. ) ;
#24744 = EDGE_CURVE ( 'NONE', #29882, #38699, #10751, .T. ) ;
#24745 = CARTESIAN_POINT ( 'NONE',  ( 114.9518748109119883, -1.834011780172310813, -8.268836392978581529 ) ) ;
#24746 = AXIS2_PLACEMENT_3D ( 'NONE', #32836, #39475, #8465 ) ;
#24747 = CARTESIAN_POINT ( 'NONE',  ( 136.5795292550376132, 0.4320203884789947102, -15.53198663114375222 ) ) ;
#24748 = CARTESIAN_POINT ( 'NONE',  ( 108.9545983795247821, -0.7896495226426338832, -9.318865927141430916 ) ) ;
#24749 = CARTESIAN_POINT ( 'NONE',  ( 70.19189222814998175, -50.70706315265230302, -33.48565765860439569 ) ) ;
#24750 = CARTESIAN_POINT ( 'NONE',  ( 126.7218814084904182, 0.3870001044524405964, -13.29043313491086842 ) ) ;
#24751 = CARTESIAN_POINT ( 'NONE',  ( 116.8028015045247940, -6.936859964151250502, -18.39754474579286025 ) ) ;
#24752 = AXIS2_PLACEMENT_3D ( 'NONE', #37792, #27769, #10000 ) ;
#24753 = CARTESIAN_POINT ( 'NONE',  ( 115.9729548109119861, -6.344957434206662583, -7.627207830600332805 ) ) ;
#24754 = VECTOR ( 'NONE', #16125, 1000.000000000000000 ) ;
#24755 = CARTESIAN_POINT ( 'NONE',  ( 124.6736757622208671, -8.623525442416562825, -16.74998043996585650 ) ) ;
#24756 = CARTESIAN_POINT ( 'NONE',  ( 111.5473838361194794, 0.1075849324168598464, -12.14321520033829671 ) ) ;
#24757 = CARTESIAN_POINT ( 'NONE',  ( 63.74703025577719018, -40.95155355269160680, -15.89321520033831447 ) ) ;
#24758 = CARTESIAN_POINT ( 'NONE',  ( 116.9417077545247992, -2.791137627527939813, -18.39754474579286025 ) ) ;
#24759 = CARTESIAN_POINT ( 'NONE',  ( 114.1009748109119784, -5.574606645277164318, -18.38911715685844683 ) ) ;
#24760 = EDGE_CURVE ( 'NONE', #11611, #29815, #86, .T. ) ;
#24761 = CARTESIAN_POINT ( 'NONE',  ( 70.19189222814998175, -100.0979043305785581, -53.24182196210380624 ) ) ;
#24763 = CARTESIAN_POINT ( 'NONE',  ( 115.4624148109119943, -5.638512984488999180, -18.83840828888717311 ) ) ;
#24762 = CARTESIAN_POINT ( 'NONE',  ( 124.3273610609119828, -6.340755971794960644, -8.611740276972867036 ) ) ;
#24764 = PLANE ( 'NONE',  #11830 ) ;
#24765 = CARTESIAN_POINT ( 'NONE',  ( 117.7314814775786260, -5.574606645277164318, -18.38911715685844683 ) ) ;
#24766 = EDGE_LOOP ( 'NONE', ( #14324, #17028, #22640, #26871, #25370 ) ) ;
#24767 = CARTESIAN_POINT ( 'NONE',  ( 136.7860375664301102, -9.155735703506769241, -9.793839820488711823 ) ) ;
#24768 = CARTESIAN_POINT ( 'NONE',  ( 122.7801548109119665, -3.383040157471821630, -19.15922257007629170 ) ) ;
#24769 = CARTESIAN_POINT ( 'NONE',  ( 114.3719421295247827, -9.868328341294093420, -13.39321520033831447 ) ) ;
#24770 = CARTESIAN_POINT ( 'NONE',  ( 118.5823814775786360, -7.643976991954077427, -18.09477374809248928 ) ) ;
#24771 = EDGE_CURVE ( 'NONE', #42142, #7750, #21151, .T. ) ;
#24772 = CARTESIAN_POINT ( 'NONE',  ( 113.3635281442453504, -0.1624402480850797581, -16.17319339645315424 ) ) ;
#24773 = EDGE_CURVE ( 'NONE', #3515, #41752, #23528, .T. ) ;
#24774 = DIRECTION ( 'NONE',  ( 0.000000000000000000, -0.9242245927363028635, -0.3818493186865930533 ) ) ;
#24775 = CARTESIAN_POINT ( 'NONE',  ( 111.7327233795247849, -8.938348069036489818, -17.46756447353520159 ) ) ;
#24776 = CARTESIAN_POINT ( 'NONE',  ( 118.9794681442453026, -0.8288870151387760510, -10.36305467784173118 ) ) ;
#24777 = CARTESIAN_POINT ( 'NONE',  ( 119.2631014775786298, -9.565557343593413364, -10.61323700422348004 ) ) ;
#24778 = CARTESIAN_POINT ( 'NONE',  ( 67.08264006073221708, -20.21382323020432992, -10.39321520033831625 ) ) ;
#24779 = AXIS2_PLACEMENT_3D ( 'NONE', #23448, #33444, #2908 ) ;
#24780 = CARTESIAN_POINT ( 'NONE',  ( 109.2294428007942741, -3.526316717755844987, -8.039392986164429544 ) ) ;
#24781 = CARTESIAN_POINT ( 'NONE',  ( 121.2019704359119743, 1.345710702986147034, -13.97328579221134426 ) ) ;
#24782 = CARTESIAN_POINT ( 'NONE',  ( 109.8574890045247940, -9.868328341294098749, -11.32035403202665869 ) ) ;
#24783 =( BOUNDED_CURVE ( )  B_SPLINE_CURVE ( 2, ( #16816, #9288, #43945, #16127, #23196, #30031, #30480, #12712, #23653, #6770, #3115, #37075, #19770, #2429, #2887, #17040, #20000 ),
 .UNSPECIFIED., .F., .T. ) 
 B_SPLINE_CURVE_WITH_KNOTS ( ( 3, 2, 2, 2, 2, 2, 2, 2, 3 ),
 ( 0.5089135524044680059, 0.5312500000000000000, 0.5625000000000000000, 0.5937500000000000000, 0.6250000000000000000, 0.6562500000000000000, 0.6875000000000000000, 0.7187500000000000000, 0.7410864475955319941 ),
 .UNSPECIFIED. ) 
 CURVE ( )  GEOMETRIC_REPRESENTATION_ITEM ( )  RATIONAL_B_SPLINE_CURVE ( ( 0.9689618144536780164, 0.9455916533437099813, 1.000000000000000000, 0.9238795325112869605, 1.000000000000000000, 0.9238795325112869605, 1.000000000000000000, 0.9238795325112869605, 1.000000000000000000, 0.9238795325112869605, 1.000000000000000000, 0.9238795325112869605, 1.000000000000000000, 0.9238795325112869605, 1.000000000000000000, 0.9455916533437099813, 0.9689618144536780164 ) ) 
 REPRESENTATION_ITEM ( '' )  );
#24784 = CYLINDRICAL_SURFACE ( 'NONE', #6575, 4.500000000000003553 ) ;
#24785 = CARTESIAN_POINT ( 'NONE',  ( 118.7525614775786380, -8.166667518702819706, -8.995218007635861213 ) ) ;
#24786 = CARTESIAN_POINT ( 'NONE',  ( 116.3700414775786527, -5.638512984488999180, -18.83840828888717311 ) ) ;
#24787 = CARTESIAN_POINT ( 'NONE',  ( 109.9963952545248134, 0.8980012041604421569, -11.00651665394454071 ) ) ;
#24788 = CARTESIAN_POINT ( 'NONE',  ( 112.4559014775786494, -9.988377603198976828, -10.36322818467138340 ) ) ;
#24789 = EDGE_LOOP ( 'NONE', ( #4529, #31517, #2826, #27099, #15553 ) ) ;
#24790 = CARTESIAN_POINT ( 'NONE',  ( 112.9455131944929462, -1.036737761566191018, -17.24079555149560150 ) ) ;
#24791 = CARTESIAN_POINT ( 'NONE',  ( 122.5532481442453019, -10.63000616557722466, -14.87417383870573495 ) ) ;
#24792 = VECTOR ( 'NONE', #3145, 999.9999999999998863 ) ;
#24793 = CARTESIAN_POINT ( 'NONE',  ( 116.2565881442452991, -9.261995988541697145, -16.69588392320189030 ) ) ;
#24794 = CARTESIAN_POINT ( 'NONE',  ( 120.4543614775786295, -5.574606645277164318, -18.38911715685844683 ) ) ;
#24795 =( LENGTH_UNIT ( ) NAMED_UNIT ( * ) SI_UNIT ( .MILLI., .METRE. ) );
#24796 = CIRCLE ( 'NONE', #14605, 3.500000000000003109 ) ;
#24797 = CARTESIAN_POINT ( 'NONE',  ( 112.1155414775786454, -10.15424416112533912, -14.75197769757731336 ) ) ;
#24798 = CARTESIAN_POINT ( 'NONE',  ( 123.2339681442453241, -6.344957434206665248, -7.627207830600338134 ) ) ;
#24799 = ADVANCED_FACE ( 'NONE', ( #37883 ), #16702, .F. ) ;
#24800 = CARTESIAN_POINT ( 'NONE',  ( 115.7610046295247912, -4.863998795839590272, -7.631215200338315796 ) ) ;
#24801 = CARTESIAN_POINT ( 'NONE',  ( 115.0653281442453277, -3.505236298600246325, -18.68346056562440793 ) ) ;
#24802 = CARTESIAN_POINT ( 'NONE',  ( 116.0286950891469786, 2.331313199634366118, -4.893215200338314474 ) ) ;
#24803 = ORIENTED_EDGE ( 'NONE', *, *, #25873, .F. ) ;
#24804 = CARTESIAN_POINT ( 'NONE',  ( 123.0637881442452937, -0.4660016031367893996, -10.09054647747474043 ) ) ;
#24805 = CARTESIAN_POINT ( 'NONE',  ( 122.9382985609119743, -10.36940331770106916, -15.09355782777062061 ) ) ;
#24806 = CARTESIAN_POINT ( 'NONE',  ( 119.4332814775786318, -0.4660016031367893996, -10.09054647747474043 ) ) ;
#24807 = ORIENTED_EDGE ( 'NONE', *, *, #28670, .T. ) ;
#24808 = CARTESIAN_POINT ( 'NONE',  ( 115.8304577545247582, -7.250697342233347165, -7.631215200338321125 ) ) ;
#24809 = CARTESIAN_POINT ( 'NONE',  ( 124.3117748109119844, -10.30919188438810075, -12.61870101168855918 ) ) ;
#24810 = VECTOR ( 'NONE', #6685, 1000.000000000000227 ) ;
#24811 = CARTESIAN_POINT ( 'NONE',  ( 88.35093386163799778, -26.75858941326842810, -11.54476601486570964 ) ) ;
#24812 = CARTESIAN_POINT ( 'NONE',  ( 116.4834948109119779, -7.894159318335828068, -9.358103419637847864 ) ) ;
#24813 = CARTESIAN_POINT ( 'NONE',  ( 75.95778847736481509, -3.256761025687722189, -16.89321520033831447 ) ) ;
#24814 = CARTESIAN_POINT ( 'NONE',  ( 121.4187148109119789, -3.505236298600246325, -18.68346056562440793 ) ) ;
#24815 = CARTESIAN_POINT ( 'NONE',  ( 121.0408330757767459, -0.9924539043446216624, -17.29976612834909133 ) ) ;
#24816 = CARTESIAN_POINT ( 'NONE',  ( 122.7234281442452755, -4.153390946401325223, -8.397313243818185668 ) ) ;
#24817 = CIRCLE ( 'NONE', #5870, 5.000000000000004441 ) ;
#24818 = CARTESIAN_POINT ( 'NONE',  ( 125.1028739313169496, -10.94014759239619039, -9.048497972336113193 ) ) ;
#24819 = CARTESIAN_POINT ( 'NONE',  ( 117.9583881442453048, 0.1319031606808879209, -14.10382304977623669 ) ) ;
#24820 = CIRCLE ( 'NONE', #43746, 5.132259260909280307 ) ;
#24821 = CARTESIAN_POINT ( 'NONE',  ( 122.2437673109119629, 0.2312338769422704887, -16.08380026872395874 ) ) ;
#24822 = CARTESIAN_POINT ( 'NONE',  ( 116.4834948109119779, -1.561330072975668504, -17.79121239304076951 ) ) ;
#24823 = CARTESIAN_POINT ( 'NONE',  ( 122.6009548109119720, -11.97804492312076086, -17.05249760251924229 ) ) ;
#24824 = ADVANCED_BREP_SHAPE_REPRESENTATION ( '', ( #36408, #12375 ), #14045 ) ;
#24825 = CARTESIAN_POINT ( 'NONE',  ( 119.2631014775786298, -9.565557343593413364, -10.61323700422348004 ) ) ;
#24826 = ORIENTED_EDGE ( 'NONE', *, *, #19286, .T. ) ;
#24827 = CARTESIAN_POINT ( 'NONE',  ( 115.1787814775786387, -9.988377603198976828, -10.36322818467138340 ) ) ;
#24828 = CARTESIAN_POINT ( 'NONE',  ( 113.4690515045247992, -6.936859964151250502, -18.39754474579286025 ) ) ;
#24829 = CARTESIAN_POINT ( 'NONE',  ( 122.6009548109119720, -11.17722486020181627, -8.479644537342501565 ) ) ;
#24830 = CARTESIAN_POINT ( 'NONE',  ( 70.19189222814998175, -57.98054017398621340, -36.39502311309316696 ) ) ;
#24831 = DIRECTION ( 'NONE',  ( 0.000000000000000000, -0.3818493186865927203, 0.9242245927363029745 ) ) ;
#24832 = CARTESIAN_POINT ( 'NONE',  ( 123.4041481442452834, -10.30919188438810075, -12.61870101168855918 ) ) ;
#24833 = ORIENTED_EDGE ( 'NONE', *, *, #44062, .F. ) ;
#24834 = CARTESIAN_POINT ( 'NONE',  ( 84.10862215250544693, -26.60966817898065884, -11.90521360603286816 ) ) ;
#24835 = CARTESIAN_POINT ( 'NONE',  ( 120.9649014775786355, -6.222761293078241884, -8.102969835052219238 ) ) ;
#24836 = DIRECTION ( 'NONE',  ( -0.000000000000000000, -0.9284778069183721172, -0.3713878862591650232 ) ) ;
#24837 = CARTESIAN_POINT ( 'NONE',  ( 65.71132926441107713, -16.34206498534276264, -16.79547554155828593 ) ) ;
#24838 = EDGE_CURVE ( 'NONE', #38575, #11904, #41104, .T. ) ;
#24839 = CARTESIAN_POINT ( 'NONE',  ( 125.9001214775786224, -4.089484607189486809, -7.948022111789456723 ) ) ;
#24840 = CARTESIAN_POINT ( 'NONE',  ( 110.8992858795247827, -8.402594152722688392, -9.854619843455216355 ) ) ;
#24841 = DIRECTION ( 'NONE',  ( 0.000000000000000000, -0.9242245927363028635, -0.3818493186865930533 ) ) ;
#24842 = VERTEX_POINT ( 'NONE', #6436 ) ;
#24843 = CARTESIAN_POINT ( 'NONE',  ( 116.1998614775786507, -10.63000616557722466, -14.87417383870573495 ) ) ;
#24844 = CARTESIAN_POINT ( 'NONE',  ( 125.0492214775786266, -3.505236298600246325, -18.68346056562440793 ) ) ;
#24845 = CARTESIAN_POINT ( 'NONE',  ( 123.8012348109119642, 0.2603800115204892296, -16.42320221600525088 ) ) ;
#24846 = CIRCLE ( 'NONE', #5892, 2.999999999999999556 ) ;
#24847 = CARTESIAN_POINT ( 'NONE',  ( 117.8449348109119938, -1.833838273342659253, -17.42832698103878286 ) ) ;
#24848 = CARTESIAN_POINT ( 'NONE',  ( 126.9733055311760239, -3.110392498322739563, -8.309745536333537075 ) ) ;
#24849 = CARTESIAN_POINT ( 'NONE',  ( 123.6877814775786533, -3.383040157471821630, -19.15922257007629170 ) ) ;
#24850 = CARTESIAN_POINT ( 'NONE',  ( 111.3319081442453182, -5.568102603702657305, -18.34339073538273013 ) ) ;
#24851 = DIRECTION ( 'NONE',  ( 0.000000000000000000, 0.000000000000000000, 1.000000000000000000 ) ) ;
#24852 = DIRECTION ( 'NONE',  ( 0.000000000000000000, 0.000000000000000000, -1.000000000000000000 ) ) ;
#24853 = CARTESIAN_POINT ( 'NONE',  ( 125.5030348109119558, -6.222761293078241884, -8.102969835052219238 ) ) ;
#24854 = EDGE_LOOP ( 'NONE', ( #229, #4554, #12368, #2253 ) ) ;
#24855 = DIRECTION ( 'NONE',  ( 0.000000000000000000, 0.000000000000000000, -1.000000000000000000 ) ) ;
#24856 = AXIS2_PLACEMENT_3D ( 'NONE', #11513, #1894, #18570 ) ;
#24857 = CARTESIAN_POINT ( 'NONE',  ( 120.7947214775786193, -9.261995988541697145, -16.69588392320189030 ) ) ;
#24858 = CARTESIAN_POINT ( 'NONE',  ( 135.3184548109119874, -8.536181032868617180, -18.13822074491315561 ) ) ;
#24859 = ORIENTED_EDGE ( 'NONE', *, *, #6178, .F. ) ;
#24860 = B_SPLINE_SURFACE_WITH_KNOTS ( 'NONE', 3, 3, ( 
 ( #36892, #29164, #5662, #29394, #43305, #16171, #19581, #33462, #12074, #25978 ),
 ( #5999, #5097, #22881, #19012, #39986, #40676, #26767, #15597, #26310, #36775 ),
 ( #19243, #19922, #33808, #16509, #5327, #5546, #1674, #33575, #8983, #32898 ),
 ( #36553, #29500, #2350, #2579, #43414, #19463, #12181, #8752, #9428, #23341 ),
 ( #40218, #33346, #2120, #33126, #30408, #11958, #25856, #1895, #16049, #26082 ),
 ( #29955, #22657, #43870, #39762, #9210, #12642, #15823, #29722, #37225, #43636 ),
 ( #8532, #26538, #12410, #40448, #23119, #36996, #5767, #22434, #19688, #36327 ),
 ( #16282, #30184, #44102, #12867, #3643, #25077, #42409, #37697, #9661, #11173 ) ),
 .UNSPECIFIED., .F., .F., .F.,
 ( 4, 2, 2, 4 ),
 ( 4, 2, 2, 2, 4 ),
 ( 0.000000000000000000, 0.5000000000000000000, 0.7500000000000000000, 1.000000000000000000 ),
 ( 0.000000000000000000, 0.2500000000000000000, 0.5000000000000000000, 0.7500000000000000000, 1.000000000000000000 ),
 .UNSPECIFIED. ) ;
#24861 = EDGE_CURVE ( 'NONE', #38458, #10189, #24796, .T. ) ;
#24862 = FACE_OUTER_BOUND ( 'NONE', #26663, .T. ) ;
#24863 = CARTESIAN_POINT ( 'NONE',  ( 120.7947214775786193, -9.261995988541697145, -16.69588392320189030 ) ) ;
#24864 = CARTESIAN_POINT ( 'NONE',  ( 109.9963952545248134, 0.8980012041604421569, -11.00651665394454071 ) ) ;
#24865 = CARTESIAN_POINT ( 'NONE',  ( 118.9227414775786542, 0.4262465694468514643, -12.03445270309931736 ) ) ;
#24866 = VERTEX_POINT ( 'NONE', #17152 ) ;
#24867 = CARTESIAN_POINT ( 'NONE',  ( 116.1998614775786507, -10.63000616557722466, -14.87417383870573495 ) ) ;
#24868 = LINE ( 'NONE', #21446, #31391 ) ;
#24869 = CARTESIAN_POINT ( 'NONE',  ( 120.9542138145250192, -3.807985514183305664, -19.09877912889402651 ) ) ;
#24870 = DIRECTION ( 'NONE',  ( -1.000000000000000000, 0.000000000000000000, 0.000000000000000000 ) ) ;
#24871 = CARTESIAN_POINT ( 'NONE',  ( 125.6164881442453094, 0.2603800115204892296, -16.42320221600525088 ) ) ;
#24872 = CARTESIAN_POINT ( 'NONE',  ( 55.68041887817022939, -39.85035523279287162, -7.393215200338315363 ) ) ;
#24873 = AXIS2_PLACEMENT_3D ( 'NONE', #31226, #37845, #37628 ) ;
#24874 = CARTESIAN_POINT ( 'NONE',  ( 90.45092582798827152, -25.99489077589524300, -13.39321520033831625 ) ) ;
#24875 = CARTESIAN_POINT ( 'NONE',  ( 121.9859814775786333, 0.2603800115204892296, -16.42320221600525088 ) ) ;
#24877 = CARTESIAN_POINT ( 'NONE',  ( 121.6456214775786293, 0.4262465694468514643, -12.03445270309931736 ) ) ;
#24876 = CARTESIAN_POINT ( 'NONE',  ( 121.8158014775786171, -5.638512984488999180, -18.83840828888717311 ) ) ;
#24878 = CARTESIAN_POINT ( 'NONE',  ( 120.3409081442453044, -8.899110576539710493, -16.42337572283490132 ) ) ;
#24879 = CARTESIAN_POINT ( 'NONE',  ( 125.3223148109119904, 0.3778260857404744377, -12.04688916545782007 ) ) ;
#24880 = CARTESIAN_POINT ( 'NONE',  ( 117.2209414775786485, -7.893985811506177619, -18.51759400769804742 ) ) ;
#24881 = ORIENTED_EDGE ( 'NONE', *, *, #33364, .F. ) ;
#24882 = CARTESIAN_POINT ( 'NONE',  ( 112.2395221536727377, 0.3967854368540359999, -10.50530088663809636 ) ) ;
#24883 = CARTESIAN_POINT ( 'NONE',  ( 114.1635827545248389, -2.477300249445798297, -19.15521520033831138 ) ) ;
#24884 = CARTESIAN_POINT ( 'NONE',  ( 114.7192077545248594, -2.791137627527939813, -18.39754474579286025 ) ) ;
#24885 = AXIS2_PLACEMENT_3D ( 'NONE', #30618, #2336, #34252 ) ;
#24886 = CARTESIAN_POINT ( 'NONE',  ( 110.3436608795247764, -1.325403438956436419, -16.93181055722141792 ) ) ;
#24887 = CARTESIAN_POINT ( 'NONE',  ( 113.1912390045248031, -9.868328341294098749, -11.32035403202665869 ) ) ;
#24888 = CARTESIAN_POINT ( 'NONE',  ( 125.6732148109119862, 0.5811942927096110934, -14.16772938898807510 ) ) ;
#24889 = CARTESIAN_POINT ( 'NONE',  ( 125.7299414775786346, -10.15424416112533912, -14.75197769757731336 ) ) ;
#24890 = ORIENTED_EDGE ( 'NONE', *, *, #14485, .T. ) ;
#24891 = CARTESIAN_POINT ( 'NONE',  ( 114.7816948109119863, -9.859900752359374465, -12.68260735090039404 ) ) ;
#24892 = CARTESIAN_POINT ( 'NONE',  ( 109.9963952545248134, 0.8980012041604421569, -11.00651665394454071 ) ) ;
#24893 = CARTESIAN_POINT ( 'NONE',  ( 118.9794681442453026, -0.8288870151387751628, -10.36305467784173118 ) ) ;
#24894 = LINE ( 'NONE', #42677, #12359 ) ;
#24895 = CARTESIAN_POINT ( 'NONE',  ( 125.7866681442452688, -0.4660016031367893996, -10.09054647747474043 ) ) ;
#24896 = CARTESIAN_POINT ( 'NONE',  ( 79.31152370492512205, 5.005448908239999994, -6.165396227893437775 ) ) ;
#24897 = CARTESIAN_POINT ( 'NONE',  ( 117.7314814775786260, -4.089484607189486809, -7.948022111789456723 ) ) ;
#24898 = CARTESIAN_POINT ( 'NONE',  ( 114.4413952545248350, 0.8980012041604421569, -11.00651665394454071 ) ) ;
#24899 = CARTESIAN_POINT ( 'NONE',  ( 111.5243640045248412, 0.1403307496149616695, -15.46607636864997204 ) ) ;
#24900 = ORIENTED_EDGE ( 'NONE', *, *, #5394, .F. ) ;
#24901 = CARTESIAN_POINT ( 'NONE',  ( 126.8396850857720324, -7.259892949939295015, -8.653599086628718240 ) ) ;
#24902 = CARTESIAN_POINT ( 'NONE',  ( 115.9162281442453235, -5.574606645277164318, -18.38911715685844683 ) ) ;
#24903 = CARTESIAN_POINT ( 'NONE',  ( 114.3278814775786429, -10.30919188438810075, -12.61870101168855918 ) ) ;
#24904 = CARTESIAN_POINT ( 'NONE',  ( 112.8529881442453302, -1.561330072975668060, -17.79121239304076596 ) ) ;
#24905 = CARTESIAN_POINT ( 'NONE',  ( 123.6310548109119765, -4.153390946401325223, -8.397313243818185668 ) ) ;
#24906 = CARTESIAN_POINT ( 'NONE',  ( 118.8660148109119774, 0.1319031606808879209, -14.10382304977623669 ) ) ;
#24907 = CARTESIAN_POINT ( 'NONE',  ( 112.1722681442453222, -8.899110576539710493, -16.42337572283490132 ) ) ;
#24908 = ORIENTED_EDGE ( 'NONE', *, *, #18083, .T. ) ;
#24909 = CARTESIAN_POINT ( 'NONE',  ( 124.8790414775786246, -8.899110576539710493, -16.42337572283490132 ) ) ;
#24910 = VECTOR ( 'NONE', #15261, 1000.000000000000000 ) ;
#24911 = EDGE_CURVE ( 'NONE', #5770, #30504, #44970, .T. ) ;
#24912 = CARTESIAN_POINT ( 'NONE',  ( 121.4937273908105908, -2.443475742715334853, -17.86549347949429389 ) ) ;
#24913 = CARTESIAN_POINT ( 'NONE',  ( 112.7962614775786676, -6.222761293078241884, -8.102969835052219238 ) ) ;
#24914 = ORIENTED_EDGE ( 'NONE', *, *, #43534, .F. ) ;
#24915 = CARTESIAN_POINT ( 'NONE',  ( 126.2184548109090940, -8.862178061931365036, -16.39564131203211517 ) ) ;
#24916 = CARTESIAN_POINT ( 'NONE',  ( 106.6626452545248611, 0.8980012041604421569, -11.00651665394454071 ) ) ;
#24917 = CARTESIAN_POINT ( 'NONE',  ( 112.7050671295247923, 0.1403307496149613920, -13.39321520033831447 ) ) ;
#24918 = CARTESIAN_POINT ( 'NONE',  ( 125.3895814775786448, -2.084020599724406786, -8.691656652584148546 ) ) ;
#24919 = VECTOR ( 'NONE', #23090, 1000.000000000000000 ) ;
#24920 = EDGE_LOOP ( 'NONE', ( #30776, #8602, #6015, #22164 ) ) ;
#24921 = CARTESIAN_POINT ( 'NONE',  ( 119.3765548109119834, -10.15424416112533912, -14.75197769757731336 ) ) ;
#24922 = CARTESIAN_POINT ( 'NONE',  ( 117.5045748109119756, -9.859900752359374465, -12.68260735090039404 ) ) ;
#24923 = LINE ( 'NONE', #14890, #11260 ) ;
#24924 = CARTESIAN_POINT ( 'NONE',  ( 122.5910329359119970, -4.283928203966213211, -7.183505701512925334 ) ) ;
#24925 = ORIENTED_EDGE ( 'NONE', *, *, #37870, .T. ) ;
#24926 = DIRECTION ( 'NONE',  ( 0.000000000000000000, 0.000000000000000000, -1.000000000000000000 ) ) ;
#24927 = CARTESIAN_POINT ( 'NONE',  ( 125.0849378844200714, -0.4913414945001060574, -7.311231363296191610 ) ) ;
#24928 = CARTESIAN_POINT ( 'NONE',  ( 109.0240515045248202, -2.477300249445798297, -7.631215200338321125 ) ) ;
#24929 = CARTESIAN_POINT ( 'NONE',  ( 117.1373561229423217, -11.24370064073201902, -21.77221270345598825 ) ) ;
#24930 = CARTESIAN_POINT ( 'NONE',  ( 113.3635281442453504, -9.988377603198976828, -10.36322818467138340 ) ) ;
#24931 = CARTESIAN_POINT ( 'NONE',  ( 115.9162281442453093, -5.574606645277164318, -18.38911715685844683 ) ) ;
#24932 = DIRECTION ( 'NONE',  ( 0.000000000000000000, -0.6004852223388322807, 0.7996358532186280677 ) ) ;
#24933 = ORIENTED_EDGE ( 'NONE', *, *, #17248, .T. ) ;
#24934 = CARTESIAN_POINT ( 'NONE',  ( 116.9373081442452929, -1.833838273342659253, -17.42832698103878286 ) ) ;
#24935 = AXIS2_PLACEMENT_3D ( 'NONE', #36666, #30293, #11847 ) ;
#24936 = CARTESIAN_POINT ( 'NONE',  ( 115.3442858795247759, -0.7896495226426338832, -17.46756447353520159 ) ) ;
#24937 = VECTOR ( 'NONE', #39466, 1000.000000000000000 ) ;
#24938 = CARTESIAN_POINT ( 'NONE',  ( 125.1344018827933411, -1.272282569755609494, -16.92713242264453655 ) ) ;
#24939 = CARTESIAN_POINT ( 'NONE',  ( 116.6493314740559413, -1.081026697600512732, -17.18181821144401056 ) ) ;
#24940 = CARTESIAN_POINT ( 'NONE',  ( 114.2711548109119803, -9.988377603198976828, -10.36322818467138340 ) ) ;
#24941 = VERTEX_POINT ( 'NONE', #18256 ) ;
#24942 = CARTESIAN_POINT ( 'NONE',  ( 117.2776681442452968, -5.638512984488999180, -18.83840828888717311 ) ) ;
#24943 = CARTESIAN_POINT ( 'NONE',  ( 114.5547881442453217, -5.638512984488999180, -18.83840828888717311 ) ) ;
#24944 = CARTESIAN_POINT ( 'NONE',  ( 111.3854577545248645, -7.250697342233347165, -7.631215200338321125 ) ) ;
#24945 = CARTESIAN_POINT ( 'NONE',  ( 126.2404814775786264, -0.8288870151387760510, -10.36305467784173118 ) ) ;
#24946 = CARTESIAN_POINT ( 'NONE',  ( 115.2355081442453155, -10.30919188438810075, -12.61870101168855918 ) ) ;
#24947 = AXIS2_PLACEMENT_3D ( 'NONE', #21824, #22493, #36168 ) ;
#24948 = LINE ( 'NONE', #21752, #12617 ) ;
#24949 = CARTESIAN_POINT ( 'NONE',  ( 111.6379010812576809, -0.01829820670803256055, -12.14321520033831625 ) ) ;
#24950 = CARTESIAN_POINT ( 'NONE',  ( 111.9410827545248708, -6.936859964151250502, -8.388885654883777576 ) ) ;
#24951 = EDGE_LOOP ( 'NONE', ( #14483, #13622, #43282 ) ) ;
#24952 = AXIS2_PLACEMENT_3D ( 'NONE', #22339, #681, #38986 ) ;
#24953 = DIRECTION ( 'NONE',  ( 1.000000000000000000, 0.000000000000000000, 0.000000000000000000 ) ) ;
#24954 = CARTESIAN_POINT ( 'NONE',  ( 109.2294425607255164, -3.087680864912572432, -18.17836862529099307 ) ) ;
#24955 = CARTESIAN_POINT ( 'NONE',  ( 117.7882081442453170, -3.505236298600246325, -18.68346056562440793 ) ) ;
#24956 = CARTESIAN_POINT ( 'NONE',  ( 64.43454729525839753, -13.05486520922822713, -11.18801556346294390 ) ) ;
#24957 = CARTESIAN_POINT ( 'NONE',  ( 118.0718414775786300, -9.261995988541702474, -16.69588392320188319 ) ) ;
#24958 = CARTESIAN_POINT ( 'NONE',  ( 107.4960827545248350, -2.477300249445798297, -19.15521520033831138 ) ) ;
#24959 = LINE ( 'NONE', #38618, #14532 ) ;
#24960 = CARTESIAN_POINT ( 'NONE',  ( 115.9162281442453093, -5.574606645277164318, -18.38911715685844683 ) ) ;
#24961 = CARTESIAN_POINT ( 'NONE',  ( 135.3184548109119874, 1.087851763053662602, -12.63461456455805276 ) ) ;
#24962 = CARTESIAN_POINT ( 'NONE',  ( 123.5743281442453139, -7.893985811506177619, -18.51759400769804742 ) ) ;
#24963 = CARTESIAN_POINT ( 'NONE',  ( 117.3911214775786505, -1.561330072975668504, -17.79121239304076951 ) ) ;
#24964 = EDGE_LOOP ( 'NONE', ( #11382, #37937, #22152, #2562, #33600, #8380, #44387, #36729 ) ) ;
#24965 = CARTESIAN_POINT ( 'NONE',  ( 114.4980614775786734, -2.084020599724406786, -8.691656652584148546 ) ) ;
#24966 = CARTESIAN_POINT ( 'NONE',  ( 112.0020881442453344, 0.2603800115204892296, -16.42320221600525088 ) ) ;
#24967 = CARTESIAN_POINT ( 'NONE',  ( 116.9940348109119839, -9.988377603198976828, -10.36322818467138340 ) ) ;
#24968 = CARTESIAN_POINT ( 'NONE',  ( 116.4834948109119779, -7.894159318335828068, -9.358103419637847864 ) ) ;
#24969 = ORIENTED_EDGE ( 'NONE', *, *, #21716, .F. ) ;
#24970 = CARTESIAN_POINT ( 'NONE',  ( 121.9292548109119849, -7.894159318335828068, -9.358103419637847864 ) ) ;
#24971 = AXIS2_PLACEMENT_3D ( 'NONE', #36223, #12073, #25976 ) ;
#24972 = AXIS2_PLACEMENT_3D ( 'NONE', #44820, #44595, #20423 ) ;
#24973 = CARTESIAN_POINT ( 'NONE',  ( 115.2355081442453155, -10.30919188438810075, -12.61870101168855918 ) ) ;
#24974 = CARTESIAN_POINT ( 'NONE',  ( 137.2016500469330538, 0.1791020294301809146, -15.04270252157057719 ) ) ;
#24975 = CARTESIAN_POINT ( 'NONE',  ( 110.4825671295247815, -10.62599879583958540, -13.39321520033831447 ) ) ;
#24976 = CARTESIAN_POINT ( 'NONE',  ( -7.917624645353497748, -12.21642755857638818, -8.593215200338315540 ) ) ;
#24977 = CARTESIAN_POINT ( 'NONE',  ( 126.4168230350732358, 0.2316726006529284954, -13.58249618387747581 ) ) ;
#24978 = CARTESIAN_POINT ( 'NONE',  ( 115.8304577545247582, -2.791137627527939813, -18.39754474579286025 ) ) ;
#24979 = VECTOR ( 'NONE', #12884, 1000.000000000000000 ) ;
#24980 = CARTESIAN_POINT ( 'NONE',  ( 113.9307948109119906, 0.9020085738987339008, -11.91225656197089222 ) ) ;
#24981 = CARTESIAN_POINT ( 'NONE',  ( 117.2294421295247986, 1.224656517226988761, -5.142251848794600733 ) ) ;
#24982 = CARTESIAN_POINT ( 'NONE',  ( 115.0086014775786509, -5.574606645277164318, -18.38911715685844683 ) ) ;
#24983 = CARTESIAN_POINT ( 'NONE',  ( 111.3178276191212888, 0.4261359969230590905, -12.14321520033830026 ) ) ;
#24984 = CARTESIAN_POINT ( 'NONE',  ( 66.50565249108366572, -35.53029877516337365, -12.39321520033831447 ) ) ;
#24985 = CARTESIAN_POINT ( 'NONE',  ( 114.1635827545248389, -6.936859964151250502, -8.388885654883777576 ) ) ;
#24986 = CARTESIAN_POINT ( 'NONE',  ( 114.3846081442453197, 0.4262465694468514643, -12.03445270309931736 ) ) ;
#24987 = DIRECTION ( 'NONE',  ( 0.7962509850245451659, 0.6049664196031394603, 0.000000000000000000 ) ) ;
#24988 = CARTESIAN_POINT ( 'NONE',  ( 60.06931813437629586, -14.72076136720887085, -18.18301750815651374 ) ) ;
#24990 = CARTESIAN_POINT ( 'NONE',  ( 118.5823814775786360, -1.834011780172310813, -8.268836392978581529 ) ) ;
#24989 = DIRECTION ( 'NONE',  ( 0.9908103287288504424, -0.1352586133457950035, 0.000000000000000000 ) ) ;
#24991 = FACE_OUTER_BOUND ( 'NONE', #12645, .T. ) ;
#24992 = CARTESIAN_POINT ( 'NONE',  ( 120.7947214775786193, -0.8288870151387760510, -10.36305467784173118 ) ) ;
#24993 = CARTESIAN_POINT ( 'NONE',  ( 125.5597614775786326, -1.561330072975669392, -17.79121239304076951 ) ) ;
#24994 = ORIENTED_EDGE ( 'NONE', *, *, #6377, .F. ) ;
#24995 = DIRECTION ( 'NONE',  ( -0.6383198453882299450, -0.7697712484781087383, -9.200178928217186715E-17 ) ) ;
#24996 = CARTESIAN_POINT ( 'NONE',  ( 122.0427081442452817, 0.5811942927096110934, -14.16772938898807510 ) ) ;
#24997 = CARTESIAN_POINT ( 'NONE',  ( 116.0388171295248014, 0.1403307496149613920, -13.39321520033831447 ) ) ;
#24998 = CARTESIAN_POINT ( 'NONE',  ( 120.4543614775786295, -5.574606645277164318, -18.38911715685844683 ) ) ;
#25000 = CARTESIAN_POINT ( 'NONE',  ( 117.5045748109119756, -9.859900752359374465, -12.68260735090039404 ) ) ;
#24999 = VECTOR ( 'NONE', #18628, 1000.000000000000000 ) ;
#25001 = CARTESIAN_POINT ( 'NONE',  ( 94.86797725101196477, -26.19000531189954728, -14.26966130367462426 ) ) ;
#25002 = CARTESIAN_POINT ( 'NONE',  ( 113.8163171295247764, -10.62599879583958540, -13.39321520033831447 ) ) ;
#25003 = CARTESIAN_POINT ( 'NONE',  ( 121.3619881442452879, -5.574606645277164318, -18.38911715685844683 ) ) ;
#25004 = VECTOR ( 'NONE', #22095, 1000.000000000000000 ) ;
#25005 = CARTESIAN_POINT ( 'NONE',  ( 125.6164881442453094, -9.565557343593413364, -10.61323700422348004 ) ) ;
#25006 = CARTESIAN_POINT ( 'NONE',  ( 109.2295803840910509, -1.953966997837194963, -8.791361225266440371 ) ) ;
#25007 = CARTESIAN_POINT ( 'NONE',  ( 121.5492360609119800, -3.387241619883791355, -18.17469012370385073 ) ) ;
#25008 = CARTESIAN_POINT ( 'NONE',  ( 113.4690515045247992, -2.477300249445798297, -7.631215200338321125 ) ) ;
#25009 = EDGE_CURVE ( 'NONE', #29964, #18680, #42277, .T. ) ;
#25010 = CARTESIAN_POINT ( 'NONE',  ( 116.4462812948059707, 2.227954574770207863, -20.42202840589934709 ) ) ;
#25011 = CARTESIAN_POINT ( 'NONE',  ( 116.2565881442452991, -9.261995988541697145, -16.69588392320189030 ) ) ;
#25012 = CARTESIAN_POINT ( 'NONE',  ( 113.8740681442453138, 0.5811942927096154232, -14.16772938898807155 ) ) ;
#25013 = CARTESIAN_POINT ( 'NONE',  ( 112.5661608795247872, -8.938348069036489818, -9.318865927141430916 ) ) ;
#25014 = CARTESIAN_POINT ( 'NONE',  ( 113.7606148109119886, -1.561330072975668060, -17.79121239304076596 ) ) ;
#25015 = ORIENTED_EDGE ( 'NONE', *, *, #32499, .T. ) ;
#25016 = CARTESIAN_POINT ( 'NONE',  ( 135.3184548109119874, -4.863998795839242995, -13.39321520033831447 ) ) ;
#25017 = VECTOR ( 'NONE', #29120, 1000.000000000000000 ) ;
#25018 = CARTESIAN_POINT ( 'NONE',  ( 124.1983214775786166, -8.166667518702819706, -8.995218007635861213 ) ) ;
#25019 = CARTESIAN_POINT ( 'NONE',  ( 115.8027748109119841, -0.4660016031367893996, -10.09054647747474043 ) ) ;
#25020 = CARTESIAN_POINT ( 'NONE',  ( 123.2906948109119867, -1.833838273342659697, -17.42832698103878286 ) ) ;
#25021 = CARTESIAN_POINT ( 'NONE',  ( 112.2289948109119848, -7.643976991954077427, -18.09477374809248928 ) ) ;
#25022 = CARTESIAN_POINT ( 'NONE',  ( 123.4608748109119745, -10.63000616557722466, -14.87417383870573495 ) ) ;
#25023 = ADVANCED_FACE ( 'NONE', ( #14385 ), #20452, .T. ) ;
#25024 = CARTESIAN_POINT ( 'NONE',  ( 112.4967077545247633, -7.250697342233347165, -7.631215200338321125 ) ) ;
#25025 = CARTESIAN_POINT ( 'NONE',  ( 116.6536748109119941, -10.15424416112533912, -14.75197769757731336 ) ) ;
#25026 = DIRECTION ( 'NONE',  ( 1.000000000000000000, 0.000000000000000000, -0.000000000000000000 ) ) ;
#25027 = ORIENTED_EDGE ( 'NONE', *, *, #14710, .F. ) ;
#25028 = CARTESIAN_POINT ( 'NONE',  ( 120.2274548109119934, 0.5811942927096110934, -14.16772938898807510 ) ) ;
#25029 = EDGE_CURVE ( 'NONE', #13571, #27865, #4335, .T. ) ;
#25030 = VECTOR ( 'NONE', #7280, 1000.000000000000000 ) ;
#25031 = CARTESIAN_POINT ( 'NONE',  ( 120.0212673109119805, -9.289237151508434209, -11.05642687123711276 ) ) ;
#25032 = ADVANCED_FACE ( 'NONE', ( #14839 ), #758, .F. ) ;
#25033 = CARTESIAN_POINT ( 'NONE',  ( 118.3554748109119998, 0.2603800115204892296, -16.42320221600525088 ) ) ;
#25034 = ORIENTED_EDGE ( 'NONE', *, *, #5771, .T. ) ;
#25035 = CARTESIAN_POINT ( 'NONE',  ( 106.1070202545248407, 0.1403307496149616695, -11.32035403202665336 ) ) ;
#25036 = DIRECTION ( 'NONE',  ( -0.000000000000000000, -0.9284778069183721172, -0.3713878862591650232 ) ) ;
#25037 = DIRECTION ( 'NONE',  ( 0.9908103287288504424, -0.1352586133457950590, 0.000000000000000000 ) ) ;
#25038 = CARTESIAN_POINT ( 'NONE',  ( 117.1074881442453233, 0.4262465694468514643, -12.03445270309931736 ) ) ;
#25039 = CARTESIAN_POINT ( 'NONE',  ( 65.96249443994719286, -37.38467533475423465, -4.893215200338314474 ) ) ;
#25040 = CARTESIAN_POINT ( 'NONE',  ( 64.35098164443778046, -35.92212675331819582, -5.786495942213375265 ) ) ;
#25041 = CARTESIAN_POINT ( 'NONE',  ( 118.4122014775786340, -9.859900752359374465, -12.68260735090039404 ) ) ;
#25042 = CARTESIAN_POINT ( 'NONE',  ( 121.3052614775786395, -1.834011780172307704, -8.268836392978586858 ) ) ;
#25043 = EDGE_CURVE ( 'NONE', #12184, #21045, #38534, .T. ) ;
#25044 = CARTESIAN_POINT ( 'NONE',  ( 122.2128881442453263, -7.643976991954077427, -18.09477374809248928 ) ) ;
#25045 = AXIS2_PLACEMENT_3D ( 'NONE', #21060, #31542, #28355 ) ;
#25046 = CARTESIAN_POINT ( 'NONE',  ( 124.4646854081411504, -12.39265241589126987, -10.94766876842672332 ) ) ;
#25047 = CARTESIAN_POINT ( 'NONE',  ( 119.3765548109119834, -10.15424416112533912, -14.75197769757731336 ) ) ;
#25048 = ADVANCED_FACE ( 'NONE', ( #21675 ), #6604, .T. ) ;
#25049 = CARTESIAN_POINT ( 'NONE',  ( 112.1722681442453222, -0.4660016031367893996, -10.09054647747474043 ) ) ;
#25050 = CARTESIAN_POINT ( 'NONE',  ( 119.6034614775786196, -6.344957434206665248, -7.627207830600338134 ) ) ;
#25051 = CARTESIAN_POINT ( 'NONE',  ( 126.0135748109119902, -1.833838273342660141, -17.42832698103878286 ) ) ;
#25052 = DIRECTION ( 'NONE',  ( -0.9609149988134837450, 0.1028163501681639419, -0.2570431154366518145 ) ) ;
#25053 = EDGE_CURVE ( 'NONE', #39963, #21924, #10966, .T. ) ;
#25054 = ADVANCED_FACE ( 'NONE', ( #29188 ), #4561, .T. ) ;
#25055 = CARTESIAN_POINT ( 'NONE',  ( 121.4754414775786131, -1.833838273342659697, -17.42832698103878286 ) ) ;
#25056 = ORIENTED_EDGE ( 'NONE', *, *, #13941, .F. ) ;
#25057 = CARTESIAN_POINT ( 'NONE',  ( 117.9016614775786280, -9.988377603198976828, -10.36322818467138340 ) ) ;
#25058 = CARTESIAN_POINT ( 'NONE',  ( 115.8304577545247582, -2.791137627527939813, -18.39754474579286025 ) ) ;
#25059 = CARTESIAN_POINT ( 'NONE',  ( 71.02242295334774269, -53.19601237546052630, -37.58603632025644714 ) ) ;
#25060 = CARTESIAN_POINT ( 'NONE',  ( 70.19189222814998175, -61.90193818873174791, -37.96356864969668266 ) ) ;
#25061 = CARTESIAN_POINT ( 'NONE',  ( 68.07789357685331311, -68.58957386525776201, -38.44539312525988350 ) ) ;
#25062 = CARTESIAN_POINT ( 'NONE',  ( 124.9924948109119924, -4.089484607189486809, -7.948022111789456723 ) ) ;
#25063 = ORIENTED_EDGE ( 'NONE', *, *, #21716, .T. ) ;
#25064 = LINE ( 'NONE', #31006, #9626 ) ;
#25065 = CARTESIAN_POINT ( 'NONE',  ( 121.1350814775786233, -9.859900752359378018, -12.68260735090039759 ) ) ;
#25066 = CARTESIAN_POINT ( 'NONE',  ( 59.75121349346655109, -13.58877957849837692, -19.38162691376808411 ) ) ;
#25067 = CARTESIAN_POINT ( 'NONE',  ( 65.01222975847794316, -15.66120467700027064, -17.43105922203487523 ) ) ;
#25068 = CARTESIAN_POINT ( 'NONE',  ( 120.3024188928271059, -8.278628333885235335, -17.13983228602121045 ) ) ;
#25069 = VECTOR ( 'NONE', #34877, 1000.000000000000000 ) ;
#25070 = CARTESIAN_POINT ( 'NONE',  ( 113.8857702545248003, 0.1403307496149616695, -11.32035403202665336 ) ) ;
#25071 = ORIENTED_EDGE ( 'NONE', *, *, #8947, .T. ) ;
#25072 = CARTESIAN_POINT ( 'NONE',  ( 114.2711548109119803, -9.988377603198976828, -10.36322818467138340 ) ) ;
#25073 = CARTESIAN_POINT ( 'NONE',  ( 114.2144281442453178, -8.166667518702817929, -8.995218007635859436 ) ) ;
#25074 = CARTESIAN_POINT ( 'NONE',  ( 125.5597614775786326, -1.561330072975669392, -17.79121239304076951 ) ) ;
#25075 = CARTESIAN_POINT ( 'NONE',  ( 120.0005481442453146, -4.153390946401325223, -8.397313243818185668 ) ) ;
#25076 = CARTESIAN_POINT ( 'NONE',  ( 112.2289948109119848, -7.643976991954077427, -18.09477374809248928 ) ) ;
#25077 = CARTESIAN_POINT ( 'NONE',  ( 68.68839935636917460, -25.95913848132418522, -5.893215200338315363 ) ) ;
#25078 = CARTESIAN_POINT ( 'NONE',  ( 123.0070614775786169, 0.9020085738987339008, -11.91225656197089222 ) ) ;
#25079 = CARTESIAN_POINT ( 'NONE',  ( 123.9146881442452894, -10.15424416112534978, -14.75197769757730093 ) ) ;
#25080 = PLANE ( 'NONE',  #38299 ) ;
#25081 = CARTESIAN_POINT ( 'NONE',  ( 62.78176453955970970, -64.70373736148800958, -45.96606927953587984 ) ) ;
#25082 = CARTESIAN_POINT ( 'NONE',  ( 125.2194014775786286, 0.1319031606808879209, -14.10382304977623669 ) ) ;
#25083 = ORIENTED_EDGE ( 'NONE', *, *, #9602, .T. ) ;
#25084 = CARTESIAN_POINT ( 'NONE',  ( 119.7434548109119703, 3.382738713931011443, -10.84621265594315176 ) ) ;
#25085 = CARTESIAN_POINT ( 'NONE',  ( 119.9438214775786378, -7.893985811506177619, -18.51759400769804742 ) ) ;
#25086 = CARTESIAN_POINT ( 'NONE',  ( 137.3527759848290657, -9.371214294599425898, -15.91961478861451340 ) ) ;
#25087 = ORIENTED_EDGE ( 'NONE', *, *, #29223, .T. ) ;
#25088 = CARTESIAN_POINT ( 'NONE',  ( 121.4544569107182070, -2.467220198592778413, -17.83387418641524391 ) ) ;
#25089 = B_SPLINE_CURVE_WITH_KNOTS ( 'NONE', 3,
 ( #11539, #19278, #29755, #1482, #43667, #12442, #26343, #25446, #39348, #22017 ),
 .UNSPECIFIED., .F., .F.,
 ( 4, 3, 3, 4 ),
 ( 2.168404344971010024E-18, 0.0002476486541971039844, 0.0004952973025691040062, 0.0009610892161188170019 ),
 .UNSPECIFIED. ) ;
#25090 = CARTESIAN_POINT ( 'NONE',  ( 124.9357681442453014, -1.834011780172310813, -8.268836392978581529 ) ) ;
#25091 = CARTESIAN_POINT ( 'NONE',  ( 73.07463722459043254, -51.99713136313413031, -33.10717255453590013 ) ) ;
#25092 = CARTESIAN_POINT ( 'NONE',  ( 123.2339681442453241, -3.505236298600246325, -18.68346056562440793 ) ) ;
#25093 = AXIS2_PLACEMENT_3D ( 'NONE', #37033, #5802, #12900 ) ;
#25094 = ORIENTED_EDGE ( 'NONE', *, *, #38936, .T. ) ;
#25095 = CARTESIAN_POINT ( 'NONE',  ( 115.2355081442453155, -10.30919188438810075, -12.61870101168855918 ) ) ;
#25096 = DIRECTION ( 'NONE',  ( 1.000000000000000000, 0.000000000000000000, -0.000000000000000000 ) ) ;
#25097 = CARTESIAN_POINT ( 'NONE',  ( 121.0024232127138504, -2.191907684172563986, -18.20049396185734025 ) ) ;
#25098 = DIRECTION ( 'NONE',  ( 1.000000000000000000, 0.000000000000000000, -0.000000000000000000 ) ) ;
#25099 = AXIS2_PLACEMENT_3D ( 'NONE', #24376, #13450, #41048 ) ;
#25100 = CARTESIAN_POINT ( 'NONE',  ( 125.8433948109119456, -1.834011780172310813, -8.268836392978581529 ) ) ;
#25101 = EDGE_CURVE ( 'NONE', #2056, #17567, #29868, .T. ) ;
#25102 = LINE ( 'NONE', #36019, #5842 ) ;
#25103 = DIRECTION ( 'NONE',  ( 0.000000000000000000, 0.000000000000000000, 1.000000000000000000 ) ) ;
#25104 = CARTESIAN_POINT ( 'NONE',  ( 124.8790414775786246, -0.4660016031367893996, -10.09054647747474043 ) ) ;
#25106 = CARTESIAN_POINT ( 'NONE',  ( 122.8936081442453059, -9.565557343593413364, -10.61323700422348004 ) ) ;
#25105 = CARTESIAN_POINT ( 'NONE',  ( 123.9714148109119805, -0.4660016031367893996, -10.09054647747474043 ) ) ;
#25107 = CARTESIAN_POINT ( 'NONE',  ( 123.4608748109119745, 0.4262465694468514643, -12.03445270309931736 ) ) ;
#25108 = DIRECTION ( 'NONE',  ( 1.000000000000000000, 0.000000000000000000, -0.000000000000000000 ) ) ;
#25109 = CARTESIAN_POINT ( 'NONE',  ( 120.9649014775786355, -3.383040157471821630, -19.15922257007629170 ) ) ;
#25110 = ORIENTED_EDGE ( 'NONE', *, *, #12253, .F. ) ;
#25111 = EDGE_CURVE ( 'NONE', #22322, #13343, #25102, .T. ) ;
#25112 = VERTEX_POINT ( 'NONE', #39224 ) ;
#25113 = CARTESIAN_POINT ( 'NONE',  ( 112.1234697116520920, -8.918491192341182483, -16.31914947962552631 ) ) ;
#25114 = CARTESIAN_POINT ( 'NONE',  ( 116.5249890045247980, 0.8980012041604421569, -15.77991374673208469 ) ) ;
#25115 = CARTESIAN_POINT ( 'NONE',  ( 106.0375671295248310, -10.62599879583958540, -13.39321520033831447 ) ) ;
#25116 = CARTESIAN_POINT ( 'NONE',  ( 112.9134265045247645, -2.791137627527939813, -8.388885654883777576 ) ) ;
#25117 = EDGE_CURVE ( 'NONE', #14190, #5770, #11638, .T. ) ;
#25118 = CARTESIAN_POINT ( 'NONE',  ( 126.0703014775786102, -9.988377603198980381, -10.36322818467138518 ) ) ;
#25119 = CARTESIAN_POINT ( 'NONE',  ( 126.2972081442452890, -2.084020599724406786, -8.691656652584148546 ) ) ;
#25120 = ORIENTED_EDGE ( 'NONE', *, *, #38675, .F. ) ;
#25121 = CARTESIAN_POINT ( 'NONE',  ( 111.3780948109119890, -5.574606645277164318, -18.38911715685844683 ) ) ;
#25122 = CARTESIAN_POINT ( 'NONE',  ( 107.0793640045248196, -10.62599879583958717, -11.00651665394454604 ) ) ;
#25123 = PLANE ( 'NONE',  #16134 ) ;
#25124 = EDGE_CURVE ( 'NONE', #36955, #37929, #32034, .T. ) ;
#25125 = CARTESIAN_POINT ( 'NONE',  ( 125.6164881442453094, 0.2603800115204892296, -16.42320221600525088 ) ) ;
#25126 = CARTESIAN_POINT ( 'NONE',  ( 123.8012348109119642, 0.2603800115204892296, -16.42320221600525088 ) ) ;
#25127 = CARTESIAN_POINT ( 'NONE',  ( -13.78505786849281911, -3.796669023460694792, -17.89321520033831447 ) ) ;
#25128 = CARTESIAN_POINT ( 'NONE',  ( 117.3343948109119737, -3.383040157471821630, -19.15922257007629170 ) ) ;
#25129 = CARTESIAN_POINT ( 'NONE',  ( 113.2606921295247702, 0.8980012041604618078, -13.39321520033831447 ) ) ;
#25130 = CARTESIAN_POINT ( 'NONE',  ( 110.3436608795247764, -1.325403438956436419, -16.93181055722141792 ) ) ;
#25131 = VECTOR ( 'NONE', #860, 1000.000000000000227 ) ;
#25132 = VERTEX_POINT ( 'NONE', #18708 ) ;
#25133 = CARTESIAN_POINT ( 'NONE',  ( 116.0286950891469786, 2.331313199634366118, -4.893215200338314474 ) ) ;
#25134 = CARTESIAN_POINT ( 'NONE',  ( 116.4267681442453153, -6.222761293078241884, -8.102969835052219238 ) ) ;
#25135 = CARTESIAN_POINT ( 'NONE',  ( 116.8805814775786445, -6.344957434206662583, -7.627207830600332805 ) ) ;
#25136 = CARTESIAN_POINT ( 'NONE',  ( 112.5693548109119888, -10.63000616557722466, -14.87417383870573495 ) ) ;
#25137 = CARTESIAN_POINT ( 'NONE',  ( 123.8012348109119642, -9.565557343593413364, -10.61323700422348004 ) ) ;
#25138 = UNCERTAINTY_MEASURE_WITH_UNIT (LENGTH_MEASURE( 1.000000000000000082E-05 ), #7965, 'distance_accuracy_value', 'NONE');
#25139 = CARTESIAN_POINT ( 'NONE',  ( 120.5678148109119832, -1.833838273342659253, -17.42832698103878286 ) ) ;
#25140 = CARTESIAN_POINT ( 'NONE',  ( 116.1998614775786507, 0.4262465694468514643, -12.03445270309931736 ) ) ;
#25141 = ORIENTED_EDGE ( 'NONE', *, *, #37359, .T. ) ;
#25142 = CONICAL_SURFACE ( 'NONE', #24383, 5.999999999999997335, 0.4636476090008060935 ) ;
#25143 = CARTESIAN_POINT ( 'NONE',  ( 124.7440798109119697, -7.200787124940443817, -17.81845355600750835 ) ) ;
#25144 = CYLINDRICAL_SURFACE ( 'NONE', #1843, 1.499999999999996225 ) ;
#25145 = CARTESIAN_POINT ( 'NONE',  ( 116.8238548109119819, -5.574606645277164318, -18.38911715685844683 ) ) ;
#25146 = ORIENTED_EDGE ( 'NONE', *, *, #34063, .T. ) ;
#25147 = CARTESIAN_POINT ( 'NONE',  ( 69.36136150295220659, -51.77767972350450520, -30.80909290640445519 ) ) ;
#25148 = CARTESIAN_POINT ( 'NONE',  ( 105.8986608795248401, -8.938348069036489818, -9.318865927141430916 ) ) ;
#25149 = CARTESIAN_POINT ( 'NONE',  ( 115.1359265045248605, -7.250697342233347165, -19.15521520033831138 ) ) ;
#25150 = CARTESIAN_POINT ( 'NONE',  ( 112.3991748109119868, -1.833838273342658809, -17.42832698103878286 ) ) ;
#25151 = ORIENTED_EDGE ( 'NONE', *, *, #8956, .F. ) ;
#25152 = VERTEX_POINT ( 'NONE', #32598 ) ;
#25153 = CARTESIAN_POINT ( 'NONE',  ( 118.4122014775786340, -9.859900752359374465, -12.68260735090039404 ) ) ;
#25154 = CARTESIAN_POINT ( 'NONE',  ( 118.8660148109119774, 0.1319031606808879209, -14.10382304977623669 ) ) ;
#25155 = CYLINDRICAL_SURFACE ( 'NONE', #38910, 4.500000000000003553 ) ;
#25156 = EDGE_CURVE ( 'NONE', #30218, #20552, #12621, .T. ) ;
#25157 = CARTESIAN_POINT ( 'NONE',  ( 123.4939235609119663, 0.6414057260225851653, -11.69287257290600657 ) ) ;
#25158 = EDGE_LOOP ( 'NONE', ( #13682, #30742, #17332, #11349 ) ) ;
#25159 = DIRECTION ( 'NONE',  ( 0.000000000000000000, 0.000000000000000000, -1.000000000000000000 ) ) ;
#25160 = DIRECTION ( 'NONE',  ( -0.9908103287288504424, 0.1352586133457950590, 0.000000000000000000 ) ) ;
#25161 = CARTESIAN_POINT ( 'NONE',  ( 110.8992858795247827, -0.7896495226426338832, -17.46756447353520159 ) ) ;
#25162 = CARTESIAN_POINT ( 'NONE',  ( 117.1361595269186040, -11.24668708007285289, -21.77080567551499968 ) ) ;
#25163 = CARTESIAN_POINT ( 'NONE',  ( 124.9924948109119924, -5.574606645277164318, -18.38911715685844683 ) ) ;
#25164 = CARTESIAN_POINT ( 'NONE',  ( 116.5969481442453031, -9.859900752359374465, -12.68260735090039404 ) ) ;
#25165 = DIRECTION ( 'NONE',  ( 0.000000000000000000, 0.000000000000000000, -1.000000000000000000 ) ) ;
#25166 = ORIENTED_EDGE ( 'NONE', *, *, #5904, .T. ) ;
#25167 = CARTESIAN_POINT ( 'NONE',  ( 116.2565881442453133, -0.8288870151387760510, -10.36305467784173118 ) ) ;
#25168 = CARTESIAN_POINT ( 'NONE',  ( 119.7434548109119845, -0.5379176930699823833, -10.61813817059959142 ) ) ;
#25169 = CARTESIAN_POINT ( 'NONE',  ( 84.86020291624612355, -29.99489077589588959, -12.39321520033831447 ) ) ;
#25170 = CARTESIAN_POINT ( 'NONE',  ( 116.8057029421682813, 0.1954196160062621201, -12.14321520033831625 ) ) ;
#25171 = ADVANCED_FACE ( 'NONE', ( #31702 ), #31925, .T. ) ;
#25172 = CARTESIAN_POINT ( 'NONE',  ( 113.4769814775786330, -10.63000616557722466, -14.87417383870573495 ) ) ;
#25173 = ORIENTED_EDGE ( 'NONE', *, *, #9249, .T. ) ;
#25174 = CARTESIAN_POINT ( 'NONE',  ( 117.9016614775786280, -9.988377603198976828, -10.36322818467138340 ) ) ;
#25175 = CARTESIAN_POINT ( 'NONE',  ( 121.9470836909669913, -27.84333996136784961, -14.15691383771150136 ) ) ;
#25176 = CARTESIAN_POINT ( 'NONE',  ( 109.7185827545247889, -2.477300249445798297, -19.15521520033831138 ) ) ;
#25177 = CARTESIAN_POINT ( 'NONE',  ( 117.3343948109119737, -3.383040157471821630, -19.15922257007629170 ) ) ;
#25178 = CARTESIAN_POINT ( 'NONE',  ( 114.4413348109119823, -9.261995988541697145, -16.69588392320189030 ) ) ;
#25179 = CARTESIAN_POINT ( 'NONE',  ( 126.2455040230450720, -9.855666071798866668, -12.91250244977849526 ) ) ;
#25180 = CARTESIAN_POINT ( 'NONE',  ( 112.1494421295248003, -9.868328341294093420, -13.39321520033836421 ) ) ;
#25181 = DIRECTION ( 'NONE',  ( -0.9908103287288504424, 0.1352586133457958917, 0.000000000000000000 ) ) ;
#25182 = ORIENTED_EDGE ( 'NONE', *, *, #31462, .F. ) ;
#25183 = DIRECTION ( 'NONE',  ( 1.000000000000000000, 0.000000000000000000, -0.000000000000000000 ) ) ;
#25184 = CARTESIAN_POINT ( 'NONE',  ( 109.2294421286841697, -3.110521482657592873, -18.18806147283417474 ) ) ;
#25185 = CARTESIAN_POINT ( 'NONE',  ( 117.1074881442453233, 0.4262465694468514643, -12.03445270309931736 ) ) ;
#25186 = CARTESIAN_POINT ( 'NONE',  ( 65.46440686121715657, -13.61036171439920928, -12.26818186452783266 ) ) ;
#25187 = CIRCLE ( 'NONE', #34628, 2.445500000000004448 ) ;
#25188 = CARTESIAN_POINT ( 'NONE',  ( 115.4137390045248566, -9.868328341294098749, -11.32035403202665869 ) ) ;
#25189 = CARTESIAN_POINT ( 'NONE',  ( 107.1488171295247867, -10.62599879583958540, -13.39321520033831447 ) ) ;
#25190 = DIRECTION ( 'NONE',  ( 0.000000000000000000, 0.9242245927363040847, 0.3818493186865897226 ) ) ;
#25191 = CARTESIAN_POINT ( 'NONE',  ( 114.5547881442453217, -4.153390946401321671, -8.397313243818183892 ) ) ;
#25192 = LINE ( 'NONE', #20873, #14602 ) ;
#25193 = CARTESIAN_POINT ( 'NONE',  ( 123.7445081442452874, -1.561330072975668948, -17.79121239304076951 ) ) ;
#25194 = CARTESIAN_POINT ( 'NONE',  ( 121.5321681442453183, -9.988377603198976828, -10.36322818467138340 ) ) ;
#25195 = ORIENTED_EDGE ( 'NONE', *, *, #28663, .T. ) ;
#25196 = CARTESIAN_POINT ( 'NONE',  ( 113.9875214775786532, -8.899110576539710493, -16.42337572283490132 ) ) ;
#25197 = CARTESIAN_POINT ( 'NONE',  ( 113.3068014775786594, -8.166667518702817929, -8.995218007635859436 ) ) ;
#25199 = EDGE_CURVE ( 'NONE', #8760, #18545, #19685, .T. ) ;
#25198 = CARTESIAN_POINT ( 'NONE',  ( 117.1642148109119859, -9.261995988541697145, -16.69588392320189030 ) ) ;
#25200 = CARTESIAN_POINT ( 'NONE',  ( 119.5467348109119712, -5.574606645277164318, -18.38911715685844683 ) ) ;
#25201 = VERTEX_POINT ( 'NONE', #8445 ) ;
#25202 = CARTESIAN_POINT ( 'NONE',  ( 122.8368814775786291, -7.894159318335828068, -9.358103419637847864 ) ) ;
#25203 = VECTOR ( 'NONE', #978, 1000.000000000000114 ) ;
#25204 = CARTESIAN_POINT ( 'NONE',  ( 121.4754414775786131, -8.166667518702819706, -8.995218007635861213 ) ) ;
#25205 = CARTESIAN_POINT ( 'NONE',  ( 137.3172077154941348, 0.1253259204073826072, -14.86998863374360447 ) ) ;
#25206 = CARTESIAN_POINT ( 'NONE',  ( 108.8156921295247912, 0.8980012041604618078, -13.39321520033831447 ) ) ;
#25207 = DIRECTION ( 'NONE',  ( -0.2768435750659243300, -0.3568721902840674698, 0.8921882507333136481 ) ) ;
#25208 = CARTESIAN_POINT ( 'NONE',  ( 61.63318325272354770, -19.46990085680238636, -19.39321520033831447 ) ) ;
#25209 = CARTESIAN_POINT ( 'NONE',  ( 111.9410827545248708, -6.936859964151250502, -8.388885654883777576 ) ) ;
#25210 = CARTESIAN_POINT ( 'NONE',  ( 114.1009748109119784, -4.089484607189486809, -7.948022111789456723 ) ) ;
#25211 = CARTESIAN_POINT ( 'NONE',  ( 137.2352176311238452, -10.13879886906272887, -13.53006418403055733 ) ) ;
#25212 = CARTESIAN_POINT ( 'NONE',  ( 114.6682414775786469, -7.894159318335828068, -9.358103419637847864 ) ) ;
#25213 = CARTESIAN_POINT ( 'NONE',  ( 119.7434548109119703, -7.476587315910852460, -21.06050163197695824 ) ) ;
#25214 = DIRECTION ( 'NONE',  ( 0.9609149988134837450, -0.1028163501681639419, 0.2570431154366518145 ) ) ;
#25215 = CARTESIAN_POINT ( 'NONE',  ( 112.4272546295247821, -4.863998795839590272, -18.39754474579285315 ) ) ;
#25216 = CARTESIAN_POINT ( 'NONE',  ( 121.9100498793805230, -2.191907684172563986, -18.20049396185734025 ) ) ;
#25217 = SURFACE_STYLE_FILL_AREA ( #32267 ) ;
#25218 = AXIS2_PLACEMENT_3D ( 'NONE', #41276, #30539, #30992 ) ;
#25219 = CARTESIAN_POINT ( 'NONE',  ( 67.30914723170953096, -50.45175545520677929, -34.27804336089664616 ) ) ;
#25221 = CARTESIAN_POINT ( 'NONE',  ( 120.2841814775786276, 0.9020085738987339008, -11.91225656197089222 ) ) ;
#25220 = CARTESIAN_POINT ( 'NONE',  ( 64.85972373664627355, -13.90976778618263410, -9.092962798488864351 ) ) ;
#25222 = EDGE_CURVE ( 'NONE', #19524, #23245, #43711, .T. ) ;
#25223 = CARTESIAN_POINT ( 'NONE',  ( 120.3409081442453044, -8.899110576539710493, -16.42337572283490132 ) ) ;
#25224 = CARTESIAN_POINT ( 'NONE',  ( 126.0135748109119902, -8.166667518702819706, -8.995218007635861213 ) ) ;
#25225 = VERTEX_POINT ( 'NONE', #11869 ) ;
#25226 = CARTESIAN_POINT ( 'NONE',  ( 136.4173705901494316, -7.083541812144162897, -8.051131675560494472 ) ) ;
#25227 = CARTESIAN_POINT ( 'NONE',  ( 124.4819548109119722, -7.893985811506177619, -18.51759400769804742 ) ) ;
#25228 = CARTESIAN_POINT ( 'NONE',  ( 116.1777233795247781, -1.325403438956436419, -9.854619843455211026 ) ) ;
#25229 = CARTESIAN_POINT ( 'NONE',  ( 118.0151148109119816, 0.4262465694468514643, -12.03445270309931736 ) ) ;
#25230 = CIRCLE ( 'NONE', #4088, 3.500000000000003109 ) ;
#25231 = CARTESIAN_POINT ( 'NONE',  ( 114.8951481442453115, -8.899110576539710493, -16.42337572283490132 ) ) ;
#25232 = CARTESIAN_POINT ( 'NONE',  ( 85.91347875220176888, -27.44380683465356441, -8.664846435848167161 ) ) ;
#25233 = CARTESIAN_POINT ( 'NONE',  ( 113.2606921295247702, 0.8980012041604618078, -13.39321520033831447 ) ) ;
#25234 = CARTESIAN_POINT ( 'NONE',  ( 121.8725281442453223, -6.222761293078241884, -8.102969835052219238 ) ) ;
#25235 = CARTESIAN_POINT ( 'NONE',  ( 125.5030348109119558, -6.222761293078241884, -8.102969835052219238 ) ) ;
#25236 = CARTESIAN_POINT ( 'NONE',  ( 116.3860827545247787, -6.936859964151197211, -8.388885654883754484 ) ) ;
#25237 = CARTESIAN_POINT ( 'NONE',  ( 109.2294653279517149, -0.7726726615477512716, -9.908608680919114065 ) ) ;
#25238 = CARTESIAN_POINT ( 'NONE',  ( 123.6328298109119714, -2.173413727453600508, -8.297982527556802879 ) ) ;
#25239 = CARTESIAN_POINT ( 'NONE',  ( 114.5108483795247878, -0.7896495226426338832, -9.318865927141430916 ) ) ;
#25240 = PRODUCT_DEFINITION_SHAPE ( 'NONE', 'NONE',  #7964 ) ;
#25241 = CARTESIAN_POINT ( 'NONE',  ( 76.69189222814998175, -45.49566950204133065, -19.39321520033831447 ) ) ;
#25242 = CARTESIAN_POINT ( 'NONE',  ( 83.96621166889828203, -31.47958770101378434, -20.89321520034811641 ) ) ;
#25243 = CARTESIAN_POINT ( 'NONE',  ( 116.5969481442453031, 0.5811942927096154232, -14.16772938898807155 ) ) ;
#25244 = CARTESIAN_POINT ( 'NONE',  ( 119.4332814775786318, -0.4660016031367893996, -10.09054647747474043 ) ) ;
#25245 = CARTESIAN_POINT ( 'NONE',  ( 109.7880358795247986, -0.7896495226426338832, -17.46756447353520159 ) ) ;
#25246 =( BOUNDED_CURVE ( )  B_SPLINE_CURVE ( 2, ( #190, #11139, #28246, #4734, #18652, #25042, #43045, #8390, #21843, #18870, #864, #25720, #15004, #35275, #28696, #38938, #32094 ),
 .UNSPECIFIED., .F., .T. ) 
 B_SPLINE_CURVE_WITH_KNOTS ( ( 3, 2, 2, 2, 2, 2, 2, 2, 3 ),
 ( 0.6420046674808920217, 0.6484375000000000000, 0.6562500000000000000, 0.6640625000000000000, 0.6718750000000000000, 0.6796875000000000000, 0.6875000000000000000, 0.6953125000000000000, 0.7017453325190590174 ),
 .UNSPECIFIED. ) 
 CURVE ( )  GEOMETRIC_REPRESENTATION_ITEM ( )  RATIONAL_B_SPLINE_CURVE ( ( 0.9778625265006449796, 0.9373222120152220338, 1.000000000000000000, 0.9238795325112869605, 1.000000000000000000, 0.9238795325112869605, 1.000000000000000000, 0.9238795325112869605, 1.000000000000000000, 0.9238795325112869605, 1.000000000000000000, 0.9238795325112869605, 1.000000000000000000, 0.9238795325112869605, 1.000000000000000000, 0.9373222120157009840, 0.9778625265000250311 ) ) 
 REPRESENTATION_ITEM ( '' )  );
#25247 = ORIENTED_EDGE ( 'NONE', *, *, #15010, .T. ) ;
#25248 = CARTESIAN_POINT ( 'NONE',  ( 113.2492419144190592, -1.220279397241706532, -16.99638242193885773 ) ) ;
#25249 = CARTESIAN_POINT ( 'NONE',  ( 115.1787814775786387, -9.988377603198976828, -10.36322818467138340 ) ) ;
#25250 = CARTESIAN_POINT ( 'NONE',  ( 121.3052614775786111, -7.643976991954077427, -18.09477374809248928 ) ) ;
#25251 = CIRCLE ( 'NONE', #5565, 1.499999999999996225 ) ;
#25252 = APPLICATION_PROTOCOL_DEFINITION ( 'draft international standard', 'automotive_design', 1998, #37879 ) ;
#25253 = CARTESIAN_POINT ( 'NONE',  ( 124.4819548109119722, -7.893985811506177619, -18.51759400769804742 ) ) ;
#25254 = CARTESIAN_POINT ( 'NONE',  ( 123.5743281442453139, -7.893985811506177619, -18.51759400769804742 ) ) ;
#25255 = CIRCLE ( 'NONE', #11424, 5.999999999999997335 ) ;
#25256 = CARTESIAN_POINT ( 'NONE',  ( 111.8021765045248372, -7.250697342233347165, -19.15521520033831138 ) ) ;
#25257 = CARTESIAN_POINT ( 'NONE',  ( 116.1998614775786507, 0.4262465694468514643, -12.03445270309931736 ) ) ;
#25258 = CARTESIAN_POINT ( 'NONE',  ( 121.4103298109119748, -2.173413727453600508, -8.297982527556802879 ) ) ;
#25259 = DIRECTION ( 'NONE',  ( -0.000000000000000000, -0.9284778069183721172, -0.3713878862591650232 ) ) ;
#25260 = ORIENTED_EDGE ( 'NONE', *, *, #35036, .F. ) ;
#25261 = AXIS2_PLACEMENT_3D ( 'NONE', #6593, #37367, #33941 ) ;
#25262 = CARTESIAN_POINT ( 'NONE',  ( 120.4379860609119675, -3.387241619883791355, -18.17469012370385073 ) ) ;
#25263 = CARTESIAN_POINT ( 'NONE',  ( 118.8092881442453290, -9.988377603198976828, -10.36322818467138340 ) ) ;
#25264 = VERTEX_POINT ( 'NONE', #9344 ) ;
#25265 = DIRECTION ( 'NONE',  ( 0.9659258262890690894, 0.2588190451025180749, 0.000000000000000000 ) ) ;
#25266 = CARTESIAN_POINT ( 'NONE',  ( 66.31675885524160208, -2.050240359669329937, -8.986641377623520555 ) ) ;
#25267 = DIRECTION ( 'NONE',  ( 0.000000000000000000, 0.9284778069183720062, 0.3713878862591650232 ) ) ;
#25268 = CARTESIAN_POINT ( 'NONE',  ( 114.9518748109119883, -7.643976991954077427, -18.09477374809248928 ) ) ;
#25269 = CARTESIAN_POINT ( 'NONE',  ( 77.24258364551867828, -56.45027166639924587, -1.965605518563571019 ) ) ;
#25270 = CARTESIAN_POINT ( 'NONE',  ( 124.5241427111123755, -9.788830010355399125, -12.52847583010056098 ) ) ;
#25271 = CARTESIAN_POINT ( 'NONE',  ( 118.1285681442453068, -2.084020599724406786, -8.691656652584148546 ) ) ;
#25272 = CARTESIAN_POINT ( 'NONE',  ( 125.4584548109119737, -6.717659058379802595, -19.62329895828877468 ) ) ;
#25273 = CARTESIAN_POINT ( 'NONE',  ( 122.5532481442453019, 0.4262465694468514643, -12.03445270309931736 ) ) ;
#25274 = CARTESIAN_POINT ( 'NONE',  ( 124.0650380271183906, -12.48185142254331836, -10.95032796985108270 ) ) ;
#25275 = CONICAL_SURFACE ( 'NONE', #37644, 0.8509999999999994236, 0.06981317007976593769 ) ;
#25276 = CARTESIAN_POINT ( 'NONE',  ( 123.4041481442452834, 0.1319031606808879209, -14.10382304977623669 ) ) ;
#25277 = CARTESIAN_POINT ( 'NONE',  ( 114.1009748109119784, -4.089484607189486809, -7.948022111789456723 ) ) ;
#25278 = CARTESIAN_POINT ( 'NONE',  ( 120.6245414775786458, -9.988377603198976828, -10.36322818467138340 ) ) ;
#25279 = CARTESIAN_POINT ( 'NONE',  ( 126.6375681442452930, -10.15424416112533912, -14.75197769757731336 ) ) ;
#25280 = CARTESIAN_POINT ( 'NONE',  ( 61.69189222814998175, -69.76310523276724496, -16.89321520033831447 ) ) ;
#25281 = CARTESIAN_POINT ( 'NONE',  ( 122.3263414775786373, -3.505236298600246325, -18.68346056562440793 ) ) ;
#25282 = ORIENTED_EDGE ( 'NONE', *, *, #26130, .F. ) ;
#25283 = CARTESIAN_POINT ( 'NONE',  ( 119.4332814775786318, -0.4660016031367893996, -10.09054647747474043 ) ) ;
#25284 = CARTESIAN_POINT ( 'NONE',  ( 113.8163171295247764, 0.1403307496149613920, -13.39321520033831447 ) ) ;
#25285 = ADVANCED_FACE ( 'NONE', ( #36910 ), #31326, .T. ) ;
#25286 = CIRCLE ( 'NONE', #11463, 5.132259260909266985 ) ;
#25287 = CARTESIAN_POINT ( 'NONE',  ( 115.2922348109119781, 0.4262465694468551280, -12.03445270309932269 ) ) ;
#25288 = FACE_OUTER_BOUND ( 'NONE', #44165, .T. ) ;
#25289 = CARTESIAN_POINT ( 'NONE',  ( 69.36136150295220659, -59.97963455175678860, -34.08984624715239420 ) ) ;
#25290 = CARTESIAN_POINT ( 'NONE',  ( 59.58306117764126952, -13.63527223977064295, -7.397078708827238280 ) ) ;
#25291 = ORIENTED_EDGE ( 'NONE', *, *, #29196, .F. ) ;
#25292 = CARTESIAN_POINT ( 'NONE',  ( 128.2184548109119930, -1.889072916127989776, -18.60376373290417362 ) ) ;
#25293 = CARTESIAN_POINT ( 'NONE',  ( 121.3052614775786111, -7.643976991954077427, -18.09477374809248928 ) ) ;
#25294 = CARTESIAN_POINT ( 'NONE',  ( 121.6186891859119896, -8.844754642576884152, -8.592115655440050404 ) ) ;
#25295 = CARTESIAN_POINT ( 'NONE',  ( 61.00841592940014380, -13.32659487457196335, -19.27059286807817884 ) ) ;
#25296 = VECTOR ( 'NONE', #9978, 999.9999999999998863 ) ;
#25297 = DIRECTION ( 'NONE',  ( -0.5735764363510450492, -0.3127926500124816878, 0.7570804645221038687 ) ) ;
#25298 = EDGE_CURVE ( 'NONE', #13764, #8341, #4381, .T. ) ;
#25299 = CARTESIAN_POINT ( 'NONE',  ( 106.0375671295248310, 0.1403307496149613920, -13.39321520033831447 ) ) ;
#25300 = VERTEX_POINT ( 'NONE', #29413 ) ;
#25301 = CARTESIAN_POINT ( 'NONE',  ( 114.3278814775786429, -10.30919188438810075, -12.61870101168855918 ) ) ;
#25302 = CARTESIAN_POINT ( 'NONE',  ( 115.5191414775786569, -3.383040157471821630, -19.15922257007629170 ) ) ;
#25303 = CARTESIAN_POINT ( 'NONE',  ( 126.2404814775786264, -9.261995988541697145, -16.69588392320189030 ) ) ;
#25304 = CARTESIAN_POINT ( 'NONE',  ( 119.1496481442453046, -6.222761293078241884, -8.102969835052219238 ) ) ;
#25305 = DIRECTION ( 'NONE',  ( 0.000000000000000000, -0.3818493186865936084, 0.9242245927363024194 ) ) ;
#25306 = CARTESIAN_POINT ( 'NONE',  ( 121.5888948109119809, -10.30919188438810075, -12.61870101168855918 ) ) ;
#25307 = CARTESIAN_POINT ( 'NONE',  ( 111.7751814775786556, -2.084020599724406786, -8.691656652584148546 ) ) ;
#25308 = DIRECTION ( 'NONE',  ( -0.7871354856660162103, -0.4483307682966942709, -0.4235767337848251879 ) ) ;
#25309 = CARTESIAN_POINT ( 'NONE',  ( 63.56235174433628998, -1.192518024930046661, -9.408727405721505122 ) ) ;
#25310 = CARTESIAN_POINT ( 'NONE',  ( 112.7395348109119766, -5.638512984488999180, -18.83840828888717311 ) ) ;
#25311 = EDGE_LOOP ( 'NONE', ( #22457, #3489, #28363, #41371 ) ) ;
#25312 = DIRECTION ( 'NONE',  ( 0.000000000000000000, -0.2950959089608191088, 0.9554676365605421218 ) ) ;
#25313 = CIRCLE ( 'NONE', #10029, 2.445500000000004448 ) ;
#25314 = CARTESIAN_POINT ( 'NONE',  ( 119.2063748109119814, -1.561330072975668504, -17.79121239304076951 ) ) ;
#25315 = CARTESIAN_POINT ( 'NONE',  ( 137.4478226697684136, -9.171749513548395072, -16.06665655585063135 ) ) ;
#25316 = VERTEX_POINT ( 'NONE', #39680 ) ;
#25317 = EDGE_CURVE ( 'NONE', #31011, #14190, #36686, .T. ) ;
#25318 = CARTESIAN_POINT ( 'NONE',  ( 111.7751814775786556, -7.893985811506177619, -18.51759400769804742 ) ) ;
#25319 = EDGE_CURVE ( 'NONE', #38775, #19108, #23253, .T. ) ;
#25320 = EDGE_CURVE ( 'NONE', #35019, #9951, #1809, .T. ) ;
#25321 = CARTESIAN_POINT ( 'NONE',  ( 124.8223148109119762, 0.9020085738987339008, -11.91225656197089222 ) ) ;
#25322 = CARTESIAN_POINT ( 'NONE',  ( 111.4549108795247747, -1.325403438956436419, -16.93181055722138595 ) ) ;
#25323 = CARTESIAN_POINT ( 'NONE',  ( 123.6310548109119765, -4.153390946401325223, -8.397313243818185668 ) ) ;
#25324 = VERTEX_POINT ( 'NONE', #12094 ) ;
#25325 = CARTESIAN_POINT ( 'NONE',  ( 118.4689281442453392, 0.9020085738987339008, -11.91225656197089222 ) ) ;
#25326 = DIRECTION ( 'NONE',  ( 1.000000000000000000, 0.000000000000000000, -0.000000000000000000 ) ) ;
#25327 = CYLINDRICAL_SURFACE ( 'NONE', #14219, 3.000000000000001776 ) ;
#25328 = VECTOR ( 'NONE', #37501, 1000.000000000000000 ) ;
#25329 = CARTESIAN_POINT ( 'NONE',  ( 137.2352176311223673, -5.000847779533773796, -8.118415127113269847 ) ) ;
#25330 = CARTESIAN_POINT ( 'NONE',  ( 125.4463081442452932, -5.638512984488999180, -18.83840828888717311 ) ) ;
#25331 = CARTESIAN_POINT ( 'NONE',  ( 69.69189222815028018, -41.76310523276638520, -12.39321520033831447 ) ) ;
#25332 = DIRECTION ( 'NONE',  ( 0.000000000000000000, 0.000000000000000000, -1.000000000000000000 ) ) ;
#25333 = CARTESIAN_POINT ( 'NONE',  ( 124.8223148109119762, 0.9020085738987339008, -11.91225656197089222 ) ) ;
#25334 = CARTESIAN_POINT ( 'NONE',  ( 123.0070614775786169, -10.15424416112533912, -14.75197769757731336 ) ) ;
#25335 = CARTESIAN_POINT ( 'NONE',  ( 116.6298240518509317, -9.627756678427191517, -15.02827327735217544 ) ) ;
#25336 = CARTESIAN_POINT ( 'NONE',  ( 121.8725281442453223, -6.222761293078241884, -8.102969835052219238 ) ) ;
#25337 = CARTESIAN_POINT ( 'NONE',  ( 112.6260814775786514, -0.8288870151387760510, -10.36305467784173118 ) ) ;
#25338 = CARTESIAN_POINT ( 'NONE',  ( 119.6601881442453106, -8.166667518702819706, -8.995218007635861213 ) ) ;
#25339 = ORIENTED_EDGE ( 'NONE', *, *, #10299, .T. ) ;
#25340 = ORIENTED_EDGE ( 'NONE', *, *, #42891, .T. ) ;
#25341 = DIRECTION ( 'NONE',  ( 1.000000000000000000, 0.000000000000000000, -0.000000000000000000 ) ) ;
#25342 = CARTESIAN_POINT ( 'NONE',  ( 125.6732148109119862, -9.859900752359514797, -12.68260735090137459 ) ) ;
#25343 = CARTESIAN_POINT ( 'NONE',  ( 115.5526452545247622, -9.868328341294098749, -15.46607636864997204 ) ) ;
#25344 = CARTESIAN_POINT ( 'NONE',  ( 114.9970202545248412, 0.1403307496149616695, -11.32035403202665336 ) ) ;
#25345 = CARTESIAN_POINT ( 'NONE',  ( 125.0492214775786408, -3.505236298599212041, -18.68346056562414859 ) ) ;
#25346 = CARTESIAN_POINT ( 'NONE',  ( 115.4056881442453459, -7.893985811506177619, -18.51759400769804742 ) ) ;
#25347 = VERTEX_POINT ( 'NONE', #2262 ) ;
#25348 = CARTESIAN_POINT ( 'NONE',  ( 112.1722681442453222, -8.899110576539710493, -16.42337572283490132 ) ) ;
#25349 = CARTESIAN_POINT ( 'NONE',  ( -6.962123463324020101, -11.49046785505261248, -18.19321520033831519 ) ) ;
#25350 = DIRECTION ( 'NONE',  ( 0.9609149988134837450, -0.1028163501681639419, 0.2570431154366518145 ) ) ;
#25351 = CARTESIAN_POINT ( 'NONE',  ( 120.0546248871816317, -6.188980713775695364, -18.62212668298318619 ) ) ;
#25352 = CARTESIAN_POINT ( 'NONE',  ( 109.2294452378115039, 0.04794956319235682551, -14.87050034823130851 ) ) ;
#25353 = CARTESIAN_POINT ( 'NONE',  ( 121.9470836909669913, -25.99489077589524300, -13.39321520033831447 ) ) ;
#25354 = CARTESIAN_POINT ( 'NONE',  ( 115.3489614775786407, -9.261995988541697145, -16.69588392320189030 ) ) ;
#25355 = ADVANCED_FACE ( 'NONE', ( #26000 ), #18926, .T. ) ;
#25356 = CARTESIAN_POINT ( 'NONE',  ( 115.1359265045248605, -7.250697342233347165, -19.15521520033831138 ) ) ;
#25357 = CARTESIAN_POINT ( 'NONE',  ( 113.3995983795247895, -8.402594152722688392, -16.93181055722141792 ) ) ;
#25358 = ORIENTED_EDGE ( 'NONE', *, *, #40533, .F. ) ;
#25359 = CARTESIAN_POINT ( 'NONE',  ( 69.69189222814998175, -41.76310523276723785, -24.39321520033831447 ) ) ;
#25360 = CARTESIAN_POINT ( 'NONE',  ( 119.7736414775786358, 0.1319031606808879209, -14.10382304977623669 ) ) ;
#25361 = CARTESIAN_POINT ( 'NONE',  ( 115.6325948109119821, 0.2603800115204892296, -16.42320221600525088 ) ) ;
#25362 = DIRECTION ( 'NONE',  ( 0.000000000000000000, 0.000000000000000000, -1.000000000000000000 ) ) ;
#25363 = CARTESIAN_POINT ( 'NONE',  ( 124.4252281442452812, -0.8288870151387760510, -10.36305467784173118 ) ) ;
#25364 = CARTESIAN_POINT ( 'NONE',  ( 118.1852948109119836, -4.153390946401325223, -8.397313243818185668 ) ) ;
#25365 = CARTESIAN_POINT ( 'NONE',  ( 116.0296814775786345, -1.833838273342658809, -17.42832698103878286 ) ) ;
#25366 = ORIENTED_EDGE ( 'NONE', *, *, #42558, .T. ) ;
#25367 = CARTESIAN_POINT ( 'NONE',  ( 124.1884548109119777, -2.527210466738041728, -8.967976844669124148 ) ) ;
#25368 = CARTESIAN_POINT ( 'NONE',  ( 94.20708369096698220, -25.17209684859101415, -13.61049647700816401 ) ) ;
#25369 = CARTESIAN_POINT ( 'NONE',  ( 118.9227414775786542, 0.4262465694468514643, -12.03445270309931736 ) ) ;
#25370 = ORIENTED_EDGE ( 'NONE', *, *, #21755, .T. ) ;
#25371 = APPLICATION_CONTEXT ( 'automotive_design' ) ;
#25372 = CARTESIAN_POINT ( 'NONE',  ( 110.6689883310706790, 0.1843591316377651834, -12.14321520033831625 ) ) ;
#25373 = EDGE_CURVE ( 'NONE', #30249, #41341, #40355, .T. ) ;
#25374 = CARTESIAN_POINT ( 'NONE',  ( 114.0442481442453300, -1.834011780172310813, -8.268836392978581529 ) ) ;
#25375 = CARTESIAN_POINT ( 'NONE',  ( 107.9822546295247889, -4.863998795839590272, -18.39754474579285315 ) ) ;
#25376 = FACE_OUTER_BOUND ( 'NONE', #1776, .T. ) ;
#25377 = ORIENTED_EDGE ( 'NONE', *, *, #44678, .T. ) ;
#25378 = ORIENTED_EDGE ( 'NONE', *, *, #2876, .F. ) ;
#25379 = CARTESIAN_POINT ( 'NONE',  ( 121.7590748109119687, -2.084020599724406786, -8.691656652584148546 ) ) ;
#25380 = CIRCLE ( 'NONE', #42139, 2.445500000000001339 ) ;
#25381 = CARTESIAN_POINT ( 'NONE',  ( 115.7460481442453357, -10.15424416112533912, -14.75197769757731336 ) ) ;
#25382 = EDGE_CURVE ( 'NONE', #21884, #17628, #21176, .T. ) ;
#25383 = DIRECTION ( 'NONE',  ( 0.000000000000000000, 0.000000000000000000, 1.000000000000000000 ) ) ;
#25384 = LINE ( 'NONE', #28802, #14049 ) ;
#25385 = ORIENTED_EDGE ( 'NONE', *, *, #5771, .F. ) ;
#25386 = DIRECTION ( 'NONE',  ( 0.2588190451025260685, -0.9659258262890669799, 0.000000000000000000 ) ) ;
#25387 = CARTESIAN_POINT ( 'NONE',  ( 119.7434548109119703, -2.590033228374110763, -8.938908788042002840 ) ) ;
#25388 = CARTESIAN_POINT ( 'NONE',  ( 110.6214733795247867, -8.938348069036489818, -17.46756447353520159 ) ) ;
#25389 = CARTESIAN_POINT ( 'NONE',  ( 112.0588148109119828, 0.5811942927096154232, -14.16772938898807155 ) ) ;
#25390 = CARTESIAN_POINT ( 'NONE',  ( 125.4463081442452932, -4.153390946401325223, -8.397313243818185668 ) ) ;
#25391 = CARTESIAN_POINT ( 'NONE',  ( 121.3052614775786111, -7.643976991954077427, -18.09477374809248928 ) ) ;
#25392 = PLANE ( 'NONE',  #19649 ) ;
#25393 = ORIENTED_EDGE ( 'NONE', *, *, #20393, .T. ) ;
#25394 = CARTESIAN_POINT ( 'NONE',  ( 121.3619881442452879, -5.574606645277164318, -18.38911715685844683 ) ) ;
#25395 = FACE_OUTER_BOUND ( 'NONE', #9128, .T. ) ;
#25396 = CARTESIAN_POINT ( 'NONE',  ( 114.1961422310133685, -1.244021962887382315, -16.96476564598603787 ) ) ;
#25397 = CARTESIAN_POINT ( 'NONE',  ( 115.0664733795247798, -8.938348069036489818, -17.46756447353520159 ) ) ;
#25398 = CARTESIAN_POINT ( 'NONE',  ( 116.8238548109119819, -4.089484607189486809, -7.948022111789456723 ) ) ;
#25399 = ORIENTED_EDGE ( 'NONE', *, *, #15908, .F. ) ;
#25400 = CARTESIAN_POINT ( 'NONE',  ( 115.9162281442453235, -4.089484607189486809, -7.948022111789456723 ) ) ;
#25401 = CARTESIAN_POINT ( 'NONE',  ( 62.36806374128264707, -37.05470338471879188, -5.389733333427170869 ) ) ;
#25402 = CARTESIAN_POINT ( 'NONE',  ( 113.6774108795247997, -8.938348069036489818, -9.318865927141430916 ) ) ;
#25403 = CARTESIAN_POINT ( 'NONE',  ( 117.0507614775786465, -10.30919188438810075, -12.61870101168855918 ) ) ;
#25404 = CARTESIAN_POINT ( 'NONE',  ( 116.1998614775786507, -10.63000616557722466, -14.87417383870573495 ) ) ;
#25405 = CARTESIAN_POINT ( 'NONE',  ( 125.6732148109119862, -9.859900752359378018, -12.68260735090039759 ) ) ;
#25406 = LINE ( 'NONE', #11046, #30055 ) ;
#25407 = FACE_OUTER_BOUND ( 'NONE', #19568, .T. ) ;
#25408 = ORIENTED_EDGE ( 'NONE', *, *, #19220, .F. ) ;
#25409 = DIRECTION ( 'NONE',  ( 0.9609149988134843001, -0.1028163501681632064, 0.2570431154366505933 ) ) ;
#25410 = CARTESIAN_POINT ( 'NONE',  ( 109.2294977741537707, -10.19482194012555176, -11.51702172248756284 ) ) ;
#25411 = CARTESIAN_POINT ( 'NONE',  ( 119.4900081442453086, -7.643976991954077427, -18.09477374809248928 ) ) ;
#25412 = DIRECTION ( 'NONE',  ( 0.000000000000000000, 0.000000000000000000, -1.000000000000000000 ) ) ;
#25413 = CARTESIAN_POINT ( 'NONE',  ( 114.6497546295247929, -4.863998795839590272, -18.39754474579285315 ) ) ;
#25414 = CARTESIAN_POINT ( 'NONE',  ( 113.7468640045248236, 0.1403307496149616695, -15.46607636864997204 ) ) ;
#25415 = CARTESIAN_POINT ( 'NONE',  ( 121.9470836909669913, -25.99489077589524300, -13.39321520033831447 ) ) ;
#25416 = CARTESIAN_POINT ( 'NONE',  ( 115.2355081442453155, 0.1319031606808879209, -14.10382304977623669 ) ) ;
#25417 = DIRECTION ( 'NONE',  ( -1.000000000000000000, 0.000000000000000000, 0.000000000000000000 ) ) ;
#25418 = CARTESIAN_POINT ( 'NONE',  ( 122.1561614775786353, -0.4660016031367893996, -10.09054647747474043 ) ) ;
#25419 = CARTESIAN_POINT ( 'NONE',  ( 118.9794681442453026, -9.261995988541697145, -16.69588392320189030 ) ) ;
#25421 = ORIENTED_EDGE ( 'NONE', *, *, #490, .T. ) ;
#25420 = EDGE_CURVE ( 'NONE', #35973, #3780, #795, .T. ) ;
#25422 = CARTESIAN_POINT ( 'NONE',  ( 119.7169148109119874, -0.1624402480850797581, -16.17319339645315424 ) ) ;
#25423 = CARTESIAN_POINT ( 'NONE',  ( 126.1270281442452870, -10.30919188438810075, -12.61870101168855918 ) ) ;
#25424 = CARTESIAN_POINT ( 'NONE',  ( 117.3911214775786505, -1.561330072975668504, -17.79121239304076951 ) ) ;
#25425 = CARTESIAN_POINT ( 'NONE',  ( 121.1918081442452859, -10.15424416112533912, -14.75197769757731336 ) ) ;
#25426 = ORIENTED_EDGE ( 'NONE', *, *, #13998, .T. ) ;
#25427 = CARTESIAN_POINT ( 'NONE',  ( 124.4252281442452812, -0.8288870151387760510, -10.36305467784173118 ) ) ;
#25428 = CARTESIAN_POINT ( 'NONE',  ( 120.7947214775786193, -9.261995988541697145, -16.69588392320189030 ) ) ;
#25429 = EDGE_CURVE ( 'NONE', #18421, #18481, #2036, .T. ) ;
#25430 = CARTESIAN_POINT ( 'NONE',  ( 137.0998855943435615, 0.2258552152529801627, -15.16215999076406362 ) ) ;
#25431 = EDGE_CURVE ( 'NONE', #20559, #23478, #11713, .T. ) ;
#25432 = CARTESIAN_POINT ( 'NONE',  ( 109.4407702545248355, -10.62599879583958717, -15.77991374673208469 ) ) ;
#25433 = CARTESIAN_POINT ( 'NONE',  ( 109.2294421295247844, 7.836001204160461420, -14.64321520033831447 ) ) ;
#25434 = FACE_OUTER_BOUND ( 'NONE', #24735, .T. ) ;
#25435 = CARTESIAN_POINT ( 'NONE',  ( 114.7886608795247696, -1.325403438956436419, -16.93181055722141792 ) ) ;
#25436 = CARTESIAN_POINT ( 'NONE',  ( 117.6180281442453150, -0.4660016031367893996, -10.09054647747474043 ) ) ;
#25437 = VECTOR ( 'NONE', #14083, 1000.000000000000000 ) ;
#25438 = AXIS2_PLACEMENT_3D ( 'NONE', #18325, #543, #42725 ) ;
#25439 = CARTESIAN_POINT ( 'NONE',  ( -1.637506834317598026, -6.775152287193681566, -19.39321520033831447 ) ) ;
#25440 = CARTESIAN_POINT ( 'NONE',  ( 116.8805814775786445, -3.505236298600246325, -18.68346056562440793 ) ) ;
#25441 = CARTESIAN_POINT ( 'NONE',  ( 70.19189222814998175, -57.05206236706784040, -36.02363522683400276 ) ) ;
#25442 = CARTESIAN_POINT ( 'NONE',  ( 70.19189222814998175, -55.40259354030312267, -35.36385344588251911 ) ) ;
#25443 = CARTESIAN_POINT ( 'NONE',  ( 108.6073327545248048, -6.936859964151250502, -8.388885654883777576 ) ) ;
#25444 = CARTESIAN_POINT ( 'NONE',  ( 122.2173036525449987, -2.378957183258595176, -17.95140958770220863 ) ) ;
#25445 = CARTESIAN_POINT ( 'NONE',  ( 27.78057335388972504, -13.48551096636548330, -19.39321520033831447 ) ) ;
#25446 = CARTESIAN_POINT ( 'NONE',  ( 122.8568014173871177, -8.493878760966627084, -17.54745775818410536 ) ) ;
#25448 = CARTESIAN_POINT ( 'NONE',  ( 119.0361948109119652, -7.893985811506177619, -18.51759400769804742 ) ) ;
#25447 = CARTESIAN_POINT ( 'NONE',  ( 61.87551538731119649, -14.47097590406426093, -8.981403309440874949 ) ) ;
#25449 = CARTESIAN_POINT ( 'NONE',  ( 118.6958348109119754, -3.505236298600246325, -18.68346056562440793 ) ) ;
#25450 = CARTESIAN_POINT ( 'NONE',  ( 113.7606148109119886, -7.894159318335828068, -9.358103419637847864 ) ) ;
#25451 = ORIENTED_EDGE ( 'NONE', *, *, #44531, .F. ) ;
#25452 = CARTESIAN_POINT ( 'NONE',  ( 135.3184548109119874, -7.067465109756605912, -7.812468278694988832 ) ) ;
#25453 = CARTESIAN_POINT ( 'NONE',  ( 123.7445081442452874, -1.561330072975668948, -17.79121239304076951 ) ) ;
#25454 = CARTESIAN_POINT ( 'NONE',  ( 113.6079577545248043, -2.791137627527939813, -18.39754474579286025 ) ) ;
#25455 = CARTESIAN_POINT ( 'NONE',  ( 119.8870948109119752, -0.8288870151387760510, -10.36305467784173118 ) ) ;
#25456 = CARTESIAN_POINT ( 'NONE',  ( 121.1350814775786233, -9.859900752359378018, -12.68260735090039759 ) ) ;
#25457 = CARTESIAN_POINT ( 'NONE',  ( 118.0151148109119816, 0.4262465694468514643, -12.03445270309931736 ) ) ;
#25458 = FACE_OUTER_BOUND ( 'NONE', #9282, .T. ) ;
#25459 = CARTESIAN_POINT ( 'NONE',  ( 107.2182702545248105, -10.62599879583958717, -15.77991374673208469 ) ) ;
#25460 = CARTESIAN_POINT ( 'NONE',  ( 124.0848681442452772, -5.574606645277164318, -18.38911715685844683 ) ) ;
#25461 = CARTESIAN_POINT ( 'NONE',  ( 123.5743281442453139, -2.084020599724406786, -8.691656652584148546 ) ) ;
#25462 = CARTESIAN_POINT ( 'NONE',  ( 116.1319545411901970, -0.3595008806742178709, -10.82052240173746682 ) ) ;
#25463 = CARTESIAN_POINT ( 'NONE',  ( -13.56828337869067269, -4.779084862086131480, -8.846323889245468308 ) ) ;
#25464 = CARTESIAN_POINT ( 'NONE',  ( 122.3132204359119868, -10.25716656981731489, -12.88942061488890545 ) ) ;
#25465 = CARTESIAN_POINT ( 'NONE',  ( 115.4137390045248566, 0.8980012041604421569, -15.77991374673208469 ) ) ;
#25466 = CARTESIAN_POINT ( 'NONE',  ( 116.8411475980424257, 1.961928045763841499, -20.95697541397089836 ) ) ;
#25467 = FACE_OUTER_BOUND ( 'NONE', #781, .T. ) ;
#25468 = CARTESIAN_POINT ( 'NONE',  ( 117.7882081442453170, -6.344957434206665248, -7.627207830600338134 ) ) ;
#25469 = CARTESIAN_POINT ( 'NONE',  ( 120.1707281442453166, 0.2603800115204892296, -16.42320221600525088 ) ) ;
#25470 = CARTESIAN_POINT ( 'NONE',  ( 109.3713171295247832, -10.62599879583958540, -13.39321520033831447 ) ) ;
#25471 = CARTESIAN_POINT ( 'NONE',  ( 113.6471614775786492, -5.638512984488999180, -18.83840828888717311 ) ) ;
#25472 = VERTEX_POINT ( 'NONE', #15962 ) ;
#25473 = DIRECTION ( 'NONE',  ( -0.8636456077245092677, 0.5040994586965584778, 0.000000000000000000 ) ) ;
#25474 = CARTESIAN_POINT ( 'NONE',  ( 118.0151148109119816, -10.63000616557722466, -14.87417383870573495 ) ) ;
#25475 = CONICAL_SURFACE ( 'NONE', #29826, 2.445500000000004448, 0.9599310885968757034 ) ;
#25476 = CARTESIAN_POINT ( 'NONE',  ( 120.5110881442453206, -3.505236298600246325, -18.68346056562440793 ) ) ;
#25477 = CARTESIAN_POINT ( 'NONE',  ( 114.7249681442453237, -9.565557343593413364, -10.61323700422348004 ) ) ;
#25478 = CARTESIAN_POINT ( 'NONE',  ( 121.6456214775786293, -10.63000616557722466, -14.87417383870573495 ) ) ;
#25479 = CARTESIAN_POINT ( 'NONE',  ( 112.5661608795247872, -8.938348069036489818, -9.318865927141430916 ) ) ;
#25480 = AXIS2_PLACEMENT_3D ( 'NONE', #1131, #1354, #4323 ) ;
#25481 = EDGE_CURVE ( 'NONE', #4318, #15657, #34978, .T. ) ;
#25482 = CARTESIAN_POINT ( 'NONE',  ( 115.0086014775786509, -5.574606645277164318, -18.38911715685844683 ) ) ;
#25483 = CARTESIAN_POINT ( 'NONE',  ( 120.7157985609119635, -10.36940331770106916, -15.09355782777062061 ) ) ;
#25484 = CARTESIAN_POINT ( 'NONE',  ( 123.6776560953690591, -6.001247023715324147, -18.26661038929047010 ) ) ;
#25485 = VERTEX_POINT ( 'NONE', #16419 ) ;
#25486 = AXIS2_PLACEMENT_3D ( 'NONE', #34337, #38426, #13610 ) ;
#25487 = CARTESIAN_POINT ( 'NONE',  ( 123.4244704359119709, 1.345710702986147034, -13.97328579221134426 ) ) ;
#25488 = CARTESIAN_POINT ( 'NONE',  ( 117.6180281442453150, -0.4660016031367893996, -10.09054647747474043 ) ) ;
#25489 = ORIENTED_EDGE ( 'NONE', *, *, #7813, .F. ) ;
#25490 = CARTESIAN_POINT ( 'NONE',  ( 125.1309504620138284, -2.495269033102075262, -17.79652296963211455 ) ) ;
#25491 = CARTESIAN_POINT ( 'NONE',  ( -13.52882246642779940, -4.831022935409089669, -8.722530528169237130 ) ) ;
#25492 = CARTESIAN_POINT ( 'NONE',  ( 114.9716510812576757, -0.01829820670803256055, -12.14321520033831625 ) ) ;
#25493 = CARTESIAN_POINT ( 'NONE',  ( 114.5547881442453217, -4.153390946401321671, -8.397313243818183892 ) ) ;
#25494 = CARTESIAN_POINT ( 'NONE',  ( 66.02316373260774185, -0.1478461060746093236, -16.39321520033831447 ) ) ;
#25495 = CARTESIAN_POINT ( 'NONE',  ( 123.9210066692503602, -2.311015703046761072, -18.04188382666269774 ) ) ;
#25496 = CARTESIAN_POINT ( 'NONE',  ( 123.9146881442452894, -10.15424416112533912, -14.75197769757731336 ) ) ;
#25497 = CYLINDRICAL_SURFACE ( 'NONE', #1074, 1.299999999999995604 ) ;
#25498 = CARTESIAN_POINT ( 'NONE',  ( 119.9438214775786378, -2.084020599724406786, -8.691656652584148546 ) ) ;
#25499 = CONICAL_SURFACE ( 'NONE', #2180, 2.999999999999999556, 0.9599310885968830309 ) ;
#25500 = CARTESIAN_POINT ( 'NONE',  ( 68.80767435282035649, -101.8822652819988974, -48.78088070843723756 ) ) ;
#25501 = CARTESIAN_POINT ( 'NONE',  ( 123.9714148109119805, -8.899110576539710493, -16.42337572283490132 ) ) ;
#25502 = CARTESIAN_POINT ( 'NONE',  ( 113.3068014775786594, -8.166667518702817929, -8.995218007635859436 ) ) ;
#25503 = CARTESIAN_POINT ( 'NONE',  ( 117.7882081442453170, -6.344957434206665248, -7.627207830600338134 ) ) ;
#25504 = CARTESIAN_POINT ( 'NONE',  ( 112.4559014775786494, -9.988377603198976828, -10.36322818467138340 ) ) ;
#25505 = CYLINDRICAL_SURFACE ( 'NONE', #7458, 1.999999999999999112 ) ;
#25506 = CARTESIAN_POINT ( 'NONE',  ( 121.7023481442452919, -0.8288870151387760510, -10.36305467784173118 ) ) ;
#25507 = ORIENTED_EDGE ( 'NONE', *, *, #27880, .T. ) ;
#25508 = CARTESIAN_POINT ( 'NONE',  ( 122.2696148109119889, -4.089484607189486809, -7.948022111789456723 ) ) ;
#25509 = CARTESIAN_POINT ( 'NONE',  ( 113.1912390045248031, -9.868328341294098749, -11.32035403202665869 ) ) ;
#25510 = CARTESIAN_POINT ( 'NONE',  ( 82.48419058924217495, -31.76353122097473047, -22.93120623788412615 ) ) ;
#25511 = CARTESIAN_POINT ( 'NONE',  ( 70.19189222814998175, -59.83749578782295941, -37.13779888561150244 ) ) ;
#25512 = VECTOR ( 'NONE', #2911, 1000.000000000000114 ) ;
#25513 = CARTESIAN_POINT ( 'NONE',  ( 138.1290508867525659, -3.202662983232241523, -16.85452216123445623 ) ) ;
#25514 = CARTESIAN_POINT ( 'NONE',  ( 115.9693640045247776, 0.1403307496149616695, -15.46607636864997204 ) ) ;
#25515 = ORIENTED_EDGE ( 'NONE', *, *, #36970, .F. ) ;
#25516 = AXIS2_PLACEMENT_3D ( 'NONE', #4107, #472, #15061 ) ;
#25517 = CARTESIAN_POINT ( 'NONE',  ( 119.9438214775786378, -2.084020599724406786, -8.691656652584148546 ) ) ;
#25518 = CARTESIAN_POINT ( 'NONE',  ( 119.7434548109119703, -7.554583864224885481, -18.48844787311982785 ) ) ;
#25519 = CARTESIAN_POINT ( 'NONE',  ( 64.39944321480182055, -15.22860971205249569, -17.87854327940120669 ) ) ;
#25520 = CARTESIAN_POINT ( 'NONE',  ( 125.2761281442453054, -10.63000616557722466, -14.87417383870573495 ) ) ;
#25521 = CARTESIAN_POINT ( 'NONE',  ( 108.4684265045248424, -2.791137627527939813, -8.388885654883777576 ) ) ;
#25522 = VERTEX_POINT ( 'NONE', #29637 ) ;
#25523 = CARTESIAN_POINT ( 'NONE',  ( 116.0864081442453113, -9.988377603198976828, -10.36322818467138340 ) ) ;
#25524 = CARTESIAN_POINT ( 'NONE',  ( 88.53603805838689311, -11.36969738595376000, -13.94316338922722665 ) ) ;
#25525 = CARTESIAN_POINT ( 'NONE',  ( 121.3619881442452879, -5.574606645277164318, -18.38911715685844683 ) ) ;
#25526 = CARTESIAN_POINT ( 'NONE',  ( 112.6828081442453282, -2.084020599724406786, -8.691656652584148546 ) ) ;
#25527 = PRODUCT_RELATED_PRODUCT_CATEGORY ( 'part', '', ( #10664 ) ) ;
#25528 = CARTESIAN_POINT ( 'NONE',  ( 123.6877814775786675, -6.222761293078255207, -8.102969835052217462 ) ) ;
#25529 = FACE_OUTER_BOUND ( 'NONE', #31231, .T. ) ;
#25530 = CARTESIAN_POINT ( 'NONE',  ( 86.34560043013698305, -9.320000780048239619, -18.64321520033831803 ) ) ;
#25531 = CARTESIAN_POINT ( 'NONE',  ( 125.1626748109119802, -0.1624402480850797581, -16.17319339645315424 ) ) ;
#25532 = EDGE_LOOP ( 'NONE', ( #19869, #15055, #4235, #33781, #16747, #9670 ) ) ;
#25533 = CARTESIAN_POINT ( 'NONE',  ( 116.5249890045247980, -9.868328341294098749, -11.32035403202665869 ) ) ;
#25534 = VECTOR ( 'NONE', #41833, 1000.000000000000000 ) ;
#25535 = CARTESIAN_POINT ( 'NONE',  ( 121.8158014775786171, -5.638512984488999180, -18.83840828888717311 ) ) ;
#25536 = CARTESIAN_POINT ( 'NONE',  ( 137.5082292857711082, -8.696096796519196204, -16.61830971866196549 ) ) ;
#25537 = ORIENTED_EDGE ( 'NONE', *, *, #37021, .T. ) ;
#25538 = CARTESIAN_POINT ( 'NONE',  ( 136.7036351578996403, 0.3218787459907788695, -11.14856471978897190 ) ) ;
#25539 = CARTESIAN_POINT ( 'NONE',  ( 125.1059481442452750, -8.166667518702819706, -8.995218007635861213 ) ) ;
#25540 = FACE_OUTER_BOUND ( 'NONE', #6130, .T. ) ;
#25541 = CARTESIAN_POINT ( 'NONE',  ( 122.3830681442452857, -1.833838273342659697, -17.42832698103878286 ) ) ;
#25542 = ORIENTED_EDGE ( 'NONE', *, *, #43174, .T. ) ;
#25543 = VECTOR ( 'NONE', #27040, 1000.000000000000114 ) ;
#25544 = CARTESIAN_POINT ( 'NONE',  ( 119.0361948109119652, -7.893985811506177619, -18.51759400769804742 ) ) ;
#25545 = CARTESIAN_POINT ( 'NONE',  ( 116.6991193335884418, -2.334846009198389805, -18.01015021110788439 ) ) ;
#25546 = CIRCLE ( 'NONE', #2258, 5.000000000000004441 ) ;
#25547 = CARTESIAN_POINT ( 'NONE',  ( 79.79010115959992788, 5.106172230548759572, -19.89321520033831447 ) ) ;
#25548 = CARTESIAN_POINT ( 'NONE',  ( 136.5278073585037077, -5.459964313008185854, -7.687332562961293192 ) ) ;
#25549 = CARTESIAN_POINT ( 'NONE',  ( 125.7299414775786346, 0.9020085738987339008, -11.91225656197089222 ) ) ;
#25550 = DIRECTION ( 'NONE',  ( 0.1352586133457950590, 0.9908103287288504424, 0.000000000000000000 ) ) ;
#25551 = FACE_OUTER_BOUND ( 'NONE', #10625, .T. ) ;
#25552 = CARTESIAN_POINT ( 'NONE',  ( 125.4463081442452932, -5.638512984488999180, -18.83840828888717311 ) ) ;
#25553 = CARTESIAN_POINT ( 'NONE',  ( 113.4202548109119846, -10.30919188438810075, -12.61870101168855918 ) ) ;
#25554 = CARTESIAN_POINT ( 'NONE',  ( 67.30914723170953096, -59.52904673731846685, -37.90892823192145755 ) ) ;
#25555 = CARTESIAN_POINT ( 'NONE',  ( 122.9503348109119827, -9.859900752359378018, -12.68260735090039759 ) ) ;
#25556 = DIRECTION ( 'NONE',  ( 0.000000000000000000, -0.3818493186865936084, 0.9242245927363024194 ) ) ;
#25557 = CARTESIAN_POINT ( 'NONE',  ( 120.0572748109119772, -3.383040157471821630, -19.15922257007629170 ) ) ;
#25558 = CARTESIAN_POINT ( 'NONE',  ( 126.2184548109090940, -8.862178061931365036, -16.39564131203211517 ) ) ;
#25559 = CARTESIAN_POINT ( 'NONE',  ( 114.5108483795247878, -0.7896495226426338832, -9.318865927141430916 ) ) ;
#25560 = CARTESIAN_POINT ( 'NONE',  ( 110.4131140045248287, 0.1403307496149616695, -15.46607636864997204 ) ) ;
#25561 = CARTESIAN_POINT ( 'NONE',  ( 112.7745202545247878, 0.1403307496149616695, -11.32035403202665336 ) ) ;
#25562 = AXIS2_PLACEMENT_3D ( 'NONE', #41062, #20525, #6840 ) ;
#25563 = CARTESIAN_POINT ( 'NONE',  ( 124.8790414775786388, -8.899110576539117190, -16.42337572283568647 ) ) ;
#25564 = CARTESIAN_POINT ( 'NONE',  ( 114.7816948109119863, 0.5811942927096154232, -14.16772938898807155 ) ) ;
#25565 = ORIENTED_EDGE ( 'NONE', *, *, #10543, .F. ) ;
#25566 = CARTESIAN_POINT ( 'NONE',  ( 116.4834948109119779, -7.894159318335828068, -9.358103419637847864 ) ) ;
#25567 = CARTESIAN_POINT ( 'NONE',  ( 108.4684265045247997, -7.250697342233347165, -19.15521520033831138 ) ) ;
#25568 = DIRECTION ( 'NONE',  ( 0.000000000000000000, 0.000000000000000000, -1.000000000000000000 ) ) ;
#25569 = CARTESIAN_POINT ( 'NONE',  ( 84.49707967414211396, -25.23119213852205789, -15.24166438581092109 ) ) ;
#25570 = EDGE_CURVE ( 'NONE', #24054, #9778, #4413, .T. ) ;
#25571 = ADVANCED_FACE ( 'NONE', ( #43552 ), #12320, .T. ) ;
#25572 = DIRECTION ( 'NONE',  ( -0.000000000000000000, -0.9284778069183720062, -0.3713878862591650232 ) ) ;
#25573 = FACE_BOUND ( 'NONE', #12362, .T. ) ;
#25574 = CARTESIAN_POINT ( 'NONE',  ( 116.7671281442453335, -1.834011780172310813, -8.268836392978581529 ) ) ;
#25575 = CARTESIAN_POINT ( 'NONE',  ( 112.0799890045248475, 0.8980012041604421569, -15.77991374673208469 ) ) ;
#25576 = CARTESIAN_POINT ( 'NONE',  ( 109.9269421295247753, -9.868328341294093420, -13.39321520033831447 ) ) ;
#25577 = ORIENTED_EDGE ( 'NONE', *, *, #2440, .T. ) ;
#25578 = CARTESIAN_POINT ( 'NONE',  ( 73.01241679510815175, -68.13509210538408922, -39.58160742654554554 ) ) ;
#25579 = AXIS2_PLACEMENT_3D ( 'NONE', #18794, #15373, #22880 ) ;
#25580 = CARTESIAN_POINT ( 'NONE',  ( 120.3409081442453044, -8.899110576539710493, -16.42337572283490132 ) ) ;
#25581 = CARTESIAN_POINT ( 'NONE',  ( 116.9940348109119839, -9.988377603198976828, -10.36322818467138340 ) ) ;
#25582 = CARTESIAN_POINT ( 'NONE',  ( 112.7395348109119766, -5.638512984488999180, -18.83840828888717311 ) ) ;
#25583 = CIRCLE ( 'NONE', #39309, 2.999999999999999556 ) ;
#25584 = CARTESIAN_POINT ( 'NONE',  ( 125.1626748109119802, -0.1624402480850797581, -16.17319339645315424 ) ) ;
#25585 = CARTESIAN_POINT ( 'NONE',  ( 122.2696148109119889, -5.574606645277164318, -18.38911715685844683 ) ) ;
#25586 = CARTESIAN_POINT ( 'NONE',  ( 114.9518748109119883, -7.643976991954077427, -18.09477374809248928 ) ) ;
#25587 = ORIENTED_EDGE ( 'NONE', *, *, #23099, .T. ) ;
#25588 = CARTESIAN_POINT ( 'NONE',  ( 120.2296266859119953, -0.06289925094097943703, -9.412459353600674206 ) ) ;
#25589 = DIRECTION ( 'NONE',  ( 0.000000000000000000, 0.4669533266896288004, 0.8842819633428518067 ) ) ;
#25590 = CARTESIAN_POINT ( 'NONE',  ( 118.0718414775786442, -0.8288870151387760510, -10.36305467784173118 ) ) ;
#25591 = ORIENTED_EDGE ( 'NONE', *, *, #32524, .T. ) ;
#25592 = CARTESIAN_POINT ( 'NONE',  ( 91.38554522942851577, -26.60966817898065884, -11.90521360603286816 ) ) ;
#25593 = CARTESIAN_POINT ( 'NONE',  ( 116.5969481442453031, 0.5811942927096154232, -14.16772938898807155 ) ) ;
#25594 = CARTESIAN_POINT ( 'NONE',  ( 107.5655358795247736, -8.402594152722688392, -9.854619843455216355 ) ) ;
#25595 = CARTESIAN_POINT ( 'NONE',  ( 112.2289948109119848, -7.643976991954077427, -18.09477374809248928 ) ) ;
#25596 = EDGE_CURVE ( 'NONE', #14979, #36847, #9119, .T. ) ;
#25597 = ORIENTED_EDGE ( 'NONE', *, *, #19748, .T. ) ;
#25598 = ORIENTED_EDGE ( 'NONE', *, *, #36161, .F. ) ;
#25599 = CIRCLE ( 'NONE', #15403, 2.000000000000000444 ) ;
#25600 = CARTESIAN_POINT ( 'NONE',  ( 123.7445081442452874, -7.894159318335828068, -9.358103419637847864 ) ) ;
#25601 = CARTESIAN_POINT ( 'NONE',  ( 116.6536748109119941, -10.15424416112533912, -14.75197769757731336 ) ) ;
#25602 = CARTESIAN_POINT ( 'NONE',  ( 124.5706358376855860, -9.845282878008639216, -13.85115115540643593 ) ) ;
#25603 = ADVANCED_FACE ( 'NONE', ( #37374 ), #31089, .T. ) ;
#25604 = CARTESIAN_POINT ( 'NONE',  ( 116.4834948109119779, -7.894159318335808528, -9.358103419637833653 ) ) ;
#25605 = VERTEX_POINT ( 'NONE', #11444 ) ;
#25606 = DIRECTION ( 'NONE',  ( 0.000000000000000000, 0.3818493186865927203, -0.9242245927363029745 ) ) ;
#25607 = CARTESIAN_POINT ( 'NONE',  ( 71.91396631829535124, -25.73035770285813939, -4.893215200338314474 ) ) ;
#25608 = EDGE_CURVE ( 'NONE', #17168, #16401, #18996, .T. ) ;
#25609 = CARTESIAN_POINT ( 'NONE',  ( 109.5796765045248122, -7.250697342233347165, -19.15521520033831138 ) ) ;
#25610 = CIRCLE ( 'NONE', #24885, 6.479565957685750277 ) ;
#25611 = CARTESIAN_POINT ( 'NONE',  ( 114.9518748109119883, -1.834011780172310813, -8.268836392978581529 ) ) ;
#25612 = CARTESIAN_POINT ( 'NONE',  ( 125.8433948109119456, -7.643976991954077427, -18.09477374809248928 ) ) ;
#25613 = CARTESIAN_POINT ( 'NONE',  ( 120.7379948109119709, 0.4262465694468514643, -12.03445270309931736 ) ) ;
#25614 = FACE_OUTER_BOUND ( 'NONE', #16598, .T. ) ;
#25615 = ORIENTED_EDGE ( 'NONE', *, *, #27157, .T. ) ;
#25616 = CARTESIAN_POINT ( 'NONE',  ( 121.3052614775786111, -7.643976991954077427, -18.09477374809248928 ) ) ;
#25617 = EDGE_CURVE ( 'NONE', #25152, #16121, #31361, .T. ) ;
#25618 = PLANE ( 'NONE',  #23353 ) ;
#25619 = CARTESIAN_POINT ( 'NONE',  ( 116.8028015045247940, -6.936859964151250502, -18.39754474579286025 ) ) ;
#25620 = CARTESIAN_POINT ( 'NONE',  ( 116.5026997424434114, -0.9924539043446216624, -17.29976612834909133 ) ) ;
#25621 = B_SPLINE_CURVE_WITH_KNOTS ( 'NONE', 3,
 ( #28993, #39700, #7559, #11662, #1386, #21473, #25351, #22146, #35585, #14631 ),
 .UNSPECIFIED., .F., .F.,
 ( 4, 3, 3, 4 ),
 ( 5.421010862427519859E-18, 0.0002476486541971024665, 0.0004952973025691049819, 0.0009610892161188130988 ),
 .UNSPECIFIED. ) ;
#25622 = CARTESIAN_POINT ( 'NONE',  ( 120.2274548109119934, 0.5811942927096110934, -14.16772938898807510 ) ) ;
#25623 = ORIENTED_EDGE ( 'NONE', *, *, #35941, .T. ) ;
#25624 = ADVANCED_FACE ( 'NONE', ( #9996 ), #5701, .T. ) ;
#25625 = CARTESIAN_POINT ( 'NONE',  ( 116.8238548109119819, -4.089484607189486809, -7.948022111789456723 ) ) ;
#25626 = DIRECTION ( 'NONE',  ( -0.6937550123170076466, 0.2674776663120608799, -0.6686999932026935767 ) ) ;
#25627 = CARTESIAN_POINT ( 'NONE',  ( 109.3018640045248304, -10.62599879583958717, -11.00651665394454604 ) ) ;
#25628 = CARTESIAN_POINT ( 'NONE',  ( 115.6325948109119821, 0.2603800115204892296, -16.42320221600525088 ) ) ;
#25629 = ADVANCED_FACE ( 'NONE', ( #13851 ), #29910, .F. ) ;
#25630 = EDGE_CURVE ( 'NONE', #20781, #36610, #23366, .T. ) ;
#25631 = CARTESIAN_POINT ( 'NONE',  ( 116.8805814775786445, -6.344957434206662583, -7.627207830600332805 ) ) ;
#25632 = DIRECTION ( 'NONE',  ( 1.000000000000000000, 0.000000000000000000, -0.000000000000000000 ) ) ;
#25633 = CARTESIAN_POINT ( 'NONE',  ( 72.75524511225664526, -25.99489077589583630, -8.393215200338314474 ) ) ;
#25634 = CARTESIAN_POINT ( 'NONE',  ( 106.3153796295248412, -4.863998795839590272, -8.388885654883775800 ) ) ;
#25635 = ORIENTED_EDGE ( 'NONE', *, *, #28135, .F. ) ;
#25636 = CARTESIAN_POINT ( 'NONE',  ( 109.2294321978889542, -10.20217893803289222, -14.76446976949403656 ) ) ;
#25637 = AXIS2_PLACEMENT_3D ( 'NONE', #7293, #17568, #20549 ) ;
#25638 = CARTESIAN_POINT ( 'NONE',  ( 119.4332814775786318, -8.899110576539710493, -16.42337572283490132 ) ) ;
#25640 = CARTESIAN_POINT ( 'NONE',  ( 111.1076452545248259, -9.868328341294098749, -15.46607636864997204 ) ) ;
#25639 = APPLICATION_CONTEXT ( 'automotive_design' ) ;
#25641 = CARTESIAN_POINT ( 'NONE',  ( 115.6915515045247531, -6.936859964151250502, -18.39754474579286025 ) ) ;
#25642 = CARTESIAN_POINT ( 'NONE',  ( 114.3846081442453197, 0.4262465694468514643, -12.03445270309931736 ) ) ;
#25643 = FACE_OUTER_BOUND ( 'NONE', #35550, .T. ) ;
#25644 = CARTESIAN_POINT ( 'NONE',  ( 124.9357681442453014, -1.834011780172310813, -8.268836392978581529 ) ) ;
#25645 = CARTESIAN_POINT ( 'NONE',  ( 121.4187148109119789, -6.344957434206665248, -7.627207830600338134 ) ) ;
#25646 = VERTEX_POINT ( 'NONE', #5255 ) ;
#25647 = CARTESIAN_POINT ( 'NONE',  ( 117.5613014775786525, -10.15424416112533912, -14.75197769757731336 ) ) ;
#25648 = CARTESIAN_POINT ( 'NONE',  ( 113.1366214775786432, -1.834011780172310813, -8.268836392978581529 ) ) ;
#25649 = CARTESIAN_POINT ( 'NONE',  ( 120.5678148109119832, -8.166667518702819706, -8.995218007635861213 ) ) ;
#25650 = CARTESIAN_POINT ( 'NONE',  ( 119.0929214775786278, -4.153390946401325223, -8.397313243818185668 ) ) ;
#25651 = ORIENTED_EDGE ( 'NONE', *, *, #4716, .F. ) ;
#25652 = CARTESIAN_POINT ( 'NONE',  ( 75.95778847736481509, -3.256761025687722189, -7.993215200338315007 ) ) ;
#25653 = CARTESIAN_POINT ( 'NONE',  ( 121.6456214775786293, -10.63000616557722466, -14.87417383870573495 ) ) ;
#25654 = CARTESIAN_POINT ( 'NONE',  ( 124.1685108350155957, -8.515285166876527256, -6.287188262108023729 ) ) ;
#25655 = LINE ( 'NONE', #15391, #19881 ) ;
#25656 = AXIS2_PLACEMENT_3D ( 'NONE', #36501, #44042, #44275 ) ;
#25657 = CARTESIAN_POINT ( 'NONE',  ( 126.9675933030687531, 0.5041375662892478848, -13.12963104399455894 ) ) ;
#25658 = CARTESIAN_POINT ( 'NONE',  ( 113.0523327545247838, -6.936859964151250502, -8.388885654883777576 ) ) ;
#25659 = AXIS2_PLACEMENT_3D ( 'NONE', #40650, #19898, #5742 ) ;
#25660 = CARTESIAN_POINT ( 'NONE',  ( 121.9470836909669913, -24.14644159042263993, -12.62951656296512937 ) ) ;
#25661 = CARTESIAN_POINT ( 'NONE',  ( 114.8951481442453115, -8.899110576539710493, -16.42337572283490132 ) ) ;
#25662 = CARTESIAN_POINT ( 'NONE',  ( 124.1983214775786166, -8.166667518702819706, -8.995218007635861213 ) ) ;
#25663 = CARTESIAN_POINT ( 'NONE',  ( 64.96812053257905006, -13.31534605384092984, -15.09338587514541352 ) ) ;
#25664 = EDGE_CURVE ( 'NONE', #26785, #24453, #20483, .T. ) ;
#25665 = CARTESIAN_POINT ( 'NONE',  ( -13.23804852390367337, -4.035795733041972255, -7.689295463341079717 ) ) ;
#25666 = CARTESIAN_POINT ( 'NONE',  ( 110.1353015045248469, -6.936859964151250502, -18.39754474579286025 ) ) ;
#25667 = CARTESIAN_POINT ( 'NONE',  ( 112.5693548109119888, 0.4262465694468514643, -12.03445270309931736 ) ) ;
#25668 = AXIS2_PLACEMENT_3D ( 'NONE', #29142, #22303, #31654 ) ;
#25669 = CARTESIAN_POINT ( 'NONE',  ( -1.637506834317628890, -6.775152287193632716, -18.06807615187975102 ) ) ;
#25671 = CARTESIAN_POINT ( 'NONE',  ( 121.0216281442452981, -1.561330072975668948, -17.79121239304076951 ) ) ;
#25670 = CARTESIAN_POINT ( 'NONE',  ( 62.99198783763660003, -14.62836571490823978, -8.152764136444947241 ) ) ;
#25672 = CARTESIAN_POINT ( 'NONE',  ( 124.3117748109119844, 0.1319031606808879209, -14.10382304977623669 ) ) ;
#25673 = ORIENTED_EDGE ( 'NONE', *, *, #25320, .T. ) ;
#25674 = CARTESIAN_POINT ( 'NONE',  ( 136.7478768735679751, -9.183261188161861099, -9.792427337551218969 ) ) ;
#25675 = CARTESIAN_POINT ( 'NONE',  ( 116.5987716749792895, -9.866677412677834269, -13.52174868289714027 ) ) ;
#25676 = CARTESIAN_POINT ( 'NONE',  ( 110.0658483795247804, -8.402594152722688392, -16.93181055722141792 ) ) ;
#25677 = CARTESIAN_POINT ( 'NONE',  ( 117.5613014775786525, -10.15424416112533912, -14.75197769757731336 ) ) ;
#25678 = CARTESIAN_POINT ( 'NONE',  ( 122.4397948109119767, -0.1624402480850797581, -16.17319339645315424 ) ) ;
#25679 = CARTESIAN_POINT ( 'NONE',  ( 116.7671281442453335, -7.643976991954077427, -18.09477374809248928 ) ) ;
#25680 = CARTESIAN_POINT ( 'NONE',  ( 120.7335793026122701, -1.179503403430468333, -17.05068175419387089 ) ) ;
#25681 = CARTESIAN_POINT ( 'NONE',  ( 106.9404577545248145, -7.250697342233347165, -7.631215200338321125 ) ) ;
#25682 = CARTESIAN_POINT ( 'NONE',  ( 123.6877814775786533, -6.222761293078241884, -8.102969835052219238 ) ) ;
#25683 = CARTESIAN_POINT ( 'NONE',  ( 122.9503348109119827, -9.859900752359378018, -12.68260735090039759 ) ) ;
#25684 = CARTESIAN_POINT ( 'NONE',  ( 78.69189222814998175, -69.76310523276724496, -16.89321520033831447 ) ) ;
#25685 = PLANE ( 'NONE',  #29183 ) ;
#25686 = CARTESIAN_POINT ( 'NONE',  ( 120.7852516859119731, -0.6942167230862511529, -9.935906262978006609 ) ) ;
#25687 = CARTESIAN_POINT ( 'NONE',  ( 114.9275671295247889, -10.62599879583958540, -13.39321520033831447 ) ) ;
#25688 = LINE ( 'NONE', #16098, #4376 ) ;
#25689 = CARTESIAN_POINT ( 'NONE',  ( 82.42681365487543133, -31.76737129425208295, -22.90237778003977809 ) ) ;
#25690 = CARTESIAN_POINT ( 'NONE',  ( 122.4965214775786251, -10.30919188438810075, -12.61870101168855918 ) ) ;
#25691 = CARTESIAN_POINT ( 'NONE',  ( 117.1074881442453233, -10.63000616557722466, -14.87417383870573495 ) ) ;
#25692 = CARTESIAN_POINT ( 'NONE',  ( 105.5513952545248060, 0.8980012041604421569, -11.00651665394454071 ) ) ;
#25693 = EDGE_CURVE ( 'NONE', #38837, #36947, #33283, .T. ) ;
#25694 = CARTESIAN_POINT ( 'NONE',  ( 111.7184548109119788, -9.261995988541697145, -16.69588392320189030 ) ) ;
#25695 = FACE_OUTER_BOUND ( 'NONE', #42110, .T. ) ;
#25696 = VERTEX_POINT ( 'NONE', #6561 ) ;
#25697 = CARTESIAN_POINT ( 'NONE',  ( 89.40092984481313465, -25.99489077589524300, -13.39321520033831625 ) ) ;
#25698 = CARTESIAN_POINT ( 'NONE',  ( 115.0653281442453277, -6.344957434206662583, -7.627207830600332805 ) ) ;
#25699 = CARTESIAN_POINT ( 'NONE',  ( 123.9146881442452894, -10.15424416112533912, -14.75197769757731336 ) ) ;
#25700 = SHAPE_DEFINITION_REPRESENTATION ( #21216, #38750 ) ;
#25701 = CARTESIAN_POINT ( 'NONE',  ( 114.6682414775786469, -7.894159318335828068, -9.358103419637847864 ) ) ;
#25702 = CARTESIAN_POINT ( 'NONE',  ( 120.1140014775786398, -1.561330072975668504, -17.79121239304076951 ) ) ;
#25703 = AXIS2_PLACEMENT_3D ( 'NONE', #35716, #42808, #32962 ) ;
#25704 = CARTESIAN_POINT ( 'NONE',  ( 114.2330358795247776, -0.7896495226426338832, -17.46756447353520159 ) ) ;
#25705 = VECTOR ( 'NONE', #18536, 1000.000000000000000 ) ;
#25706 = CARTESIAN_POINT ( 'NONE',  ( 118.8092881442453290, -0.1624402480850797581, -16.17319339645315424 ) ) ;
#25707 = DIRECTION ( 'NONE',  ( -0.2768435750659241079, -0.3568721902840695792, 0.8921882507333129819 ) ) ;
#25708 = CARTESIAN_POINT ( 'NONE',  ( 85.15861813568058380, -26.75858941326842810, -11.54476601486570964 ) ) ;
#25709 = VERTEX_POINT ( 'NONE', #30955 ) ;
#25710 = CARTESIAN_POINT ( 'NONE',  ( 123.5633766859119760, -0.06289925094097943703, -9.412459353600674206 ) ) ;
#25711 = CARTESIAN_POINT ( 'NONE',  ( 118.4689281442453392, 0.9020085738987339008, -11.91225656197089222 ) ) ;
#25712 = ORIENTED_EDGE ( 'NONE', *, *, #19812, .F. ) ;
#25713 = CARTESIAN_POINT ( 'NONE',  ( 125.3895814775786448, -2.084020599724406786, -8.691656652584148546 ) ) ;
#25714 = CARTESIAN_POINT ( 'NONE',  ( -13.50772587709714578, -4.858790063452675057, -8.690212664598012893 ) ) ;
#25715 = CYLINDRICAL_SURFACE ( 'NONE', #16551, 3.000000000000002665 ) ;
#25716 = CARTESIAN_POINT ( 'NONE',  ( 119.6601881442453106, -1.833838273342659253, -17.42832698103878286 ) ) ;
#25717 = LINE ( 'NONE', #39847, #21507 ) ;
#25718 = CARTESIAN_POINT ( 'NONE',  ( 64.79538738837304379, -35.65327282786526553, -5.786495942213274901 ) ) ;
#25719 = CARTESIAN_POINT ( 'NONE',  ( 122.4965214775786251, 0.1319031606808879209, -14.10382304977623669 ) ) ;
#25720 = CARTESIAN_POINT ( 'NONE',  ( 121.6456214775786435, -10.63000616557722999, -14.87417383870568877 ) ) ;
#25721 = VECTOR ( 'NONE', #44670, 1000.000000000000000 ) ;
#25722 = CARTESIAN_POINT ( 'NONE',  ( 125.3895814775786448, -2.084020599724406786, -8.691656652584148546 ) ) ;
#25723 = CARTESIAN_POINT ( 'NONE',  ( 125.3574654937850426, -11.58588033818513097, -15.49098285581515455 ) ) ;
#25724 = CARTESIAN_POINT ( 'NONE',  ( 117.7314814775786260, -5.574606645277164318, -18.38911715685844683 ) ) ;
#25725 = CARTESIAN_POINT ( 'NONE',  ( 122.7234281442452755, -4.153390946401325223, -8.397313243818185668 ) ) ;
#25726 = CARTESIAN_POINT ( 'NONE',  ( 114.6115148109119986, -3.383040157471821630, -19.15922257007629170 ) ) ;
#25727 = CARTESIAN_POINT ( 'NONE',  ( 121.0783548109119749, 0.2603800115204892296, -16.42320221600525088 ) ) ;
#25728 = CARTESIAN_POINT ( 'NONE',  ( 116.9373081442452929, -8.166667518702817929, -8.995218007635861213 ) ) ;
#25729 = LINE ( 'NONE', #7714, #16174 ) ;
#25730 = CARTESIAN_POINT ( 'NONE',  ( 123.8579614775786126, -9.859900752359378018, -12.68260735090039759 ) ) ;
#25731 = EDGE_LOOP ( 'NONE', ( #14284, #39614, #3659 ) ) ;
#25732 = CARTESIAN_POINT ( 'NONE',  ( 119.1496481442453046, -3.383040157471821630, -19.15922257007629170 ) ) ;
#25733 = CARTESIAN_POINT ( 'NONE',  ( 114.0941296295247867, -4.863998795839590272, -19.15521520033831493 ) ) ;
#25734 = CARTESIAN_POINT ( 'NONE',  ( 115.6220983795247861, -8.402594152722688392, -16.93181055722141792 ) ) ;
#25735 = DIRECTION ( 'NONE',  ( 0.000000000000000000, 0.3818493186865927203, -0.9242245927363029745 ) ) ;
#25736 = AXIS2_PLACEMENT_3D ( 'NONE', #28011, #24363, #44675 ) ;
#25737 = CARTESIAN_POINT ( 'NONE',  ( 114.6682414775786469, -7.894159318335828068, -9.358103419637847864 ) ) ;
#25738 = EDGE_CURVE ( 'NONE', #19235, #37757, #37788, .T. ) ;
#25739 = CARTESIAN_POINT ( 'NONE',  ( 120.1601735609119856, 0.6414057260225851653, -11.69287257290600657 ) ) ;
#25740 = CARTESIAN_POINT ( 'NONE',  ( 126.0703014775786102, -9.988377603198980381, -10.36322818467138518 ) ) ;
#25741 = ORIENTED_EDGE ( 'NONE', *, *, #126, .F. ) ;
#25742 = CARTESIAN_POINT ( 'NONE',  ( 122.6099748109119929, -0.8288870151387760510, -10.36305467784173118 ) ) ;
#25743 = CARTESIAN_POINT ( 'NONE',  ( 73.60369002873177635, -5.846784287000932778, -16.89321520033831447 ) ) ;
#25744 = CARTESIAN_POINT ( 'NONE',  ( 119.8823610609119754, -3.163656168406935087, -18.89861972220014508 ) ) ;
#25745 = CARTESIAN_POINT ( 'NONE',  ( 123.5880035264548837, -8.247323210606174015, -17.08054893949881858 ) ) ;
#25746 = CARTESIAN_POINT ( 'NONE',  ( 106.3848327545248651, -6.936859964151250502, -8.388885654883777576 ) ) ;
#25747 = ORIENTED_EDGE ( 'NONE', *, *, #33171, .F. ) ;
#25748 = CARTESIAN_POINT ( 'NONE',  ( 114.6115148109119986, -3.383040157471821630, -19.15922257007629170 ) ) ;
#25749 = CARTESIAN_POINT ( 'NONE',  ( 125.5030348109119558, -3.383040157471821630, -19.15922257007629170 ) ) ;
#25750 = CARTESIAN_POINT ( 'NONE',  ( 119.0361948109119652, -2.084020599724406786, -8.691656652584148546 ) ) ;
#25751 = LINE ( 'NONE', #32575, #7367 ) ;
#25752 =( LENGTH_UNIT ( ) NAMED_UNIT ( * ) SI_UNIT ( .MILLI., .METRE. ) );
#25753 = DIRECTION ( 'NONE',  ( -1.000000000000000000, 0.000000000000000000, 0.000000000000000000 ) ) ;
#25754 = CARTESIAN_POINT ( 'NONE',  ( 124.6329298793804981, -2.191907684172563986, -18.20049396185734025 ) ) ;
#25755 = ORIENTED_EDGE ( 'NONE', *, *, #42112, .F. ) ;
#25756=STYLED_ITEM('',(#45162),#21433);
#25757 = CARTESIAN_POINT ( 'NONE',  ( 114.5108483795247878, -8.402594152722688392, -16.93181055722141792 ) ) ;
#25758 = EDGE_CURVE ( 'NONE', #35202, #42996, #36488, .T. ) ;
#25759 = CARTESIAN_POINT ( 'NONE',  ( 121.0216281442452981, -1.561330072975668948, -17.79121239304076951 ) ) ;
#25760 = CARTESIAN_POINT ( 'NONE',  ( 137.0596819398251967, -9.757506281569700235, -15.72392196484829974 ) ) ;
#25761 = ORIENTED_EDGE ( 'NONE', *, *, #39681, .T. ) ;
#25762 = CARTESIAN_POINT ( 'NONE',  ( 115.6325948109119821, 0.2603800115204892296, -16.42320221600525088 ) ) ;
#25763 = CARTESIAN_POINT ( 'NONE',  ( 111.6050014775786536, 0.1319031606808879209, -14.10382304977623669 ) ) ;
#25764 = CARTESIAN_POINT ( 'NONE',  ( 110.5757045411902908, -0.3595008806742185925, -10.82052240173743130 ) ) ;
#25765 = CARTESIAN_POINT ( 'NONE',  ( 121.8725281442453223, -6.222761293078241884, -8.102969835052219238 ) ) ;
#25766 = AXIS2_PLACEMENT_3D ( 'NONE', #28410, #34985, #32037 ) ;
#25767 = ORIENTED_EDGE ( 'NONE', *, *, #20893, .T. ) ;
#25768 = CARTESIAN_POINT ( 'NONE',  ( 118.8092881442453290, -9.988377603198976828, -10.36322818467138340 ) ) ;
#25769 = CARTESIAN_POINT ( 'NONE',  ( 69.69189222814998175, -41.76310523276723785, -20.39321520033831447 ) ) ;
#25770 = CARTESIAN_POINT ( 'NONE',  ( 117.2294421295247844, 0.2335149919452661482, -4.893215200338314474 ) ) ;
#25771 = CARTESIAN_POINT ( 'NONE',  ( 119.7434548109119703, 3.074545301078819737, -12.40350937470759973 ) ) ;
#25772 = CYLINDRICAL_SURFACE ( 'NONE', #13460, 5.000000000000000888 ) ;
#25773 = CARTESIAN_POINT ( 'NONE',  ( 114.3278814775786429, 0.1319031606808879209, -14.10382304977623669 ) ) ;
#25774 = CARTESIAN_POINT ( 'NONE',  ( 70.19189222814998175, -55.40259354030312267, -35.36385344588251911 ) ) ;
#25775 = CARTESIAN_POINT ( 'NONE',  ( 124.5779955726312949, -3.841352728425414753, -21.19493817005371383 ) ) ;
#25776 = CARTESIAN_POINT ( 'NONE',  ( 111.4348214775786801, -3.505236298600246325, -18.68346056562440793 ) ) ;
#25777 = CARTESIAN_POINT ( 'NONE',  ( 125.6164881442453094, -9.565557343593413364, -10.61323700422348004 ) ) ;
#25778 = CARTESIAN_POINT ( 'NONE',  ( 122.8560864091100768, -0.9924539043446216624, -17.29976612834909133 ) ) ;
#25779 = CARTESIAN_POINT ( 'NONE',  ( 122.7234281442452755, -4.153390946401325223, -8.397313243818185668 ) ) ;
#25780 = CARTESIAN_POINT ( 'NONE',  ( 64.71874404463645192, -15.46959023120085064, -16.14765141715094998 ) ) ;
#25781 = CARTESIAN_POINT ( 'NONE',  ( 120.7379948109119709, -10.63000616557722466, -14.87417383870573495 ) ) ;
#25782 = CARTESIAN_POINT ( 'NONE',  ( 114.6515776191212836, 0.4261359969231631739, -12.14321520033831625 ) ) ;
#25783 = CARTESIAN_POINT ( 'NONE',  ( 125.7866681442453256, -8.899110576539117190, -16.42337572283568647 ) ) ;
#25784 = CARTESIAN_POINT ( 'NONE',  ( 108.8851452545248151, -9.868328341294098749, -15.46607636864997204 ) ) ;
#25785 = CARTESIAN_POINT ( 'NONE',  ( 108.7462390045248242, -9.868328341294098749, -11.32035403202665869 ) ) ;
#25786 = CARTESIAN_POINT ( 'NONE',  ( 125.6626748109119802, -9.522524984348629928, -10.63868154973292413 ) ) ;
#25787 = CARTESIAN_POINT ( 'NONE',  ( 115.0653281442453277, -6.344957434206662583, -7.627207830600332805 ) ) ;
#25788 = ORIENTED_EDGE ( 'NONE', *, *, #16802, .T. ) ;
#25789 = CARTESIAN_POINT ( 'NONE',  ( 107.5655358795247736, -0.7896495226426338832, -17.46756447353520159 ) ) ;
#25790 = CARTESIAN_POINT ( 'NONE',  ( 119.5918314802850091, -3.929494816604741203, -18.62311481910882804 ) ) ;
#25791 = CARTESIAN_POINT ( 'NONE',  ( 126.1837548109119211, -10.63000616557722466, -14.87417383870573495 ) ) ;
#25792 = FACE_OUTER_BOUND ( 'NONE', #15204, .T. ) ;
#25793 = CARTESIAN_POINT ( 'NONE',  ( 112.3424481442453384, -6.344957434206662583, -7.627207830600332805 ) ) ;
#25794 = CARTESIAN_POINT ( 'NONE',  ( 120.6812681442452941, -10.30919188438810075, -12.61870101168855918 ) ) ;
#25795 = CARTESIAN_POINT ( 'NONE',  ( 111.9410827545248708, -2.477300249445798297, -19.15521520033831138 ) ) ;
#25796 = CARTESIAN_POINT ( 'NONE',  ( 111.1076452545248259, -9.868328341294098749, -15.46607636864997204 ) ) ;
#25797 = ORIENTED_EDGE ( 'NONE', *, *, #6990, .T. ) ;
#25798 = DIRECTION ( 'NONE',  ( -0.9970811988817437355, 0.07634843047859309062, 0.000000000000000000 ) ) ;
#25799 = CARTESIAN_POINT ( 'NONE',  ( 118.4122014775786340, -9.859900752359374465, -12.68260735090039404 ) ) ;
#25800 = CARTESIAN_POINT ( 'NONE',  ( 116.0864081442453113, -9.988377603198976828, -10.36322818467138340 ) ) ;
#25801 = CARTESIAN_POINT ( 'NONE',  ( 112.3424481442453384, -6.344957434206662583, -7.627207830600332805 ) ) ;
#25802 = CARTESIAN_POINT ( 'NONE',  ( 123.9714148109119805, -8.899110576539710493, -16.42337572283490132 ) ) ;
#25803 = CARTESIAN_POINT ( 'NONE',  ( 124.4252281442452812, -0.8288870151387760510, -10.36305467784173118 ) ) ;
#25804 = CARTESIAN_POINT ( 'NONE',  ( 116.5969481442453031, -9.859900752359374465, -12.68260735090039404 ) ) ;
#25805 = VERTEX_POINT ( 'NONE', #34580 ) ;
#25806 = CIRCLE ( 'NONE', #14189, 2.999999999999999556 ) ;
#25807 = CARTESIAN_POINT ( 'NONE',  ( 124.5357204359119550, -10.25716656981731489, -12.88942061488890545 ) ) ;
#25808 = DIRECTION ( 'NONE',  ( 1.000000000000000000, 0.000000000000000000, -0.000000000000000000 ) ) ;
#25809 = CARTESIAN_POINT ( 'NONE',  ( 118.0151148109119816, 0.4262465694468514643, -12.03445270309931736 ) ) ;
#25810 = VERTEX_POINT ( 'NONE', #19172 ) ;
#25811 = CARTESIAN_POINT ( 'NONE',  ( 126.9733055311764502, -9.698541571718097387, -15.74778416720804763 ) ) ;
#25812 = CARTESIAN_POINT ( 'NONE',  ( 114.3846081442453197, -10.63000616557722466, -14.87417383870573495 ) ) ;
#25813 = CARTESIAN_POINT ( 'NONE',  ( 116.4555358795247884, -0.7896495226426338832, -17.46756447353520159 ) ) ;
#25814 = CARTESIAN_POINT ( 'NONE',  ( 114.3846081442453197, 0.4262465694468514643, -12.03445270309931736 ) ) ;
#25815 = ORIENTED_EDGE ( 'NONE', *, *, #12499, .T. ) ;
#25816 = EDGE_LOOP ( 'NONE', ( #42303, #32779, #4059, #23370, #31135 ) ) ;
#25817 = CARTESIAN_POINT ( 'NONE',  ( 121.0783548109119749, -9.565557343593413364, -10.61323700422348004 ) ) ;
#25818 = CARTESIAN_POINT ( 'NONE',  ( 115.8027748109119841, -8.899110576539710493, -16.42337572283490132 ) ) ;
#25819 =( LENGTH_UNIT ( ) NAMED_UNIT ( * ) SI_UNIT ( .MILLI., .METRE. ) );
#25820 = EDGE_CURVE ( 'NONE', #1411, #36318, #32279, .T. ) ;
#25821 = VERTEX_POINT ( 'NONE', #17282 ) ;
#25822 = CARTESIAN_POINT ( 'NONE',  ( 112.1721994132789320, -8.900630651041904429, -16.42135045828372597 ) ) ;
#25823 = CARTESIAN_POINT ( 'NONE',  ( 71.85867159647438029, -25.32195970414818476, -4.893215200338314474 ) ) ;
#25824 = CARTESIAN_POINT ( 'NONE',  ( 111.2465515045248168, -2.477300249445798297, -7.631215200338321125 ) ) ;
#25825 = CARTESIAN_POINT ( 'NONE',  ( 118.0151148109119816, -10.63000616557722466, -14.87417383870573495 ) ) ;
#25827 = CARTESIAN_POINT ( 'NONE',  ( 115.0086014775786509, -5.574606645277164318, -18.38911715685844683 ) ) ;
#25826 = CARTESIAN_POINT ( 'NONE',  ( 114.8384214775786489, 0.9020085738987339008, -11.91225656197089222 ) ) ;
#25828 = CARTESIAN_POINT ( 'NONE',  ( 121.4187148109119789, -3.505236298600246325, -18.68346056562440793 ) ) ;
#25829 = CARTESIAN_POINT ( 'NONE',  ( 70.19189222814998175, -60.40547808481815650, -37.36498982452450690 ) ) ;
#25830 = ORIENTED_EDGE ( 'NONE', *, *, #45086, .F. ) ;
#25831 = CARTESIAN_POINT ( 'NONE',  ( 118.9794681442453026, -0.8288870151387760510, -10.36305467784173118 ) ) ;
#25832 = CARTESIAN_POINT ( 'NONE',  ( 124.0848681442452772, -5.574606645277164318, -18.38911715685844683 ) ) ;
#25833 = VECTOR ( 'NONE', #7531, 1000.000000000000000 ) ;
#25834 = CARTESIAN_POINT ( 'NONE',  ( 114.9970202545248412, -10.62599879583958717, -15.77991374673208469 ) ) ;
#25835 = CARTESIAN_POINT ( 'NONE',  ( 116.3166296295247832, -4.863998795839590272, -8.388885654883775800 ) ) ;
#25836 = CARTESIAN_POINT ( 'NONE',  ( 113.6079577545248043, -7.250697342233347165, -7.631215200338321125 ) ) ;
#25837 = CARTESIAN_POINT ( 'NONE',  ( 119.4332814775786318, -0.4660016031367893996, -10.09054647747474043 ) ) ;
#25838 = VERTEX_POINT ( 'NONE', #5474 ) ;
#25839 = CARTESIAN_POINT ( 'NONE',  ( 120.9649014775786355, -3.383040157471821630, -19.15922257007629170 ) ) ;
#25840 = DIRECTION ( 'NONE',  ( -0.000000000000000000, -0.9284778069183721172, -0.3713878862591650232 ) ) ;
#25841 = DIRECTION ( 'NONE',  ( 0.9609149988134843001, -0.1028163501681632064, 0.2570431154366505933 ) ) ;
#25842 = CARTESIAN_POINT ( 'NONE',  ( 117.7882081442453170, -6.344957434206665248, -7.627207830600338134 ) ) ;
#25843 = CARTESIAN_POINT ( 'NONE',  ( 116.9940348109119839, -9.988377603198976828, -10.36322818467138340 ) ) ;
#25845 = CIRCLE ( 'NONE', #10567, 5.999999999999997335 ) ;
#25844 = CARTESIAN_POINT ( 'NONE',  ( 125.7866681442452688, -8.899110576539710493, -16.42337572283490132 ) ) ;
#25846 = CARTESIAN_POINT ( 'NONE',  ( 116.8784914538011179, -11.65352397162535603, -6.030266697614802496 ) ) ;
#25847 = EDGE_CURVE ( 'NONE', #31533, #8410, #42312, .T. ) ;
#25848 = ORIENTED_EDGE ( 'NONE', *, *, #8269, .T. ) ;
#25849 = CARTESIAN_POINT ( 'NONE',  ( -1.637506834317598026, -6.775152287193681566, -8.893215200338314474 ) ) ;
#25850 = CARTESIAN_POINT ( 'NONE',  ( 109.2295251720720728, -9.839649396385770075, -15.65853133350598014 ) ) ;
#25851 = CARTESIAN_POINT ( 'NONE',  ( 119.2063748109119814, -7.894159318335828068, -9.358103419637847864 ) ) ;
#25852 = CARTESIAN_POINT ( 'NONE',  ( 113.9552233795247815, -1.325403438956436419, -9.854619843455211026 ) ) ;
#25853 = CARTESIAN_POINT ( 'NONE',  ( 105.6903015045248253, -2.477300249445798297, -7.631215200338321125 ) ) ;
#25854 = CARTESIAN_POINT ( 'NONE',  ( 114.9518748109119883, -7.643976991954077427, -18.09477374809248928 ) ) ;
#25855 = CARTESIAN_POINT ( 'NONE',  ( 71.02242295334774269, -52.26753456854214619, -37.21464843399728295 ) ) ;
#25856 = CARTESIAN_POINT ( 'NONE',  ( 69.81876103444739101, -25.95566152907768753, -5.787138065658625763 ) ) ;
#25857 = EDGE_CURVE ( 'NONE', #35384, #17767, #24820, .T. ) ;
#25858 = CARTESIAN_POINT ( 'NONE',  ( 111.6617281442453304, 0.4262465694468514643, -12.03445270309931736 ) ) ;
#25859 = CARTESIAN_POINT ( 'NONE',  ( 118.4689281442453392, 0.9020085738987339008, -11.91225656197089222 ) ) ;
#25860 = VERTEX_POINT ( 'NONE', #40375 ) ;
#25861 = EDGE_CURVE ( 'NONE', #30491, #23154, #15354, .T. ) ;
#25862 = CARTESIAN_POINT ( 'NONE',  ( 119.0361948109119652, -2.084020599724406786, -8.691656652584148546 ) ) ;
#25863 = CARTESIAN_POINT ( 'NONE',  ( 115.2922348109119781, -10.63000616557722466, -14.87417383870573495 ) ) ;
#25864 = CARTESIAN_POINT ( 'NONE',  ( 121.6456214775786293, -10.63000616557722466, -14.87417383870573495 ) ) ;
#25865 = AXIS2_PLACEMENT_3D ( 'NONE', #2388, #33846, #22468 ) ;
#25866 = CARTESIAN_POINT ( 'NONE',  ( 119.7169148109119874, -0.1624402480850797581, -16.17319339645315424 ) ) ;
#25867 = ORIENTED_EDGE ( 'NONE', *, *, #39430, .F. ) ;
#25868 = CARTESIAN_POINT ( 'NONE',  ( 124.2550481442452792, -0.1624402480850797581, -16.17319339645315424 ) ) ;
#25869 = VECTOR ( 'NONE', #7878, 1000.000000000000114 ) ;
#25870 = CARTESIAN_POINT ( 'NONE',  ( 121.3052614775786111, -1.834011780172310813, -8.268836392978581529 ) ) ;
#25871 = CARTESIAN_POINT ( 'NONE',  ( 124.8633137343399113, -8.262852723283208078, -6.486460572651194134 ) ) ;
#25872 = CARTESIAN_POINT ( 'NONE',  ( 121.3052614775786111, -1.834011780172310813, -8.268836392978581529 ) ) ;
#25873 = EDGE_CURVE ( 'NONE', #35202, #2361, #38450, .T. ) ;
#25874 = ADVANCED_FACE ( 'NONE', ( #35242 ), #31615, .F. ) ;
#25875 = EDGE_CURVE ( 'NONE', #20614, #18078, #29550, .T. ) ;
#25876 = AXIS2_PLACEMENT_3D ( 'NONE', #7809, #35828, #32853 ) ;
#25877 = DIRECTION ( 'NONE',  ( 0.000000000000000000, 0.9284778069183720062, 0.3713878862591650232 ) ) ;
#25878 = CARTESIAN_POINT ( 'NONE',  ( 138.1466326771052024, -2.059073704699106333, -15.87940239184555757 ) ) ;
#25879 = CARTESIAN_POINT ( 'NONE',  ( 114.8581140045248361, 0.1403307496149616695, -15.46607636864997204 ) ) ;
#25880 = DIRECTION ( 'NONE',  ( 0.000000000000000000, -0.9242245927363029745, -0.3818493186865927758 ) ) ;
#25881 = CARTESIAN_POINT ( 'NONE',  ( 136.9394333025885260, -10.02432842090376575, -11.47584239480924495 ) ) ;
#25882 = CARTESIAN_POINT ( 'NONE',  ( 115.7460481442453357, -10.15424416112533912, -14.75197769757731336 ) ) ;
#25883 = CARTESIAN_POINT ( 'NONE',  ( 125.3895814775786448, -7.893985811506177619, -18.51759400769804742 ) ) ;
#25884 = CARTESIAN_POINT ( 'NONE',  ( 65.18805517862392662, -13.43643968393412358, -14.85905743718944727 ) ) ;
#25885 = CARTESIAN_POINT ( 'NONE',  ( 73.07463722459043254, -54.78256478388924933, -34.22133621331339981 ) ) ;
#25886 = CARTESIAN_POINT ( 'NONE',  ( 110.6909265045248247, -2.791137627527939813, -8.388885654883777576 ) ) ;
#25887 = CARTESIAN_POINT ( 'NONE',  ( 115.8595014775786609, -7.643976991954077427, -18.09477374809248928 ) ) ;
#25888 = DIRECTION ( 'NONE',  ( 0.000000000000000000, 0.000000000000000000, -1.000000000000000000 ) ) ;
#25889 = CARTESIAN_POINT ( 'NONE',  ( -2.026929177228822709, -6.892617277590884051, -18.91977777107071645 ) ) ;
#25891 = CARTESIAN_POINT ( 'NONE',  ( 118.2987481442453088, -1.561330072975668504, -17.79121239304076951 ) ) ;
#25890 = CARTESIAN_POINT ( 'NONE',  ( 65.38099912316067730, -15.98743937505324553, -9.669194438446968576 ) ) ;
#25892 = CIRCLE ( 'NONE', #12826, 2.445500000000004448 ) ;
#25893 = CARTESIAN_POINT ( 'NONE',  ( 121.9859814775786333, -9.565557343593413364, -10.61323700422348004 ) ) ;
#25894 = ORIENTED_EDGE ( 'NONE', *, *, #30301, .F. ) ;
#25895 = DIRECTION ( 'NONE',  ( 0.000000000000000000, 0.000000000000000000, -1.000000000000000000 ) ) ;
#25896 = CARTESIAN_POINT ( 'NONE',  ( 125.2761281442453054, -10.63000616557722466, -14.87417383870573495 ) ) ;
#25897 = CARTESIAN_POINT ( 'NONE',  ( 110.4131140045248287, 0.1403307496149616695, -15.46607636864997204 ) ) ;
#25898 = CARTESIAN_POINT ( 'NONE',  ( 122.4397948109119767, -0.1624402480850797581, -16.17319339645315424 ) ) ;
#25899 =( BOUNDED_CURVE ( )  B_SPLINE_CURVE ( 2, ( #23173, #37052, #5823, #42296, #34751, #24302, #41637, #3533, #10393, #10835, #11284, #14475, #17896, #18120, #17449, #31344, #14031 ),
 .UNSPECIFIED., .F., .T. ) 
 B_SPLINE_CURVE_WITH_KNOTS ( ( 3, 2, 2, 2, 2, 2, 2, 2, 3 ),
 ( 0.5796282416568590001, 0.5859375000000000000, 0.5937500000000000000, 0.6015625000000000000, 0.6093750000000000000, 0.6171875000000000000, 0.6250000000000000000, 0.6328125000000000000, 0.6391217583431409999 ),
 .UNSPECIFIED. ) 
 CURVE ( )  GEOMETRIC_REPRESENTATION_ITEM ( )  RATIONAL_B_SPLINE_CURVE ( ( 0.9763430640195970289, 0.9385262470928680267, 1.000000000000000000, 0.9238795325112869605, 1.000000000000000000, 0.9238795325112869605, 1.000000000000000000, 0.9238795325112869605, 1.000000000000000000, 0.9238795325112869605, 1.000000000000000000, 0.9238795325112869605, 1.000000000000000000, 0.9238795325112869605, 1.000000000000000000, 0.9385262470928670275, 0.9763430640195980281 ) ) 
 REPRESENTATION_ITEM ( '' )  );
#25900 = CARTESIAN_POINT ( 'NONE',  ( 122.8368814775786291, -7.894159318335828068, -9.358103419637847864 ) ) ;
#25901 = CARTESIAN_POINT ( 'NONE',  ( 117.2209414775786485, -2.084020599724406786, -8.691656652584148546 ) ) ;
#25902 = CARTESIAN_POINT ( 'NONE',  ( 123.9584548109119737, 1.449227268523328505, -18.30678586333412738 ) ) ;
#25903 = CARTESIAN_POINT ( 'NONE',  ( 108.8156921295247912, 0.8980012041604618078, -13.39321520033831447 ) ) ;
#25904 = CARTESIAN_POINT ( 'NONE',  ( 125.2761281442453054, 0.4262465694468514643, -12.03445270309931736 ) ) ;
#25905 = CARTESIAN_POINT ( 'NONE',  ( 123.7445081442452874, -7.894159318335828068, -9.358103419637847864 ) ) ;
#25906 = DIRECTION ( 'NONE',  ( 1.000000000000000000, 0.000000000000000000, -0.000000000000000000 ) ) ;
#25907 = FACE_OUTER_BOUND ( 'NONE', #24468, .T. ) ;
#25908 = CARTESIAN_POINT ( 'NONE',  ( 123.9106423109119675, -9.959231468620755479, -10.70263013195267199 ) ) ;
#25909 = CARTESIAN_POINT ( 'NONE',  ( 114.7886608795247696, -8.938348069036489818, -9.318865927141430916 ) ) ;
#25910 = CARTESIAN_POINT ( 'NONE',  ( -13.61777589163126123, -4.713943292400020191, -18.99709152357623410 ) ) ;
#25911 = CARTESIAN_POINT ( 'NONE',  ( 84.02342478082003652, -31.32369313687246049, -21.95975535756046071 ) ) ;
#25912 = CARTESIAN_POINT ( 'NONE',  ( 122.7801548109119665, -3.383040157471821630, -19.15922257007629170 ) ) ;
#25913 = CARTESIAN_POINT ( 'NONE',  ( 116.9373081442452929, -8.166667518702817929, -8.995218007635861213 ) ) ;
#25914 = CARTESIAN_POINT ( 'NONE',  ( 108.8156921295247912, 0.8980012041604618078, -13.39321520033831447 ) ) ;
#25915 = CARTESIAN_POINT ( 'NONE',  ( 116.5402214775786405, 0.2603800115204892296, -16.42320221600525088 ) ) ;
#25916 = CARTESIAN_POINT ( 'NONE',  ( 121.9470836909669913, -24.14644159042263993, -12.62951656296512937 ) ) ;
#25917 = VERTEX_POINT ( 'NONE', #8353 ) ;
#25918 = DIRECTION ( 'NONE',  ( 0.000000000000000000, 0.6004852223388321697, -0.7996358532186279566 ) ) ;
#25919 = AXIS2_PLACEMENT_3D ( 'NONE', #135, #34770, #3549 ) ;
#25920 = EDGE_CURVE ( 'NONE', #15215, #21469, #12231, .T. ) ;
#25921 = CARTESIAN_POINT ( 'NONE',  ( 119.6034614775786196, -6.344957434206665248, -7.627207830600338134 ) ) ;
#25922 = CARTESIAN_POINT ( 'NONE',  ( 126.0703014775786102, -0.1624402480850797581, -16.17319339645315424 ) ) ;
#25923 = PRODUCT_CONTEXT ( 'NONE', #16044, 'mechanical' ) ;
#25924 = CARTESIAN_POINT ( 'NONE',  ( 113.6471614775786492, -4.153390946401321671, -8.397313243818183892 ) ) ;
#25925 = CARTESIAN_POINT ( 'NONE',  ( 111.7751814775786556, -2.084020599724406786, -8.691656652584148546 ) ) ;
#25926 = CARTESIAN_POINT ( 'NONE',  ( 109.2324108795247923, -8.938348069036489818, -9.318865927141430916 ) ) ;
#25927 = CARTESIAN_POINT ( 'NONE',  ( 121.8158014775786171, -4.153390946401325223, -8.397313243818185668 ) ) ;
#25928 = CARTESIAN_POINT ( 'NONE',  ( 116.7565503026016813, -4.863998795840742240, -18.55532337341522364 ) ) ;
#25929 = AXIS2_PLACEMENT_3D ( 'NONE', #12402, #15590, #26302 ) ;
#25930 = DIRECTION ( 'NONE',  ( 0.000000000000000000, -0.4669533266896290225, -0.8842819633428516957 ) ) ;
#25931 = ORIENTED_EDGE ( 'NONE', *, *, #27571, .T. ) ;
#25932 = ADVANCED_FACE ( 'NONE', ( #15193 ), #8798, .T. ) ;
#25933 = DIRECTION ( 'NONE',  ( 0.000000000000000000, -0.3818493186865927203, 0.9242245927363029745 ) ) ;
#25934 = CARTESIAN_POINT ( 'NONE',  ( 122.2696148109119889, -4.089484607189486809, -7.948022111789456723 ) ) ;
#25935 = FACE_OUTER_BOUND ( 'NONE', #34410, .T. ) ;
#25936 = CARTESIAN_POINT ( 'NONE',  ( 65.10175888621736817, -2.513761081768071559, -8.357200856923110877 ) ) ;
#25937 = SURFACE_STYLE_FILL_AREA ( #1528 ) ;
#25938 = CARTESIAN_POINT ( 'NONE',  ( 117.9583881442453048, 0.1319031606808879209, -14.10382304977623669 ) ) ;
#25939 = DIRECTION ( 'NONE',  ( 0.7871354856660167654, -0.6167752151498625546, -0.002461946824136807422 ) ) ;
#25940 = EDGE_CURVE ( 'NONE', #1444, #15917, #22641, .T. ) ;
#25941 = CARTESIAN_POINT ( 'NONE',  ( 65.06330879403716949, -35.71473443186641816, -5.721420406450495655 ) ) ;
#25942 = CARTESIAN_POINT ( 'NONE',  ( 124.0281414775786146, -7.643976991954077427, -18.09477374809248928 ) ) ;
#25943 = CARTESIAN_POINT ( 'NONE',  ( 123.7245631242421382, -1.016270020561755860, -17.26805140881366896 ) ) ;
#25944 = VECTOR ( 'NONE', #39510, 1000.000000000000114 ) ;
#25945 = CARTESIAN_POINT ( 'NONE',  ( 124.4252281442452812, -0.8288870151387760510, -10.36305467784173118 ) ) ;
#25946 = CARTESIAN_POINT ( 'NONE',  ( 124.5035785706779876, -11.90564393026358481, -16.97396928258573112 ) ) ;
#25947 = CARTESIAN_POINT ( 'NONE',  ( 124.1983214775786166, -8.166667518702819706, -8.995218007635861213 ) ) ;
#25948 = CARTESIAN_POINT ( 'NONE',  ( 118.5256548109119876, -8.899110576539710493, -16.42337572283490132 ) ) ;
#25949 = CARTESIAN_POINT ( 'NONE',  ( 122.6667014775786413, -2.084020599724406786, -8.691656652584148546 ) ) ;
#25950 = CARTESIAN_POINT ( 'NONE',  ( 120.1140014775786398, -1.561330072975668504, -17.79121239304076951 ) ) ;
#25951 = CARTESIAN_POINT ( 'NONE',  ( 116.0864081442453113, -9.988377603198976828, -10.36322818467138340 ) ) ;
#25952 = CARTESIAN_POINT ( 'NONE',  ( 114.4413952545248350, -9.868328341294098749, -15.46607636864997204 ) ) ;
#25953 = CARTESIAN_POINT ( 'NONE',  ( 123.7445081442452874, -7.894159318335828068, -9.358103419637847864 ) ) ;
#25954 = ORIENTED_EDGE ( 'NONE', *, *, #29962, .F. ) ;
#25955 = CARTESIAN_POINT ( 'NONE',  ( 120.4543614775786295, -4.089484607189486809, -7.948022111789456723 ) ) ;
#25956 = CARTESIAN_POINT ( 'NONE',  ( 113.8857702545248003, -10.62599879583958717, -15.77991374673208469 ) ) ;
#25957 = CARTESIAN_POINT ( 'NONE',  ( 108.8156921295247912, -9.868328341294093420, -13.39321520033831447 ) ) ;
#25958 = CYLINDRICAL_SURFACE ( 'NONE', #43039, 3.500000000000003109 ) ;
#25959 = CARTESIAN_POINT ( 'NONE',  ( 113.9875214775786532, -8.899110576539710493, -16.42337572283490132 ) ) ;
#25960 = CARTESIAN_POINT ( 'NONE',  ( 84.39081516114408998, -30.32262605124144272, -9.757176231017245627 ) ) ;
#25961 = AXIS2_PLACEMENT_3D ( 'NONE', #3035, #58, #13972 ) ;
#25962 = CARTESIAN_POINT ( 'NONE',  ( 116.7333483795247844, -8.402594152722688392, -16.93181055722141792 ) ) ;
#25963 = B_SPLINE_CURVE_WITH_KNOTS ( 'NONE', 3,
 ( #10420, #23887, #24543, #13832, #30483, #37998, #7199, #21112, #37771, #16819 ),
 .UNSPECIFIED., .F., .F.,
 ( 4, 3, 3, 4 ),
 ( 0.000000000000000000, 0.0001671877560958124893, 0.0003343755126086590075, 0.0006438490228505489759 ),
 .UNSPECIFIED. ) ;
#25964 = ORIENTED_EDGE ( 'NONE', *, *, #32365, .F. ) ;
#25965 = CARTESIAN_POINT ( 'NONE',  ( 125.6732148109119862, -9.859900752359378018, -12.68260735090039759 ) ) ;
#25966 = CARTESIAN_POINT ( 'NONE',  ( 122.5910329359119970, -4.283928203966213211, -7.183505701512925334 ) ) ;
#25967 = CARTESIAN_POINT ( 'NONE',  ( 120.5768923109119868, -9.959231468620755479, -10.70263013195267199 ) ) ;
#25968 = CARTESIAN_POINT ( 'NONE',  ( 123.6361688928271150, -8.278628333885240664, -17.13983228602120690 ) ) ;
#25969 = CARTESIAN_POINT ( 'NONE',  ( 105.9681140045248355, 0.1403307496149616695, -15.46607636864997204 ) ) ;
#25970 = ORIENTED_EDGE ( 'NONE', *, *, #42209, .T. ) ;
#25971 = CARTESIAN_POINT ( 'NONE',  ( 114.7249681442453237, 0.2603800115204892296, -16.42320221600525088 ) ) ;
#25972 = CARTESIAN_POINT ( 'NONE',  ( 116.2659068881580708, -12.01880880694303855, -20.89321520033831447 ) ) ;
#25973 = CARTESIAN_POINT ( 'NONE',  ( 124.1415948109119540, -3.505236298600246325, -18.68346056562440793 ) ) ;
#25974 = CARTESIAN_POINT ( 'NONE',  ( 113.9307948109119764, -10.15424416112533912, -14.75197769757731336 ) ) ;
#25975 = FILL_AREA_STYLE ('',( #1343 ) ) ;
#25976 = DIRECTION ( 'NONE',  ( 0.000000000000000000, 0.9242245927363028635, 0.3818493186865930533 ) ) ;
#25977 = MECHANICAL_DESIGN_GEOMETRIC_PRESENTATION_REPRESENTATION (  '', ( #2631 ), #17104 ) ;
#25978 = CARTESIAN_POINT ( 'NONE',  ( 71.67504600870660170, -26.72445618319088823, -4.893215200338314474 ) ) ;
#25979 = CARTESIAN_POINT ( 'NONE',  ( 113.8740681442453138, 0.5811942927096154232, -14.16772938898807155 ) ) ;
#25980 = EDGE_CURVE ( 'NONE', #27061, #13571, #5376, .T. ) ;
#25981 = AXIS2_PLACEMENT_3D ( 'NONE', #28242, #25267, #10690 ) ;
#25982 = CARTESIAN_POINT ( 'NONE',  ( 116.8028015045247940, -6.936859964151250502, -18.39754474579286025 ) ) ;
#25983 = CARTESIAN_POINT ( 'NONE',  ( 123.9146881442452894, 0.9020085738987339008, -11.91225656197089222 ) ) ;
#25984 =( BOUNDED_CURVE ( )  B_SPLINE_CURVE ( 2, ( #12791, #40604, #9592, #23272, #30787, #23508, #34192, #37393, #6400, #27372, #13471, #36930, #2738 ),
 .UNSPECIFIED., .F., .T. ) 
 B_SPLINE_CURVE_WITH_KNOTS ( ( 3, 2, 2, 2, 2, 2, 3 ),
 ( 0.8920046674808920217, 0.8984375000000000000, 0.9062500000000000000, 0.9140625000000000000, 0.9218750000000000000, 0.9296875000000000000, 0.9375000000000000000 ),
 .UNSPECIFIED. ) 
 CURVE ( )  GEOMETRIC_REPRESENTATION_ITEM ( )  RATIONAL_B_SPLINE_CURVE ( ( 0.9778625265006449796, 0.9373222120152220338, 1.000000000000000000, 0.9238795325112869605, 1.000000000000000000, 0.9238795325112869605, 1.000000000000000000, 0.9238795325112869605, 1.000000000000000000, 0.9238795325112869605, 1.000000000000000000, 0.9238795325112759693, 1.000000000000000000 ) ) 
 REPRESENTATION_ITEM ( '' )  );
#25985 = CARTESIAN_POINT ( 'NONE',  ( 136.9115742440178281, -8.459698128447302068, -17.59059153831742961 ) ) ;
#25986 = ORIENTED_EDGE ( 'NONE', *, *, #18903, .F. ) ;
#25987 = CARTESIAN_POINT ( 'NONE',  ( 112.9664414775786412, 0.5811942927096154232, -14.16772938898807155 ) ) ;
#25988 = CARTESIAN_POINT ( 'NONE',  ( 125.7866681442452688, -0.4660016031367893996, -10.09054647747474043 ) ) ;
#25989 = DIRECTION ( 'NONE',  ( -0.8636456077245092677, 0.5040994586965584778, 0.000000000000000000 ) ) ;
#25990 = CARTESIAN_POINT ( 'NONE',  ( 125.3328548109119964, -0.8288870151387760510, -10.36305467784173118 ) ) ;
#25991 = ORIENTED_EDGE ( 'NONE', *, *, #37255, .F. ) ;
#25992 = CARTESIAN_POINT ( 'NONE',  ( 117.7882081442453170, -6.344957434206665248, -7.627207830600338134 ) ) ;
#25993 = EDGE_CURVE ( 'NONE', #8541, #23633, #10441, .T. ) ;
#25994 = CARTESIAN_POINT ( 'NONE',  ( 64.69189222814998175, -41.76310523276723785, -23.89321520033831803 ) ) ;
#25995 = CARTESIAN_POINT ( 'NONE',  ( 79.79010115959992788, 5.106172230548759572, -12.14321520033831625 ) ) ;
#25996 = DIRECTION ( 'NONE',  ( 0.000000000000000000, 0.3818493186865928868, -0.9242245927363028635 ) ) ;
#25997 = CARTESIAN_POINT ( 'NONE',  ( 136.9115742440145880, -5.289448686423090074, -7.882678547363988208 ) ) ;
#25998 = CARTESIAN_POINT ( 'NONE',  ( 113.1933481442453058, -5.574606645277164318, -18.38911715685844683 ) ) ;
#25999 = VECTOR ( 'NONE', #44599, 1000.000000000000000 ) ;
#26000 = FACE_OUTER_BOUND ( 'NONE', #31020, .T. ) ;
#26001 = CARTESIAN_POINT ( 'NONE',  ( 125.3135537922313034, -3.242854772516403639, -20.35017254681205046 ) ) ;
#26002 = CARTESIAN_POINT ( 'NONE',  ( 125.7866681442452688, -0.4660016031367893996, -10.09054647747474043 ) ) ;
#26003 = CARTESIAN_POINT ( 'NONE',  ( 126.6942948109119840, -8.899110576539710493, -16.42337572283490132 ) ) ;
#26004 = CARTESIAN_POINT ( 'NONE',  ( 116.6639544560221253, -8.875725282760177137, -16.49651588959498127 ) ) ;
#26005 = CARTESIAN_POINT ( 'NONE',  ( 121.9292548109119849, -7.894159318335828068, -9.358103419637847864 ) ) ;
#26006 = CARTESIAN_POINT ( 'NONE',  ( 86.34560043013698305, -9.320000780048239619, -9.893215200338316251 ) ) ;
#26007 = CARTESIAN_POINT ( 'NONE',  ( 118.8092881442453290, -9.988377603198976828, -10.36322818467138340 ) ) ;
#26008 = CARTESIAN_POINT ( 'NONE',  ( 121.8725281442453223, -3.383040157471821630, -19.15922257007629170 ) ) ;
#26009 = ORIENTED_EDGE ( 'NONE', *, *, #17855, .T. ) ;
#26010 = CARTESIAN_POINT ( 'NONE',  ( 126.5125895482244971, -8.560559907796994494, -16.97480111277819148 ) ) ;
#26011 = CARTESIAN_POINT ( 'NONE',  ( 114.0246765045248196, -7.250697342233347165, -19.15521520033831138 ) ) ;
#26012 = CARTESIAN_POINT ( 'NONE',  ( 111.6632702545248605, 0.1403307496149616695, -11.32035403202665336 ) ) ;
#26013 = CARTESIAN_POINT ( 'NONE',  ( 108.8156921295247912, -9.868328341294093420, -13.39321520033831447 ) ) ;
#26014 = CARTESIAN_POINT ( 'NONE',  ( 127.0150841466605698, -9.959652887476131866, -11.61104853207065979 ) ) ;
#26015 = CARTESIAN_POINT ( 'NONE',  ( 116.4834948109119779, -1.561330072975668504, -17.79121239304076951 ) ) ;
#26016 = VERTEX_POINT ( 'NONE', #33392 ) ;
#26017 = CARTESIAN_POINT ( 'NONE',  ( 105.8986608795248401, -8.938348069036489818, -9.318865927141430916 ) ) ;
#26018 = CARTESIAN_POINT ( 'NONE',  ( 91.65862616933031859, -26.75858941326842810, -11.54476601486570964 ) ) ;
#26019 = CARTESIAN_POINT ( 'NONE',  ( 113.4769814775786330, 0.4262465694468514643, -12.03445270309931736 ) ) ;
#26020 = CARTESIAN_POINT ( 'NONE',  ( 112.6828081442453282, -7.893985811506177619, -18.51759400769804742 ) ) ;
#26021 = CARTESIAN_POINT ( 'NONE',  ( 118.9794681442453026, -9.261995988541697145, -16.69588392320189030 ) ) ;
#26022 = CARTESIAN_POINT ( 'NONE',  ( 111.1076452545248259, 0.8980012041604421569, -11.00651665394454071 ) ) ;
#26023 = DIRECTION ( 'NONE',  ( 0.000000000000000000, 0.6004852223388321697, -0.7996358532186279566 ) ) ;
#26024 = ORIENTED_EDGE ( 'NONE', *, *, #25382, .F. ) ;
#26025 = CARTESIAN_POINT ( 'NONE',  ( 110.4384831777918805, -0.01829820670803256055, -14.64321520033831447 ) ) ;
#26026 = CARTESIAN_POINT ( 'NONE',  ( 118.5823814775786360, -7.643976991954077427, -18.09477374809248928 ) ) ;
#26027 = CARTESIAN_POINT ( 'NONE',  ( 117.9583881442453048, -10.30919188438810075, -12.61870101168855918 ) ) ;
#26028 = CONICAL_SURFACE ( 'NONE', #43481, 2.000000000000000444, 0.9599310885968830309 ) ;
#26029 = CARTESIAN_POINT ( 'NONE',  ( 117.1074881442453233, -10.63000616557722466, -14.87417383870573495 ) ) ;
#26030 = CARTESIAN_POINT ( 'NONE',  ( 118.2396587682627995, -1.040089454026966287, -17.23633227186632766 ) ) ;
#26031 = CARTESIAN_POINT ( 'NONE',  ( 123.4041481442452834, 0.1319031606808879209, -14.10382304977623669 ) ) ;
#26032 = CARTESIAN_POINT ( 'NONE',  ( 116.9373081442452929, -1.833838273342659253, -17.42832698103878286 ) ) ;
#26033 = EDGE_LOOP ( 'NONE', ( #9181, #30912, #12967, #38155, #38089 ) ) ;
#26034 = CARTESIAN_POINT ( 'NONE',  ( 124.1190016859119680, -0.6942167230862511529, -9.935906262978006609 ) ) ;
#26035 = CARTESIAN_POINT ( 'NONE',  ( 112.2857214775786474, -4.089484607189486809, -7.948022111789456723 ) ) ;
#26036 = CARTESIAN_POINT ( 'NONE',  ( 116.0864081442453113, -0.1624402480850797581, -16.17319339645315424 ) ) ;
#26037 = VERTEX_POINT ( 'NONE', #26128 ) ;
#26038 = CARTESIAN_POINT ( 'NONE',  ( 64.58074566301215214, -15.42874415904032936, -10.76541893930477123 ) ) ;
#26039 = CARTESIAN_POINT ( 'NONE',  ( 115.0653281442453277, -6.344957434206662583, -7.627207830600332805 ) ) ;
#26040 = CIRCLE ( 'NONE', #34045, 3.853420195439741125 ) ;
#26041 = CARTESIAN_POINT ( 'NONE',  ( 107.4266296295248821, -4.863998795839590272, -8.388885654883775800 ) ) ;
#26042 = CARTESIAN_POINT ( 'NONE',  ( 119.1864297909088179, -1.016270020561755860, -17.26805140881366896 ) ) ;
#26043 = ORIENTED_EDGE ( 'NONE', *, *, #15813, .F. ) ;
#26044 = ORIENTED_EDGE ( 'NONE', *, *, #14805, .T. ) ;
#26045 = CARTESIAN_POINT ( 'NONE',  ( 123.0637881442452937, -8.899110576539710493, -16.42337572283490132 ) ) ;
#26046 = ADVANCED_FACE ( 'NONE', ( #36600 ), #32074, .T. ) ;
#26047 = CARTESIAN_POINT ( 'NONE',  ( 122.6667014775786413, -2.084020599724406786, -8.691656652584148546 ) ) ;
#26048 = CARTESIAN_POINT ( 'NONE',  ( 66.27237322303049893, -14.92696213753554524, -16.39321520033831447 ) ) ;
#26049 = ORIENTED_EDGE ( 'NONE', *, *, #8582, .T. ) ;
#26050 = CARTESIAN_POINT ( 'NONE',  ( 71.02242295334774269, -99.02728775972636299, -55.91838671430374319 ) ) ;
#26051 = CARTESIAN_POINT ( 'NONE',  ( 62.16333102610810357, -65.29371840568624918, -44.88093227629854454 ) ) ;
#26052 = CARTESIAN_POINT ( 'NONE',  ( 106.8015515045248378, -2.477300249445798297, -7.631215200338321125 ) ) ;
#26053 = VECTOR ( 'NONE', #23825, 999.9999999999998863 ) ;
#26054 = CARTESIAN_POINT ( 'NONE',  ( 115.7460481442453357, 0.9020085738987339008, -11.91225656197089222 ) ) ;
#26056 = CARTESIAN_POINT ( 'NONE',  ( 117.3343948109119737, -6.222761293078241884, -8.102969835052219238 ) ) ;
#26055 = CARTESIAN_POINT ( 'NONE',  ( 115.9729548109119861, -6.344957434206662583, -7.627207830600332805 ) ) ;
#26057 = CARTESIAN_POINT ( 'NONE',  ( 122.8936081442453059, -9.565557343593413364, -10.61323700422348004 ) ) ;
#26058 = CARTESIAN_POINT ( 'NONE',  ( 89.78938736644981589, -27.84333996136784961, -14.15691383771150136 ) ) ;
#26059 = EDGE_LOOP ( 'NONE', ( #20722, #7797 ) ) ;
#26060 = CARTESIAN_POINT ( 'NONE',  ( 120.1140014775786398, -7.894159318335828068, -9.358103419637847864 ) ) ;
#26061 = CARTESIAN_POINT ( 'NONE',  ( 125.2761281442453054, 0.4262465694468514643, -12.03445270309931736 ) ) ;
#26062 = CARTESIAN_POINT ( 'NONE',  ( 110.8992858795247827, -0.7896495226426338832, -17.46756447353520159 ) ) ;
#26063 = CARTESIAN_POINT ( 'NONE',  ( 114.1568685810857176, -1.220279397241700758, -16.99638242193885063 ) ) ;
#26064 = CARTESIAN_POINT ( 'NONE',  ( 112.8439733795247832, -8.938348069036489818, -17.46756447353520159 ) ) ;
#26065 = CARTESIAN_POINT ( 'NONE',  ( 119.9438214775786378, -7.893985811506177619, -18.51759400769804742 ) ) ;
#26066 = ORIENTED_EDGE ( 'NONE', *, *, #24861, .T. ) ;
#26067 = CARTESIAN_POINT ( 'NONE',  ( 122.2696148109119889, -4.089484607189486809, -7.948022111789456723 ) ) ;
#26068 = FACE_OUTER_BOUND ( 'NONE', #31802, .T. ) ;
#26069 = CARTESIAN_POINT ( 'NONE',  ( 107.4960827545248350, -2.477300249445798297, -19.15521520033831138 ) ) ;
#26070 = CARTESIAN_POINT ( 'NONE',  ( 114.9518748109119883, -1.834011780172310813, -8.268836392978581529 ) ) ;
#26071 = CARTESIAN_POINT ( 'NONE',  ( 116.1431348109119881, -10.30919188438810075, -12.61870101168855918 ) ) ;
#26072 = DIRECTION ( 'NONE',  ( 0.2407039305251456596, -0.3604685577742790525, 0.9011792478113757054 ) ) ;
#26073 = CARTESIAN_POINT ( 'NONE',  ( 117.1996198715402215, -11.04292984039206793, -5.371871346472351760 ) ) ;
#26074 = ORIENTED_EDGE ( 'NONE', *, *, #1650, .F. ) ;
#26075 = LINE ( 'NONE', #15816, #15737 ) ;
#26076 = CARTESIAN_POINT ( 'NONE',  ( 109.2295177676240456, -10.22869049659968610, -11.63402529915072492 ) ) ;
#26077 = CARTESIAN_POINT ( 'NONE',  ( 120.7379948109119709, 0.4262465694468514643, -12.03445270309931736 ) ) ;
#26078 = CARTESIAN_POINT ( 'NONE',  ( 111.5243640045248412, 0.1403307496149616695, -15.46607636864997204 ) ) ;
#26079 = CARTESIAN_POINT ( 'NONE',  ( 106.2459265045248173, -7.250697342233347165, -19.15521520033831138 ) ) ;
#26080 = CARTESIAN_POINT ( 'NONE',  ( 118.6391081442452986, -5.574606645277164318, -18.38911715685844683 ) ) ;
#26081 = CARTESIAN_POINT ( 'NONE',  ( 72.84358186299090221, -48.24900165852266554, -12.39321520033831447 ) ) ;
#26082 = CARTESIAN_POINT ( 'NONE',  ( 69.74921804855158314, -26.23096954073753651, -5.785566283887345840 ) ) ;
#26083 = CARTESIAN_POINT ( 'NONE',  ( 113.8740681442453138, -9.859900752359374465, -12.68260735090039404 ) ) ;
#26084 = CARTESIAN_POINT ( 'NONE',  ( 121.1350814775786233, 0.5811942927096110934, -14.16772938898807510 ) ) ;
#26085 = ORIENTED_EDGE ( 'NONE', *, *, #32840, .T. ) ;
#26086 = CARTESIAN_POINT ( 'NONE',  ( 116.8805814775786445, -3.505236298600246325, -18.68346056562440793 ) ) ;
#26087 = CARTESIAN_POINT ( 'NONE',  ( 114.1009748109119784, -4.089484607189486809, -7.948022111789456723 ) ) ;
#26088 = CARTESIAN_POINT ( 'NONE',  ( 120.4543614775786295, -4.089484607189486809, -7.948022111789456723 ) ) ;
#26089 = CONICAL_SURFACE ( 'NONE', #42106, 2.999999999999999556, 0.9599310885968830309 ) ;
#26090 = CARTESIAN_POINT ( 'NONE',  ( 121.6456214775786293, 0.4262465694468514643, -12.03445270309931736 ) ) ;
#26091 = ORIENTED_EDGE ( 'NONE', *, *, #31166, .T. ) ;
#26092 = CARTESIAN_POINT ( 'NONE',  ( 123.2339681442453241, -3.505236298600246325, -18.68346056562440793 ) ) ;
#26093 = CARTESIAN_POINT ( 'NONE',  ( 120.4543614775786295, -4.089484607189486809, -7.948022111789456723 ) ) ;
#26094 = CARTESIAN_POINT ( 'NONE',  ( 125.2183010572602768, -6.224655641565995268, -6.204738036994054795 ) ) ;
#26095 = CARTESIAN_POINT ( 'NONE',  ( 120.7379948109119709, -10.63000616557722466, -14.87417383870573495 ) ) ;
#26096 = CARTESIAN_POINT ( 'NONE',  ( 109.0240515045248202, -2.477300249445798297, -7.631215200338321125 ) ) ;
#26097 = CARTESIAN_POINT ( 'NONE',  ( 120.4379860609119675, -3.387241619883791355, -18.17469012370385073 ) ) ;
#26098 = CARTESIAN_POINT ( 'NONE',  ( 117.2294421295247844, 1.035107641088057973, -4.893215200338314474 ) ) ;
#26099 = CARTESIAN_POINT ( 'NONE',  ( 110.2047546295247855, -4.863998795839590272, -18.39754474579285315 ) ) ;
#26100 = FACE_OUTER_BOUND ( 'NONE', #23111, .T. ) ;
#26101 = FACE_OUTER_BOUND ( 'NONE', #5133, .T. ) ;
#26102 = CARTESIAN_POINT ( 'NONE',  ( 118.7525614775786380, -1.833838273342659253, -17.42832698103878286 ) ) ;
#26103 = CARTESIAN_POINT ( 'NONE',  ( 125.1626748109119802, -9.988377603198980381, -10.36322818467138518 ) ) ;
#26104 = CARTESIAN_POINT ( 'NONE',  ( 65.00799056132680676, -13.33714338733787663, -15.05121535635604779 ) ) ;
#26105 = ORIENTED_EDGE ( 'NONE', *, *, #27633, .T. ) ;
#26106 = CARTESIAN_POINT ( 'NONE',  ( 115.5958131642484545, -2.215723800389698184, -18.16877924232191788 ) ) ;
#26107 = CARTESIAN_POINT ( 'NONE',  ( 109.3713171295247832, 0.1403307496149613920, -13.39321520033831447 ) ) ;
#26108 = CARTESIAN_POINT ( 'NONE',  ( 114.8384214775786489, -10.15424416112533912, -14.75197769757731336 ) ) ;
#26109 = CARTESIAN_POINT ( 'NONE',  ( 77.25325688895158294, -4.012910213732562070, -18.64321520033831803 ) ) ;
#26110 = ADVANCED_FACE ( 'NONE', ( #25907 ), #19293, .T. ) ;
#26111 = CARTESIAN_POINT ( 'NONE',  ( 65.75155193749419880, -0.2203213019380833582, -10.39321520033831270 ) ) ;
#26112 = CARTESIAN_POINT ( 'NONE',  ( -1.971352495715082309, -6.875908495535235865, -18.85450084843566643 ) ) ;
#26114 = CARTESIAN_POINT ( 'NONE',  ( 124.4819548109119722, -7.893985811506177619, -18.51759400769804742 ) ) ;
#26113 = CARTESIAN_POINT ( 'NONE',  ( 71.48339778575683567, -26.67534733500407640, -5.037593897558821254 ) ) ;
#26115 = VECTOR ( 'NONE', #2462, 1000.000000000000000 ) ;
#26116 = CARTESIAN_POINT ( 'NONE',  ( 123.8579614775786126, -9.859900752359378018, -12.68260735090039759 ) ) ;
#26117 = EDGE_LOOP ( 'NONE', ( #15308, #25741 ) ) ;
#26118 = CARTESIAN_POINT ( 'NONE',  ( 69.69189222815028018, -41.76310523276638520, -15.89321520033831447 ) ) ;
#26119 = DIRECTION ( 'NONE',  ( 1.000000000000000000, 0.000000000000000000, 0.000000000000000000 ) ) ;
#26120 = CARTESIAN_POINT ( 'NONE',  ( 110.7603796295247918, -4.863998795839590272, -8.388885654883775800 ) ) ;
#26121 = CARTESIAN_POINT ( 'NONE',  ( 124.5954081442453116, -6.222761293078241884, -8.102969835052219238 ) ) ;
#26122 = CARTESIAN_POINT ( 'NONE',  ( 120.1140014775786398, -7.894159318335828068, -9.358103419637847864 ) ) ;
#26123 = CARTESIAN_POINT ( 'NONE',  ( 118.5823814775786360, -7.643976991954077427, -18.09477374809248928 ) ) ;
#26124 = CARTESIAN_POINT ( 'NONE',  ( 125.3566265649659357, 1.247438245257331157, -16.90339198053782610 ) ) ;
#26125 = CARTESIAN_POINT ( 'NONE',  ( 106.6626452545248611, 0.8980012041604421569, -11.00651665394454071 ) ) ;
#26126 = DIRECTION ( 'NONE',  ( -0.6049664196031393493, 0.7962509850245451659, 0.000000000000000000 ) ) ;
#26127 = CARTESIAN_POINT ( 'NONE',  ( 115.5566632127138575, -2.191907684172563986, -18.20049396185734025 ) ) ;
#26128 = CARTESIAN_POINT ( 'NONE',  ( 67.30914723170953096, -51.17274647505311691, -34.56643725558897273 ) ) ;
#26129 = CARTESIAN_POINT ( 'NONE',  ( 108.6767858795247861, -0.7896495226426338832, -17.46756447353520159 ) ) ;
#26130 = EDGE_CURVE ( 'NONE', #3693, #408, #1948, .T. ) ;
#26131 = DIRECTION ( 'NONE',  ( 1.000000000000000000, 0.000000000000000000, -0.000000000000000000 ) ) ;
#26132 = CARTESIAN_POINT ( 'NONE',  ( 84.10271796608054728, -31.10763468207608895, -20.89321520033831447 ) ) ;
#26133 = CARTESIAN_POINT ( 'NONE',  ( 122.3830681442452857, -8.166667518702819706, -8.995218007635861213 ) ) ;
#26134 = CARTESIAN_POINT ( 'NONE',  ( 119.2631014775786298, 0.2603800115204892296, -16.42320221600525088 ) ) ;
#26135 = CARTESIAN_POINT ( 'NONE',  ( 106.2459265045248173, -7.250697342233347165, -19.15521520033831138 ) ) ;
#26136 = CARTESIAN_POINT ( 'NONE',  ( 118.2420214775786320, -3.383040157471821630, -19.15922257007629170 ) ) ;
#26137 = EDGE_CURVE ( 'NONE', #23958, #37519, #19710, .T. ) ;
#26138 = EDGE_CURVE ( 'NONE', #26479, #2604, #12457, .T. ) ;
#26139 = CARTESIAN_POINT ( 'NONE',  ( 74.82520252044861309, -48.51951888521425360, -12.39321520033831447 ) ) ;
#26140 = ORIENTED_EDGE ( 'NONE', *, *, #9691, .T. ) ;
#26141 = CARTESIAN_POINT ( 'NONE',  ( 112.1114130180079798, 0.7607806665037644134, -14.64321520033833046 ) ) ;
#26142 = CARTESIAN_POINT ( 'NONE',  ( 123.5176014775786228, -9.261995988541697145, -16.69588392320189030 ) ) ;
#26143 = CARTESIAN_POINT ( 'NONE',  ( 120.8514481442452961, -7.893985811506177619, -18.51759400769804742 ) ) ;
#26144 = CARTESIAN_POINT ( 'NONE',  ( 126.6375681442452930, -10.15424416112533912, -14.75197769757731336 ) ) ;
#26145 = CONTEXT_DEPENDENT_SHAPE_REPRESENTATION ( #21294, #26733 ) ;
#26146 = CARTESIAN_POINT ( 'NONE',  ( 114.2711548109119803, -0.1624402480850797581, -16.17319339645315424 ) ) ;
#26147 = CARTESIAN_POINT ( 'NONE',  ( 126.2404814775786264, -9.261995988541697145, -16.69588392320189030 ) ) ;
#26148 = CARTESIAN_POINT ( 'NONE',  ( 109.7880358795247986, -0.7896495226426338832, -17.46756447353520159 ) ) ;
#26149 = CARTESIAN_POINT ( 'NONE',  ( 120.2841814775786276, -10.15424416112533912, -14.75197769757731336 ) ) ;
#26150 = CARTESIAN_POINT ( 'NONE',  ( 110.8298327545248299, -2.477300249445798297, -19.15521520033832203 ) ) ;
#26151 = DIRECTION ( 'NONE',  ( 0.000000000000000000, 0.6004852223388323917, -0.7996358532186279566 ) ) ;
#26152 = ORIENTED_EDGE ( 'NONE', *, *, #34810, .F. ) ;
#26153 = CARTESIAN_POINT ( 'NONE',  ( 94.20708369096698220, -25.14343533174585943, -14.10537061818067883 ) ) ;
#26154 = CARTESIAN_POINT ( 'NONE',  ( 121.4754414775786131, -8.166667518702819706, -8.995218007635861213 ) ) ;
#26155 = ADVANCED_FACE ( 'NONE', ( #29771 ), #25685, .F. ) ;
#26156 = LINE ( 'NONE', #42593, #34922 ) ;
#26157 = CARTESIAN_POINT ( 'NONE',  ( 124.0650380271158042, 2.250018580934641577, -9.733962076267653529 ) ) ;
#26158 = FACE_OUTER_BOUND ( 'NONE', #24031, .T. ) ;
#26159 = CARTESIAN_POINT ( 'NONE',  ( 118.8092881442453290, -0.1624402480850797581, -16.17319339645315424 ) ) ;
#26160 = CARTESIAN_POINT ( 'NONE',  ( 68.14371629974728251, -1.351251493923715685, -16.39321520033831447 ) ) ;
#26161 = CYLINDRICAL_SURFACE ( 'NONE', #41324, 1.999999999999998890 ) ;
#26162 =( BOUNDED_CURVE ( )  B_SPLINE_CURVE ( 2, ( #16073, #9686, #20406, #30432, #37488, #16535, #40474, #30882, #2603, #43894, #9455, #9235, #23144 ),
 .UNSPECIFIED., .F., .T. ) 
 B_SPLINE_CURVE_WITH_KNOTS ( ( 3, 2, 2, 2, 2, 2, 3 ),
 ( 0.8921282416568590001, 0.8984375000000000000, 0.9062500000000000000, 0.9140625000000000000, 0.9218750000000000000, 0.9296875000000000000, 0.9375000000000000000 ),
 .UNSPECIFIED. ) 
 CURVE ( )  GEOMETRIC_REPRESENTATION_ITEM ( )  RATIONAL_B_SPLINE_CURVE ( ( 0.9763430640195950305, 0.9385262470928690259, 1.000000000000000000, 0.9238795325112869605, 1.000000000000000000, 0.9238795325112869605, 1.000000000000000000, 0.9238795325112869605, 1.000000000000000000, 0.9238795325112869605, 1.000000000000000000, 0.9238795325112479917, 1.000000000000039968 ) ) 
 REPRESENTATION_ITEM ( '' )  );
#26163 = EDGE_CURVE ( 'NONE', #4027, #12184, #18834, .T. ) ;
#26164 = CARTESIAN_POINT ( 'NONE',  ( 124.0848681442452772, -5.574606645277164318, -18.38911715685844683 ) ) ;
#26165 = CARTESIAN_POINT ( 'NONE',  ( 109.8889130180080826, 0.7607806665037644134, -14.64321520033833579 ) ) ;
#26166 = LINE ( 'NONE', #32545, #35452 ) ;
#26167 = EDGE_CURVE ( 'NONE', #41698, #17138, #13660, .T. ) ;
#26168 = DIRECTION ( 'NONE',  ( 0.000000000000000000, -0.4669533266896290225, -0.8842819633428516957 ) ) ;
#26169 = CARTESIAN_POINT ( 'NONE',  ( 123.2339681442453241, -6.344957434206665248, -7.627207830600338134 ) ) ;
#26170 = CARTESIAN_POINT ( 'NONE',  ( 116.0296814775786345, -1.833838273342658809, -17.42832698103878286 ) ) ;
#26171 = CARTESIAN_POINT ( 'NONE',  ( 123.6310548109119765, -4.153390946401325223, -8.397313243818185668 ) ) ;
#26172 = ORIENTED_EDGE ( 'NONE', *, *, #7485, .T. ) ;
#26173 = CARTESIAN_POINT ( 'NONE',  ( 122.6099748109119929, -9.261995988541697145, -16.69588392320189030 ) ) ;
#26174 = CARTESIAN_POINT ( 'NONE',  ( 114.6682414775786469, -1.561330072975668060, -17.79121239304076596 ) ) ;
#26175 = CARTESIAN_POINT ( 'NONE',  ( 114.6497546295247929, -4.863998795839590272, -18.39754474579285315 ) ) ;
#26176 = CARTESIAN_POINT ( 'NONE',  ( 119.7434548109119703, 0.04957186715663641774, -7.079989135975798931 ) ) ;
#26177 = CARTESIAN_POINT ( 'NONE',  ( 125.9568481442452850, -3.505236298600246325, -18.68346056562440793 ) ) ;
#26178 = CARTESIAN_POINT ( 'NONE',  ( 121.7023481442452777, -9.261995988541697145, -16.69588392320189030 ) ) ;
#26179 = CARTESIAN_POINT ( 'NONE',  ( 115.6915515045247531, -2.477300249445798297, -7.631215200338321125 ) ) ;
#26180 = CARTESIAN_POINT ( 'NONE',  ( 107.8433483795247838, -8.402594152722688392, -16.93181055722141792 ) ) ;
#26181 = DIRECTION ( 'NONE',  ( 0.000000000000000000, -0.3818493186865936084, 0.9242245927363024194 ) ) ;
#26182 = CARTESIAN_POINT ( 'NONE',  ( 113.3635281442453504, -0.1624402480850797581, -16.17319339645315424 ) ) ;
#26183 = VECTOR ( 'NONE', #34968, 1000.000000000000000 ) ;
#26184 = CARTESIAN_POINT ( 'NONE',  ( 120.8160396737536928, -8.611453504372539314, -17.77011218421760574 ) ) ;
#26185 = CARTESIAN_POINT ( 'NONE',  ( 114.9970202545248412, 0.1403307496149616695, -11.32035403202665336 ) ) ;
#26186 = ORIENTED_EDGE ( 'NONE', *, *, #29029, .F. ) ;
#26187 = CARTESIAN_POINT ( 'NONE',  ( 125.5030348109119558, -6.222761293078241884, -8.102969835052219238 ) ) ;
#26188 = CARTESIAN_POINT ( 'NONE',  ( 122.5215798109119874, -2.173413727453600508, -8.297982527556802879 ) ) ;
#26189 = CARTESIAN_POINT ( 'NONE',  ( 123.0772048109119652, -7.554583864224885481, -18.48844787311982785 ) ) ;
#26190 = ADVANCED_FACE ( 'NONE', ( #16326 ), #37509, .F. ) ;
#26191 = ADVANCED_FACE ( 'NONE', ( #2854 ), #24694, .T. ) ;
#26192 = LINE ( 'NONE', #32569, #34089 ) ;
#26193 = CARTESIAN_POINT ( 'NONE',  ( 107.7738952545248310, -9.868328341294098749, -15.46607636864997204 ) ) ;
#26194 = VERTEX_POINT ( 'NONE', #42406 ) ;
#26195 = CARTESIAN_POINT ( 'NONE',  ( 119.6601881442453106, -8.166667518702819706, -8.995218007635861213 ) ) ;
#26196 = CARTESIAN_POINT ( 'NONE',  ( 112.9664414775786412, 0.5811942927096110934, -14.16772938898807510 ) ) ;
#26197 = CARTESIAN_POINT ( 'NONE',  ( 123.1205148109119563, -7.643976991954077427, -18.09477374809248928 ) ) ;
#26198 = CARTESIAN_POINT ( 'NONE',  ( 114.2144281442453178, -1.833838273342658809, -17.42832698103878286 ) ) ;
#26199 = CIRCLE ( 'NONE', #5094, 1.587500000000001021 ) ;
#26200 = DIRECTION ( 'NONE',  ( -0.000000000000000000, -0.9284778069183718952, -0.3713878862591649677 ) ) ;
#26201 = CARTESIAN_POINT ( 'NONE',  ( 85.75809888461174069, -18.45227461768569199, -4.893215200338314474 ) ) ;
#26202 = CARTESIAN_POINT ( 'NONE',  ( 114.3846081442453197, -10.63000616557722466, -14.87417383870573495 ) ) ;
#26203 = CARTESIAN_POINT ( 'NONE',  ( 112.2188952545247531, -9.868328341294098749, -15.46607636864997204 ) ) ;
#26204 = CARTESIAN_POINT ( 'NONE',  ( 124.2550481442452792, -9.988377603198980381, -10.36322818467138518 ) ) ;
#26205 = CARTESIAN_POINT ( 'NONE',  ( 78.69189222814998175, -59.27884951796255564, -42.87418841894956500 ) ) ;
#26206 = ORIENTED_EDGE ( 'NONE', *, *, #796, .T. ) ;
#26207 = CARTESIAN_POINT ( 'NONE',  ( 113.3635281442453504, -9.988377603198976828, -10.36322818467138340 ) ) ;
#26208 = CARTESIAN_POINT ( 'NONE',  ( 114.2711548109119803, -0.1624402480850797581, -16.17319339645315424 ) ) ;
#26209 = FACE_OUTER_BOUND ( 'NONE', #36303, .T. ) ;
#26210 = CARTESIAN_POINT ( 'NONE',  ( 113.0798948109119948, -0.4660016031367893996, -10.09054647747474043 ) ) ;
#26211 = ORIENTED_EDGE ( 'NONE', *, *, #27392, .T. ) ;
#26212 = CARTESIAN_POINT ( 'NONE',  ( 117.2209414775786485, -7.893985811506177619, -18.51759400769804742 ) ) ;
#26213 = CONICAL_SURFACE ( 'NONE', #43697, 2.999999999999999556, 0.9599310885968830309 ) ;
#26214 = CARTESIAN_POINT ( 'NONE',  ( 88.46631044337289040, -25.99489077589524300, -13.39321520033831625 ) ) ;
#26215 = CARTESIAN_POINT ( 'NONE',  ( 115.9328453070359046, -1.196538596002799215, -17.02799684832027083 ) ) ;
#26216 = CARTESIAN_POINT ( 'NONE',  ( 111.7751814775786556, -2.084020599724394796, -8.691656652584146769 ) ) ;
#26217 = CARTESIAN_POINT ( 'NONE',  ( 112.5352875888224133, -2.372251574601220270, -17.96033910819751966 ) ) ;
#26218 = CARTESIAN_POINT ( 'NONE',  ( 115.0086014775786509, -5.574606645277164318, -18.38911715685844683 ) ) ;
#26219 = DIRECTION ( 'NONE',  ( 0.000000000000000000, 0.000000000000000000, -1.000000000000000000 ) ) ;
#26220 = CARTESIAN_POINT ( 'NONE',  ( 121.2141330209070276, -6.157706758239399392, -18.56290235964623392 ) ) ;
#26221 = CARTESIAN_POINT ( 'NONE',  ( 111.3780948109119890, -5.574606645277164318, -18.38911715685844683 ) ) ;
#26222 = AXIS2_PLACEMENT_3D ( 'NONE', #21897, #42654, #10970 ) ;
#26223 = CARTESIAN_POINT ( 'NONE',  ( 126.1270281442452870, 0.1319031606808879209, -14.10382304977623669 ) ) ;
#26224 = CARTESIAN_POINT ( 'NONE',  ( 122.7993923109119692, -0.4387604401700512802, -15.73000352943951619 ) ) ;
#26225 = CARTESIAN_POINT ( 'NONE',  ( 125.5030348109119558, -6.222761293078241884, -8.102969835052219238 ) ) ;
#26226 = CARTESIAN_POINT ( 'NONE',  ( 113.0798948109119948, -8.899110576539710493, -16.42337572283490132 ) ) ;
#26227 = CARTESIAN_POINT ( 'NONE',  ( 122.0427081442452817, 0.5811942927096110934, -14.16772938898807510 ) ) ;
#26228 = EDGE_CURVE ( 'NONE', #31092, #9213, #40859, .T. ) ;
#26229 = CARTESIAN_POINT ( 'NONE',  ( 123.0070614775786169, 0.9020085738987339008, -11.91225656197089222 ) ) ;
#26230 = EDGE_LOOP ( 'NONE', ( #37890, #19678, #23498, #41593 ) ) ;
#26231 = CARTESIAN_POINT ( 'NONE',  ( 127.7617783745704543, -8.479500832906602170, -17.89265013408903471 ) ) ;
#26232 = CARTESIAN_POINT ( 'NONE',  ( 109.8574890045247940, 0.8980012041604421569, -15.77991374673208469 ) ) ;
#26233 = CARTESIAN_POINT ( 'NONE',  ( 111.7327233795247849, -1.325403438956436419, -9.854619843455211026 ) ) ;
#26234 = CARTESIAN_POINT ( 'NONE',  ( 107.2877233795247776, -1.325403438956436419, -9.854619843455211026 ) ) ;
#26235 = FACE_OUTER_BOUND ( 'NONE', #14770, .T. ) ;
#26236 = CARTESIAN_POINT ( 'NONE',  ( 115.3489614775786407, -9.261995988541697145, -16.69588392320189030 ) ) ;
#26237 = ORIENTED_EDGE ( 'NONE', *, *, #1684, .T. ) ;
#26238 = CARTESIAN_POINT ( 'NONE',  ( 125.3328548109119964, -9.261995988541697145, -16.69588392320189030 ) ) ;
#26239 = CARTESIAN_POINT ( 'NONE',  ( 60.53937939559665438, -4.256997083809236138, 68.32805411424035924 ) ) ;
#26240 = DIRECTION ( 'NONE',  ( 0.8636456077245090457, -0.5040994586965586999, 0.000000000000000000 ) ) ;
#26241 = CARTESIAN_POINT ( 'NONE',  ( 113.3068014775786594, -1.833838273342658809, -17.42832698103878286 ) ) ;
#26242 = CARTESIAN_POINT ( 'NONE',  ( 120.9649014775786355, -3.383040157471821630, -19.15922257007629170 ) ) ;
#26243 = CARTESIAN_POINT ( 'NONE',  ( 108.8851452545248151, 0.8980012041604421569, -11.00651665394454071 ) ) ;
#26244 = CARTESIAN_POINT ( 'NONE',  ( 84.49707967414211396, -24.14644159042263993, -12.62951656296512937 ) ) ;
#26245 = ORIENTED_EDGE ( 'NONE', *, *, #42975, .F. ) ;
#26246 = CARTESIAN_POINT ( 'NONE',  ( 42.36021970110777346, -12.73296999994090584, -8.893215200338314474 ) ) ;
#26247 = CARTESIAN_POINT ( 'NONE',  ( 118.8092881442453290, -0.1624402480850797581, -16.17319339645315424 ) ) ;
#26248 = CARTESIAN_POINT ( 'NONE',  ( 118.8660148109119774, -10.30919188438810075, -12.61870101168855918 ) ) ;
#26249 = CYLINDRICAL_SURFACE ( 'NONE', #10185, 3.000000000000001776 ) ;
#26250 = SHAPE_REPRESENTATION ( 'Cable Anchor', ( #12375 ), #18656 ) ;
#26251 = CARTESIAN_POINT ( 'NONE',  ( 113.9307948109119906, 0.9020085738987339008, -11.91225656197089222 ) ) ;
#26252 = CARTESIAN_POINT ( 'NONE',  ( 71.02242295334774269, -99.02728775972636299, -55.91838671430374319 ) ) ;
#26253 = EDGE_CURVE ( 'NONE', #31317, #15833, #33525, .T. ) ;
#26254 = CARTESIAN_POINT ( 'NONE',  ( 123.9714148109119805, -8.899110576539710493, -16.42337572283490132 ) ) ;
#26255 = CARTESIAN_POINT ( 'NONE',  ( 120.9081748109119872, -4.153390946401325223, -8.397313243818185668 ) ) ;
#26256 = ORIENTED_EDGE ( 'NONE', *, *, #14510, .T. ) ;
#26257 = CARTESIAN_POINT ( 'NONE',  ( 121.6186891859119896, -8.844754642576884152, -8.592115655440050404 ) ) ;
#26258 = AXIS2_PLACEMENT_3D ( 'NONE', #2856, #23858, #30229 ) ;
#26259 = B_SPLINE_CURVE_WITH_KNOTS ( 'NONE', 3,
 ( #15345, #8505, #9631, #41110, #44073, #1867, #5969, #6205, #37435, #5739 ),
 .UNSPECIFIED., .F., .F.,
 ( 4, 3, 3, 4 ),
 ( 4.336808689942019662E-19, 0.0001671877548681264863, 0.0003343755096277665107, 0.0006463528481650619413 ),
 .UNSPECIFIED. ) ;
#26260 = FACE_OUTER_BOUND ( 'NONE', #11604, .T. ) ;
#26261 = CARTESIAN_POINT ( 'NONE',  ( 123.0637881442452937, -8.899110576539710493, -16.42337572283490132 ) ) ;
#26262 = VERTEX_POINT ( 'NONE', #35766 ) ;
#26263 = VECTOR ( 'NONE', #22125, 1000.000000000000227 ) ;
#26264 = CARTESIAN_POINT ( 'NONE',  ( 123.2161110609119703, -6.340755971794695078, -8.611740276972781771 ) ) ;
#26265 = CARTESIAN_POINT ( 'NONE',  ( 115.5758681442453053, -1.561330072975668060, -17.79121239304076951 ) ) ;
#26266 = CARTESIAN_POINT ( 'NONE',  ( 113.9552233795247815, -8.938348069036489818, -17.46756447353520159 ) ) ;
#26267 = CARTESIAN_POINT ( 'NONE',  ( 115.9162281442453235, -5.574606645277164318, -18.38911715685844683 ) ) ;
#26268 = ORIENTED_EDGE ( 'NONE', *, *, #40638, .F. ) ;
#26269 = ORIENTED_EDGE ( 'NONE', *, *, #25758, .T. ) ;
#26270 = CARTESIAN_POINT ( 'NONE',  ( 123.6310548109119765, -4.153390946401325223, -8.397313243818185668 ) ) ;
#26271 = B_SPLINE_CURVE_WITH_KNOTS ( 'NONE', 3,
 ( #20930, #4487, #39146, #21818, #35712, #18408, #14980, #31398, #42805, #38239 ),
 .UNSPECIFIED., .F., .F.,
 ( 4, 3, 3, 4 ),
 ( 0.000000000000000000, 0.0001671877560958109985, 0.0003343755126086590075, 0.0006438490228505489759 ),
 .UNSPECIFIED. ) ;
#26272 = CARTESIAN_POINT ( 'NONE',  ( 120.0572748109119772, -6.222761293078241884, -8.102969835052219238 ) ) ;
#26273 = FILL_AREA_STYLE_COLOUR ( '', #33829 ) ;
#26274 = ORIENTED_EDGE ( 'NONE', *, *, #216, .F. ) ;
#26275 = DIRECTION ( 'NONE',  ( 0.000000000000000000, 0.000000000000000000, -1.000000000000000000 ) ) ;
#26276 = CARTESIAN_POINT ( 'NONE',  ( 120.0005481442453146, -5.638512984488999180, -18.83840828888717311 ) ) ;
#26277 = CARTESIAN_POINT ( 'NONE',  ( 105.8986608795248401, -8.938348069036489818, -9.318865927141430916 ) ) ;
#26278 = AXIS2_PLACEMENT_3D ( 'NONE', #32109, #21184, #41943 ) ;
#26279 = CARTESIAN_POINT ( 'NONE',  ( 117.1074881442453233, -10.63000616557722466, -14.87417383870573495 ) ) ;
#26281 = CARTESIAN_POINT ( 'NONE',  ( 116.0296814775786345, -1.833838273342658809, -17.42832698103878286 ) ) ;
#26280 = CARTESIAN_POINT ( 'NONE',  ( 116.4267681442453153, -3.383040157471821630, -19.15922257007629170 ) ) ;
#26282 = CARTESIAN_POINT ( 'NONE',  ( 121.1918081442452859, -10.15424416112533912, -14.75197769757731336 ) ) ;
#26283 = CARTESIAN_POINT ( 'NONE',  ( 113.4202548109119846, -10.30919188438810075, -12.61870101168855918 ) ) ;
#26284 = VERTEX_POINT ( 'NONE', #29160 ) ;
#26285 = CARTESIAN_POINT ( 'NONE',  ( 119.3765548109119834, -10.15424416112533912, -14.75197769757731336 ) ) ;
#26286 = CARTESIAN_POINT ( 'NONE',  ( 113.7805598309151236, -2.215723800389698184, -18.16877924232191788 ) ) ;
#26287 = CARTESIAN_POINT ( 'NONE',  ( 112.4967077545247633, -7.250697342233347165, -7.631215200338321125 ) ) ;
#26288 = AXIS2_PLACEMENT_3D ( 'NONE', #44946, #31236, #36995 ) ;
#26289 = FACE_OUTER_BOUND ( 'NONE', #25158, .T. ) ;
#26290 = CARTESIAN_POINT ( 'NONE',  ( 113.8857702545248003, -10.62599879583958717, -15.77991374673208469 ) ) ;
#26291 = CARTESIAN_POINT ( 'NONE',  ( 120.0572748109119772, -3.383040157471821630, -19.15922257007629170 ) ) ;
#26292 = VERTEX_POINT ( 'NONE', #8193 ) ;
#26293 = AXIS2_PLACEMENT_3D ( 'NONE', #15735, #22566, #44010 ) ;
#26294 = CARTESIAN_POINT ( 'NONE',  ( 121.1918081442452859, 0.9020085738987339008, -11.91225656197089222 ) ) ;
#26295 = CARTESIAN_POINT ( 'NONE',  ( 63.10563328194941590, -37.74164650239046637, -4.980946376743919046 ) ) ;
#26296 = CARTESIAN_POINT ( 'NONE',  ( 107.7044421295247929, 0.8980012041604618078, -13.39321520033831447 ) ) ;
#26297 = CARTESIAN_POINT ( 'NONE',  ( 119.8870948109119752, -9.261995988541697145, -16.69588392320189030 ) ) ;
#26298 = CARTESIAN_POINT ( 'NONE',  ( 117.7314814775786260, -4.089484607189486809, -7.948022111789456723 ) ) ;
#26299 = DIRECTION ( 'NONE',  ( 0.000000000000000000, 1.000000000000000000, 0.000000000000000000 ) ) ;
#26300 = CARTESIAN_POINT ( 'NONE',  ( 116.9233217481409355, -11.60109430213782744, -5.955714001824102155 ) ) ;
#26301 = ORIENTED_EDGE ( 'NONE', *, *, #8889, .T. ) ;
#26302 = DIRECTION ( 'NONE',  ( -0.8636456077245080465, 0.5040994586965603652, 0.000000000000000000 ) ) ;
#26303 = CARTESIAN_POINT ( 'NONE',  ( 109.2294327885794161, -10.27098468477303150, -14.50962478522546739 ) ) ;
#26304 = CARTESIAN_POINT ( 'NONE',  ( 121.5321681442453183, -0.1624402480850797581, -16.17319339645315424 ) ) ;
#26305 = EDGE_CURVE ( 'NONE', #34946, #17270, #25546, .T. ) ;
#26306 = CARTESIAN_POINT ( 'NONE',  ( 112.2883483795247770, -8.402594152722688392, -16.93181055722141792 ) ) ;
#26307 = CARTESIAN_POINT ( 'NONE',  ( 109.3713171295247832, 0.1403307496149613920, -13.39321520033831447 ) ) ;
#26308 = CARTESIAN_POINT ( 'NONE',  ( 119.3198281442452924, -9.859900752359374465, -12.68260735090039404 ) ) ;
#26309 = DIRECTION ( 'NONE',  ( -1.000000000000000000, 0.000000000000000000, 0.000000000000000000 ) ) ;
#26310 = CARTESIAN_POINT ( 'NONE',  ( 71.33058836615619214, -26.45114454543378812, -5.217245182119505387 ) ) ;
#26311 = CARTESIAN_POINT ( 'NONE',  ( 113.6471614775786492, -4.153390946401321671, -8.397313243818183892 ) ) ;
#26312 = CARTESIAN_POINT ( 'NONE',  ( 122.7234281442452755, -5.638512984488999180, -18.83840828888717311 ) ) ;
#26313 = ORIENTED_EDGE ( 'NONE', *, *, #15439, .T. ) ;
#26314 = CARTESIAN_POINT ( 'NONE',  ( 121.0783548109119749, -9.565557343593413364, -10.61323700422348004 ) ) ;
#26315 = CARTESIAN_POINT ( 'NONE',  ( 114.9518748109119883, -1.834011780172310813, -8.268836392978581529 ) ) ;
#26316 = CIRCLE ( 'NONE', #37965, 1.499999999999998002 ) ;
#26317 = CARTESIAN_POINT ( 'NONE',  ( 120.5110881442453206, -6.344957434206665248, -7.627207830600338134 ) ) ;
#26318 = CARTESIAN_POINT ( 'NONE',  ( 122.0994348109119443, -10.15424416112533912, -14.75197769757731336 ) ) ;
#26319 = ORIENTED_EDGE ( 'NONE', *, *, #17516, .F. ) ;
#26320 = CARTESIAN_POINT ( 'NONE',  ( 125.3328548109119964, -0.8288870151387760510, -10.36305467784173118 ) ) ;
#26321 = AXIS2_PLACEMENT_3D ( 'NONE', #15300, #8008, #36037 ) ;
#26322 = CARTESIAN_POINT ( 'NONE',  ( 122.4965214775786251, -10.30919188438810075, -12.61870101168855918 ) ) ;
#26323 = EDGE_CURVE ( 'NONE', #37706, #42269, #22101, .T. ) ;
#26324 = DIRECTION ( 'NONE',  ( 1.000000000000000000, 0.000000000000000000, 0.000000000000000000 ) ) ;
#26325 = CARTESIAN_POINT ( 'NONE',  ( 111.4915481442453142, -1.833838273342658365, -17.42832698103878286 ) ) ;
#26326 = CARTESIAN_POINT ( 'NONE',  ( 105.8292077545248446, -7.250697342233347165, -7.631215200338321125 ) ) ;
#26327 = DIRECTION ( 'NONE',  ( 0.000000000000000000, -0.3818493186865936084, 0.9242245927363024194 ) ) ;
#26328 = CARTESIAN_POINT ( 'NONE',  ( 69.69189222814998175, -41.76310523276723785, -47.71602681600972318 ) ) ;
#26329 = CARTESIAN_POINT ( 'NONE',  ( 111.3854577545248645, -2.791137627527939813, -18.39754474579286025 ) ) ;
#26330 = CARTESIAN_POINT ( 'NONE',  ( 122.8688454359119646, 0.5291689781388270175, -13.89700978578772705 ) ) ;
#26331 = CARTESIAN_POINT ( 'NONE',  ( 137.3930029278077427, -9.820525849186804379, -12.08282185636668338 ) ) ;
#26332 = CARTESIAN_POINT ( 'NONE',  ( 118.4689281442453392, -10.15424416112533912, -14.75197769757731336 ) ) ;
#26333 = CARTESIAN_POINT ( 'NONE',  ( 124.1415948109119540, -6.344957434206665248, -7.627207830600338134 ) ) ;
#26334 = CARTESIAN_POINT ( 'NONE',  ( 75.95778847736481509, -3.256761025687722189, -9.893215200338316251 ) ) ;
#26335 = ORIENTED_EDGE ( 'NONE', *, *, #44279, .F. ) ;
#26336 = CARTESIAN_POINT ( 'NONE',  ( 116.5249890045247980, -9.868328341294098749, -11.32035403202665869 ) ) ;
#26337 = CARTESIAN_POINT ( 'NONE',  ( 107.7738952545248310, -9.868328341294098749, -15.46607636864997204 ) ) ;
#26338 = CARTESIAN_POINT ( 'NONE',  ( 117.7314814775786260, -5.574606645277164318, -18.38911715685844683 ) ) ;
#26339 = CARTESIAN_POINT ( 'NONE',  ( 114.8340781407226103, -1.081026697600512732, -17.18181821144401056 ) ) ;
#26340 = B_SPLINE_CURVE_WITH_KNOTS ( 'NONE', 3,
 ( #38205, #7192, #3765, #44397, #13161, #27062, #14489, #21782, #39334, #580 ),
 .UNSPECIFIED., .F., .F.,
 ( 4, 3, 3, 4 ),
 ( 0.000000000000000000, 0.0001671877560958105107, 0.0003343755126086565138, 0.0006438490228505459401 ),
 .UNSPECIFIED. ) ;
#26342 = CIRCLE ( 'NONE', #6702, 1.587500000000000355 ) ;
#26341 = CARTESIAN_POINT ( 'NONE',  ( 65.97129655291890060, -0.1603451389117774017, -10.39321520033831270 ) ) ;
#26343 = CARTESIAN_POINT ( 'NONE',  ( 122.7660347346423180, -8.435056900666539903, -17.43606523319152757 ) ) ;
#26345 = CARTESIAN_POINT ( 'NONE',  ( 122.8936081442453059, 0.2603800115204892296, -16.42320221600525088 ) ) ;
#26344 = DIRECTION ( 'NONE',  ( -0.9908103287288505534, 0.1352586133457950868, 0.000000000000000000 ) ) ;
#26346 = CARTESIAN_POINT ( 'NONE',  ( 123.4608748109119745, 0.4262465694468514643, -12.03445270309931736 ) ) ;
#26347 = VERTEX_POINT ( 'NONE', #18682 ) ;
#26348 = CARTESIAN_POINT ( 'NONE',  ( 111.7751814775786556, -7.893985811506177619, -18.51759400769804742 ) ) ;
#26349 = CARTESIAN_POINT ( 'NONE',  ( 66.30460113213176498, -14.82332738410570805, -10.39321520033831092 ) ) ;
#26350 = CARTESIAN_POINT ( 'NONE',  ( 109.3018640045248304, 0.1403307496149616695, -15.46607636864997204 ) ) ;
#26351 = CARTESIAN_POINT ( 'NONE',  ( 120.8514481442452961, -2.084020599724406786, -8.691656652584148546 ) ) ;
#26352 = CARTESIAN_POINT ( 'NONE',  ( 121.7590748109119687, -2.084020599724406786, -8.691656652584148546 ) ) ;
#26353 = CARTESIAN_POINT ( 'NONE',  ( 119.6026285810857104, -1.220279397241718966, -16.99638242193886484 ) ) ;
#26354 = CARTESIAN_POINT ( 'NONE',  ( 105.9681140045248355, -10.62599879583958717, -11.00651665394454604 ) ) ;
#26355 = CONICAL_SURFACE ( 'NONE', #14705, 5.000000000000000888, 0.7853981633974419507 ) ;
#26356 = CARTESIAN_POINT ( 'NONE',  ( 116.5969481442453031, 0.5811942927096102052, -14.16772938898808221 ) ) ;
#26357 = FACE_OUTER_BOUND ( 'NONE', #8652, .T. ) ;
#26358 = DIRECTION ( 'NONE',  ( 4.295035233247849253E-16, 0.3713878862591650232, -0.9284778069183718952 ) ) ;
#26359 = CARTESIAN_POINT ( 'NONE',  ( 113.0523327545247838, -2.477300249445798297, -19.15521520033831138 ) ) ;
#26360 = CARTESIAN_POINT ( 'NONE',  ( -13.32377113153209791, -5.100909530930219482, -19.39321520033831803 ) ) ;
#26361 = CARTESIAN_POINT ( 'NONE',  ( 115.7610046295247912, -4.863998795839590272, -7.631215200338315796 ) ) ;
#26362 = CARTESIAN_POINT ( 'NONE',  ( 122.0427081442452817, 0.5811942927096110934, -14.16772938898807510 ) ) ;
#26363 = CARTESIAN_POINT ( 'NONE',  ( 121.1918081442452859, 0.9020085738987339008, -11.91225656197089222 ) ) ;
#26364 = DIRECTION ( 'NONE',  ( 1.000000000000000000, 0.000000000000000000, -0.000000000000000000 ) ) ;
#26365 = CARTESIAN_POINT ( 'NONE',  ( 116.9373081442452929, -8.166667518702817929, -8.995218007635861213 ) ) ;
#26366 = CYLINDRICAL_SURFACE ( 'NONE', #29396, 5.000000000000004441 ) ;
#26367 = ORIENTED_EDGE ( 'NONE', *, *, #18048, .F. ) ;
#26368 = FACE_OUTER_BOUND ( 'NONE', #12664, .T. ) ;
#26369 = CARTESIAN_POINT ( 'NONE',  ( 121.5321681442453183, -9.988377603198976828, -10.36322818467138340 ) ) ;
#26370 = CARTESIAN_POINT ( 'NONE',  ( 118.5256548109119876, -0.4660016031367893996, -10.09054647747474043 ) ) ;
#26371 = CARTESIAN_POINT ( 'NONE',  ( 126.3539348109119800, -4.153390946401325223, -8.397313243818185668 ) ) ;
#26372 = CARTESIAN_POINT ( 'NONE',  ( 111.9453614775786434, -7.894159318335828068, -9.358103419637847864 ) ) ;
#26373 = CARTESIAN_POINT ( 'NONE',  ( 115.5191414775786569, -6.222761293078241884, -8.102969835052219238 ) ) ;
#26374 = CARTESIAN_POINT ( 'NONE',  ( 123.9714148109119805, -0.4660016031367893996, -10.09054647747474043 ) ) ;
#26375 = CARTESIAN_POINT ( 'NONE',  ( 108.5378796295247810, -4.863998795839590272, -19.15521520033831493 ) ) ;
#26376 = AXIS2_PLACEMENT_3D ( 'NONE', #28087, #3462, #261 ) ;
#26377 = CARTESIAN_POINT ( 'NONE',  ( 120.3409081442453044, -8.899110576539710493, -16.42337572283490132 ) ) ;
#26378 = CARTESIAN_POINT ( 'NONE',  ( 109.9649712410415816, 0.7607806665038616689, -12.14321520033831625 ) ) ;
#26379 = CARTESIAN_POINT ( 'NONE',  ( 124.5596097606643298, -2.236191541394346061, -18.14152338500401029 ) ) ;
#26380 = ORIENTED_EDGE ( 'NONE', *, *, #1583, .F. ) ;
#26381 = CARTESIAN_POINT ( 'NONE',  ( 123.0077516859119839, -0.6942167230862511529, -9.935906262978006609 ) ) ;
#26382 = CARTESIAN_POINT ( 'NONE',  ( 122.3263414775786373, -6.344957434206665248, -7.627207830600338134 ) ) ;
#26383 = CARTESIAN_POINT ( 'NONE',  ( 69.01908044833263034, -25.32952000468398879, -5.893215200338315363 ) ) ;
#26384 = CONICAL_SURFACE ( 'NONE', #40987, 0.8509999999999994236, 0.06981317007976593769 ) ;
#26385 = CARTESIAN_POINT ( 'NONE',  ( 62.95628177081277954, -3.333487351105247409, -7.653476909290080066 ) ) ;
#26386 = DIRECTION ( 'NONE',  ( 0.000000000000000000, 0.000000000000000000, 1.000000000000000000 ) ) ;
#26387 = CARTESIAN_POINT ( 'NONE',  ( 67.88234748603528601, -0.4879875857827546959, -16.39321520033831447 ) ) ;
#26388 = CARTESIAN_POINT ( 'NONE',  ( 69.36136150295220659, -57.40168791807370496, -33.05867657994173925 ) ) ;
#26389 = CARTESIAN_POINT ( 'NONE',  ( 124.8223148109119762, -10.15424416112533912, -14.75197769757731336 ) ) ;
#26390 = EDGE_CURVE ( 'NONE', #42481, #4027, #35989, .T. ) ;
#26391 = CARTESIAN_POINT ( 'NONE',  ( 92.32016463086877422, -26.75858941326842810, -11.54476601486570964 ) ) ;
#26392 = CARTESIAN_POINT ( 'NONE',  ( 124.8223148109119762, -10.15424416112533912, -14.75197769757731336 ) ) ;
#26393 = CARTESIAN_POINT ( 'NONE',  ( 69.36136150295220659, -101.1685209014307674, -50.56525720990386219 ) ) ;
#26394 = CARTESIAN_POINT ( 'NONE',  ( 124.7655881442452852, 0.5811942927096110934, -14.16772938898807510 ) ) ;
#26395 = CARTESIAN_POINT ( 'NONE',  ( 118.7525614775786380, -1.833838273342659253, -17.42832698103878286 ) ) ;
#26396 = CARTESIAN_POINT ( 'NONE',  ( 119.7434548109119703, -6.339884145921025116, -18.90789653539788517 ) ) ;
#26397 = VERTEX_POINT ( 'NONE', #28499 ) ;
#26398 = CARTESIAN_POINT ( 'NONE',  ( 123.6877814775786533, -3.383040157471821630, -19.15922257007629170 ) ) ;
#26399 = CARTESIAN_POINT ( 'NONE',  ( 116.4834948109119779, -1.561330072975668504, -17.79121239304076951 ) ) ;
#26400 = CARTESIAN_POINT ( 'NONE',  ( 115.9693640045247776, 0.1403307496149616695, -15.46607636864997204 ) ) ;
#26401 = CARTESIAN_POINT ( 'NONE',  ( 112.8529881442453302, -7.894159318335828068, -9.358103419637847864 ) ) ;
#26402 = CARTESIAN_POINT ( 'NONE',  ( 125.6164881442453094, -9.565557343593413364, -10.61323700422348004 ) ) ;
#26403 = CARTESIAN_POINT ( 'NONE',  ( 123.4041481442452834, -10.30919188438810075, -12.61870101168855918 ) ) ;
#26404 = CARTESIAN_POINT ( 'NONE',  ( 106.5237390045248418, -9.868328341294098749, -11.32035403202665869 ) ) ;
#26405 = CARTESIAN_POINT ( 'NONE',  ( 110.6909265045248247, -2.791137627527939813, -8.388885654883777576 ) ) ;
#26406 = DIRECTION ( 'NONE',  ( -0.9908103287288497762, 0.1352586133458010265, 0.000000000000000000 ) ) ;
#26407 = CARTESIAN_POINT ( 'NONE',  ( 113.7038881442453402, -6.222761293078241884, -8.102969835052219238 ) ) ;
#26408 = AXIS2_PLACEMENT_3D ( 'NONE', #35646, #42285, #4420 ) ;
#26409 = CARTESIAN_POINT ( 'NONE',  ( 117.1074881442453233, 0.4262465694468514643, -12.03445270309931736 ) ) ;
#26410 = CARTESIAN_POINT ( 'NONE',  ( 135.7024735266973323, -1.889072916127992219, -18.60376373290417362 ) ) ;
#26411 = CARTESIAN_POINT ( 'NONE',  ( 111.6632702545248605, 0.1403307496149616695, -11.32035403202665336 ) ) ;
#26412 = ORIENTED_EDGE ( 'NONE', *, *, #21755, .F. ) ;
#26413 = CARTESIAN_POINT ( 'NONE',  ( 124.9357681442453014, -7.643976991954077427, -18.09477374809248928 ) ) ;
#26414 = CARTESIAN_POINT ( 'NONE',  ( 119.6740016859119748, -0.6942167230862511529, -9.935906262978006609 ) ) ;
#26415 = CARTESIAN_POINT ( 'NONE',  ( 121.2019704359119743, 1.345710702986147034, -13.97328579221134426 ) ) ;
#26416 = ORIENTED_EDGE ( 'NONE', *, *, #2764, .F. ) ;
#26417 = PRODUCT_DEFINITION_FORMATION_WITH_SPECIFIED_SOURCE ( 'ANY', '', #38304, .NOT_KNOWN. ) ;
#26418 = CARTESIAN_POINT ( 'NONE',  ( 112.0678367055514570, -10.09801862800623518, -14.68466812670380506 ) ) ;
#26419 = CARTESIAN_POINT ( 'NONE',  ( 105.2735827545248810, -6.936859964151250502, -8.388885654883777576 ) ) ;
#26420 = EDGE_CURVE ( 'NONE', #29422, #32138, #19146, .T. ) ;
#26421 = VERTEX_POINT ( 'NONE', #11394 ) ;
#26422 = AXIS2_PLACEMENT_3D ( 'NONE', #17688, #11748, #15162 ) ;
#26423 = CARTESIAN_POINT ( 'NONE',  ( 118.6391081442452986, -4.089484607189486809, -7.948022111789456723 ) ) ;
#26424 = CARTESIAN_POINT ( 'NONE',  ( 123.8579614775786126, -9.859900752359378018, -12.68260735090039759 ) ) ;
#26425 = CARTESIAN_POINT ( 'NONE',  ( 114.6115148109119986, -6.222761293078241884, -8.102969835052219238 ) ) ;
#26426 = CARTESIAN_POINT ( 'NONE',  ( 116.3909697606643476, -2.236191541394345172, -18.14152338500401029 ) ) ;
#26427 = CARTESIAN_POINT ( 'NONE',  ( 72.75524511225664526, -25.99489077589588604, -12.39321520033831447 ) ) ;
#26428 = EDGE_CURVE ( 'NONE', #11018, #854, #12297, .T. ) ;
#26429 = CARTESIAN_POINT ( 'NONE',  ( 113.9875214775786532, -0.4660016031367893996, -10.09054647747474043 ) ) ;
#26430 = EDGE_CURVE ( 'NONE', #40611, #14254, #41638, .T. ) ;
#26431 = CARTESIAN_POINT ( 'NONE',  ( 112.9134265045247645, -2.791137627527939813, -8.388885654883777576 ) ) ;
#26432 = CARTESIAN_POINT ( 'NONE',  ( 122.7801548109119665, -3.383040157471821630, -19.15922257007629170 ) ) ;
#26433 = VERTEX_POINT ( 'NONE', #33667 ) ;
#26434 =( BOUNDED_CURVE ( )  B_SPLINE_CURVE ( 2, ( #28910, #21836, #18426, #18861, #25490 ),
 .UNSPECIFIED., .F., .T. ) 
 B_SPLINE_CURVE_WITH_KNOTS ( ( 3, 2, 3 ),
 ( 0.000000000000000000, 0.1250000000000000000, 0.2257267493207054943 ),
 .UNSPECIFIED. ) 
 CURVE ( )  GEOMETRIC_REPRESENTATION_ITEM ( )  RATIONAL_B_SPLINE_CURVE ( ( 1.000000000000000000, 0.9238795325112869605, 1.000000000000000000, 0.9386610620247159975, 0.9761776733139879703 ) ) 
 REPRESENTATION_ITEM ( '' )  );
#26435 = CARTESIAN_POINT ( 'NONE',  ( 113.6471614775786492, -5.638512984488999180, -18.83840828888717311 ) ) ;
#26436 = CARTESIAN_POINT ( 'NONE',  ( 113.0798948109119948, -8.899110576539710493, -16.42337572283490132 ) ) ;
#26437 = ADVANCED_FACE ( 'NONE', ( #44415 ), #5188, .F. ) ;
#26438 = AXIS2_PLACEMENT_3D ( 'NONE', #24181, #13476, #38287 ) ;
#26439 = DIRECTION ( 'NONE',  ( 0.000000000000000000, -0.3818493186865927203, 0.9242245927363029745 ) ) ;
#26440 = CARTESIAN_POINT ( 'NONE',  ( 112.6828081442453282, -7.893985811506177619, -18.51759400769804742 ) ) ;
#26441 = ORIENTED_EDGE ( 'NONE', *, *, #29340, .F. ) ;
#26442 = AXIS2_PLACEMENT_3D ( 'NONE', #3961, #25632, #31780 ) ;
#26443 = CARTESIAN_POINT ( 'NONE',  ( 120.4543614775786295, -4.089484607189486809, -7.948022111789456723 ) ) ;
#26444 = DIRECTION ( 'NONE',  ( 0.8636456077245089347, -0.5040994586965589219, 0.000000000000000000 ) ) ;
#26445 = CARTESIAN_POINT ( 'NONE',  ( 119.8791860609119624, -6.339478340643393217, -8.615877017535622073 ) ) ;
#26446 = EDGE_CURVE ( 'NONE', #30023, #16801, #34916, .T. ) ;
#26447 = DIRECTION ( 'NONE',  ( 0.000000000000000000, 0.6004852223388321697, -0.7996358532186279566 ) ) ;
#26448 = ADVANCED_FACE ( 'NONE', ( #5419 ), #33221, .F. ) ;
#26449 = EDGE_CURVE ( 'NONE', #25838, #40192, #21929, .T. ) ;
#26450 = CARTESIAN_POINT ( 'NONE',  ( 123.5300843491906733, -4.187684698237162273, -15.54286723766359479 ) ) ;
#26451 = CARTESIAN_POINT ( 'NONE',  ( 115.8027748109119841, -8.899110576539710493, -16.42337572283490132 ) ) ;
#26452 = CARTESIAN_POINT ( 'NONE',  ( 60.34146317132753978, -13.36775875599912844, -7.393215200338315363 ) ) ;
#26453 = VECTOR ( 'NONE', #43709, 1000.000000000000114 ) ;
#26454 = DIRECTION ( 'NONE',  ( 0.9609149988134843001, -0.1028163501681632064, 0.2570431154366505933 ) ) ;
#26455 = CARTESIAN_POINT ( 'NONE',  ( 112.9097148109120070, -9.565557343593413364, -10.61323700422348004 ) ) ;
#26456 = CARTESIAN_POINT ( 'NONE',  ( 113.7038881442453402, -3.383040157471821630, -19.15922257007629170 ) ) ;
#26457 = CARTESIAN_POINT ( 'NONE',  ( 121.1325173109119788, -9.289237151508434209, -11.05642687123711276 ) ) ;
#26458 = CARTESIAN_POINT ( 'NONE',  ( 113.1366214775786432, -1.834011780172310813, -8.268836392978581529 ) ) ;
#26459 = CARTESIAN_POINT ( 'NONE',  ( 114.6115148109119986, -6.222761293078241884, -8.102969835052219238 ) ) ;
#26460 = CARTESIAN_POINT ( 'NONE',  ( 122.2128881442453263, -1.834011780172310813, -8.268836392978581529 ) ) ;
#26461 = CARTESIAN_POINT ( 'NONE',  ( 123.5743281442453139, -7.893985811506177619, -18.51759400769804742 ) ) ;
#26462 = VERTEX_POINT ( 'NONE', #26627 ) ;
#26463 = CARTESIAN_POINT ( 'NONE',  ( 112.1155414775786454, 0.9020085738987339008, -11.91225656197089222 ) ) ;
#26464 = CARTESIAN_POINT ( 'NONE',  ( 110.9687390045248350, 0.8980012041604421569, -15.77991374673208469 ) ) ;
#26465 = CARTESIAN_POINT ( 'NONE',  ( 108.1211608795247798, -1.325403438956436419, -16.93181055722141792 ) ) ;
#26466 = CARTESIAN_POINT ( 'NONE',  ( 107.5655358795247736, -8.402594152722688392, -9.854619843455216355 ) ) ;
#26467 = DIRECTION ( 'NONE',  ( 0.000000000000000000, 0.9242245927363028635, 0.3818493186865930533 ) ) ;
#26468 = CARTESIAN_POINT ( 'NONE',  ( 119.0929214775786278, -5.638512984488999180, -18.83840828888717311 ) ) ;
#26469 = ORIENTED_EDGE ( 'NONE', *, *, #27126, .T. ) ;
#26470 = CARTESIAN_POINT ( 'NONE',  ( 125.0492214775786266, -6.344957434206665248, -7.627207830600338134 ) ) ;
#26471 = CARTESIAN_POINT ( 'NONE',  ( 66.82415148905926117, -40.21211973637273474, -23.89321520033831803 ) ) ;
#26472 = CARTESIAN_POINT ( 'NONE',  ( 117.2294421295247844, -10.76310523276723785, -21.89255013987451548 ) ) ;
#26473 = B_SPLINE_CURVE_WITH_KNOTS ( 'NONE', 3,
 ( #9606, #20546, #16678, #30130, #40619, #13485, #44043, #37409, #23750, #27387, #33756, #13257, #6634, #33517, #41311, #41083, #10071, #9839, #20099, #37640, #2524, #6414, #23972, #20322, #16451, #37858, #34425, #12807, #2297, #16226, #19867 ),
 .UNSPECIFIED., .F., .F.,
 ( 4, 2, 2, 1, 1, 1, 2, 2, 2, 1, 1, 1, 2, 2, 2, 1, 2, 2, 4 ),
 ( 0.000000000000000000, 0.2500000000000044964, 0.3750000000000062172, 0.4375000000000071054, 0.4687500000000212053, 0.4843750000000144329, 0.4921875000000255351, 0.5000000000000366374, 0.6250000000000016653, 0.6874999999999731326, 0.7187499999999706901, 0.7343749999999695799, 0.7421874999999682476, 0.7499999999999669154, 0.8124999999999887867, 0.8437499999999990008, 0.8593749999999964473, 0.8749999999999940048, 1.000000000000000000 ),
 .UNSPECIFIED. ) ;
#26474 = CARTESIAN_POINT ( 'NONE',  ( 115.2922348109119781, 0.4262465694468514643, -12.03445270309931736 ) ) ;
#26475 = CARTESIAN_POINT ( 'NONE',  ( 106.0375671295248310, 0.1403307496149613920, -13.39321520033831447 ) ) ;
#26476 = CARTESIAN_POINT ( 'NONE',  ( 121.4754414775786131, -8.166667518702819706, -8.995218007635861213 ) ) ;
#26477 = CARTESIAN_POINT ( 'NONE',  ( 108.5378796295247810, -4.863998795839590272, -19.15521520033831493 ) ) ;
#26478 = PLANE ( 'NONE',  #18435 ) ;
#26479 = VERTEX_POINT ( 'NONE', #26176 ) ;
#26480 = CARTESIAN_POINT ( 'NONE',  ( 89.12784890491134604, -24.14644159042263993, -12.62951656296512937 ) ) ;
#26481 = CARTESIAN_POINT ( 'NONE',  ( 122.2128881442453263, -7.643976991954077427, -18.09477374809248928 ) ) ;
#26482 = TOROIDAL_SURFACE ( 'NONE', #952, 3.640000000000000124, 0.3600000000000000422 ) ;
#26483 = CARTESIAN_POINT ( 'NONE',  ( 119.0929214775786278, -5.638512984488999180, -18.83840828888717311 ) ) ;
#26484 = FACE_OUTER_BOUND ( 'NONE', #24312, .T. ) ;
#26485 = CARTESIAN_POINT ( 'NONE',  ( 115.6325948109119821, 0.2603800115204892296, -16.42320221600525088 ) ) ;
#26486 = DIRECTION ( 'NONE',  ( 0.000000000000000000, 0.000000000000000000, -1.000000000000000000 ) ) ;
#26487 = CARTESIAN_POINT ( 'NONE',  ( 124.5386814775786206, -4.153390946401325223, -8.397313243818185668 ) ) ;
#26488 = CARTESIAN_POINT ( 'NONE',  ( 119.8303681442453126, 0.4262465694468514643, -12.03445270309931736 ) ) ;
#26489 = ORIENTED_EDGE ( 'NONE', *, *, #4499, .F. ) ;
#26490 = CARTESIAN_POINT ( 'NONE',  ( 122.5910329359119970, -4.283928203966213211, -7.183505701512925334 ) ) ;
#26491 = CIRCLE ( 'NONE', #6830, 2.999999999999999556 ) ;
#26492 = CARTESIAN_POINT ( 'NONE',  ( 114.3278814775786429, -10.30919188438810075, -12.61870101168855918 ) ) ;
#26493 = CARTESIAN_POINT ( 'NONE',  ( 120.5678148109119832, -1.833838273342659253, -17.42832698103878286 ) ) ;
#26494 = ORIENTED_EDGE ( 'NONE', *, *, #28781, .T. ) ;
#26495 = CARTESIAN_POINT ( 'NONE',  ( 121.8270485609119760, -0.08252387247370887580, -11.91645802438286417 ) ) ;
#26496 = CARTESIAN_POINT ( 'NONE',  ( 117.3343948109119737, -3.383040157471821630, -19.15922257007629170 ) ) ;
#26497 = CARTESIAN_POINT ( 'NONE',  ( 114.5803015045248117, -2.477300249445798297, -7.631215200338321125 ) ) ;
#26498 = CARTESIAN_POINT ( 'NONE',  ( 116.4834948109119779, -7.894159318335828068, -9.358103419637847864 ) ) ;
#26499 = ORIENTED_EDGE ( 'NONE', *, *, #29512, .T. ) ;
#26500 = EDGE_LOOP ( 'NONE', ( #40746, #37722, #9922, #27093 ) ) ;
#26501 = CARTESIAN_POINT ( 'NONE',  ( 126.0135748109119902, -1.833838273342660141, -17.42832698103878286 ) ) ;
#26502 = CARTESIAN_POINT ( 'NONE',  ( 120.3976348109119812, -7.643976991954077427, -18.09477374809248928 ) ) ;
#26503 = EDGE_CURVE ( 'NONE', #43140, #11788, #5906, .T. ) ;
#26504 = DIRECTION ( 'NONE',  ( -0.000000000000000000, -0.9284778069183718952, -0.3713878862591649677 ) ) ;
#26505 = CARTESIAN_POINT ( 'NONE',  ( 118.9794681442453026, -9.261995988541697145, -16.69588392320189030 ) ) ;
#26506 = LINE ( 'NONE', #40185, #34947 ) ;
#26507 = ADVANCED_FACE ( 'NONE', ( #22744 ), #43347, .T. ) ;
#26508 = CARTESIAN_POINT ( 'NONE',  ( 114.6682414775786469, -1.561330072975668060, -17.79121239304076596 ) ) ;
#26510 = CARTESIAN_POINT ( 'NONE',  ( 114.9518748109119883, -7.643976991954077427, -18.09477374809248928 ) ) ;
#26509 = CARTESIAN_POINT ( 'NONE',  ( 115.2355081442453155, -10.30919188438810075, -12.61870101168855918 ) ) ;
#26511 = EDGE_CURVE ( 'NONE', #14190, #11722, #7244, .T. ) ;
#26512 = CARTESIAN_POINT ( 'NONE',  ( 125.3895814775786448, -2.084020599724406786, -8.691656652584148546 ) ) ;
#26513 = CARTESIAN_POINT ( 'NONE',  ( 113.8740681442453138, 0.5811942927096154232, -14.16772938898807155 ) ) ;
#26514 = VERTEX_POINT ( 'NONE', #21860 ) ;
#26515 = CARTESIAN_POINT ( 'NONE',  ( 123.2906948109119867, -1.833838273342659697, -17.42832698103878286 ) ) ;
#26516 = CYLINDRICAL_SURFACE ( 'NONE', #32904, 1.199999999999999512 ) ;
#26517 = FACE_OUTER_BOUND ( 'NONE', #768, .T. ) ;
#26518 = CARTESIAN_POINT ( 'NONE',  ( 114.7192077545248594, -7.250697342233347165, -7.631215200338321125 ) ) ;
#26519 = CARTESIAN_POINT ( 'NONE',  ( 112.3578015045248861, -6.936859964151250502, -18.39754474579286025 ) ) ;
#26520 = CARTESIAN_POINT ( 'NONE',  ( 110.5520202545248054, -10.62599879583958717, -15.77991374673208469 ) ) ;
#26521 = CARTESIAN_POINT ( 'NONE',  ( 119.6601881442453106, -8.166667518702819706, -8.995218007635861213 ) ) ;
#26522 = VERTEX_POINT ( 'NONE', #28712 ) ;
#26523 = CARTESIAN_POINT ( 'NONE',  ( 120.7379948109119709, -10.63000616557722466, -14.87417383870573495 ) ) ;
#26524 = CARTESIAN_POINT ( 'NONE',  ( 61.76986277844709861, -39.32091226840162079, -7.393215200338315363 ) ) ;
#26525 = CARTESIAN_POINT ( 'NONE',  ( 106.6626452545248611, 0.8980012041604421569, -11.00651665394454071 ) ) ;
#26526 = CARTESIAN_POINT ( 'NONE',  ( 120.1707281442453166, 0.2603800115204892296, -16.42320221600525088 ) ) ;
#26527 = CARTESIAN_POINT ( 'NONE',  ( 121.8158014775786171, -5.638512984488999180, -18.83840828888717311 ) ) ;
#26528 = CARTESIAN_POINT ( 'NONE',  ( 68.14371629974728251, -1.351251493923715685, -16.39321520033831447 ) ) ;
#26529 = FACE_OUTER_BOUND ( 'NONE', #3065, .T. ) ;
#26530 = EDGE_LOOP ( 'NONE', ( #4093, #2834, #8657, #12015, #28563 ) ) ;
#26531 = CARTESIAN_POINT ( 'NONE',  ( 67.84197459855160162, -58.29708508664516842, -37.25081299080650865 ) ) ;
#26532 = DIRECTION ( 'NONE',  ( 1.000000000000000000, 0.000000000000000000, -0.000000000000000000 ) ) ;
#26533 = CARTESIAN_POINT ( 'NONE',  ( 122.4397948109119767, -0.1624402480850797581, -16.17319339645315424 ) ) ;
#26534 = CARTESIAN_POINT ( 'NONE',  ( 111.8716296295247901, -4.863998795839590272, -8.388885654883775800 ) ) ;
#26535 = CARTESIAN_POINT ( 'NONE',  ( 109.0935046295247872, -4.863998795839590272, -18.39754474579285315 ) ) ;
#26536 = CARTESIAN_POINT ( 'NONE',  ( 117.7882081442453170, -3.505236298600246325, -18.68346056562440793 ) ) ;
#26537 = CARTESIAN_POINT ( 'NONE',  ( 67.69189222814998175, -55.76310523276723785, -40.89321520033831092 ) ) ;
#26538 = CARTESIAN_POINT ( 'NONE',  ( 68.93854012757255134, -25.83497651491618896, -5.893215200338315363 ) ) ;
#26539 = CARTESIAN_POINT ( 'NONE',  ( 112.2857214775786474, -5.574606645277164318, -18.38911715685844683 ) ) ;
#26540 = CARTESIAN_POINT ( 'NONE',  ( 125.1626748109119802, -9.988377603198980381, -10.36322818467138518 ) ) ;
#26541 = ORIENTED_EDGE ( 'NONE', *, *, #39558, .T. ) ;
#26542 = CARTESIAN_POINT ( 'NONE',  ( 123.0070614775786169, -10.15424416112533912, -14.75197769757731336 ) ) ;
#26543 = CARTESIAN_POINT ( 'NONE',  ( 113.4202548109119846, -10.30919188438810075, -12.61870101168855918 ) ) ;
#26544 = CARTESIAN_POINT ( 'NONE',  ( 121.5888948109119809, -10.30919188438810075, -12.61870101168855918 ) ) ;
#26545 = CARTESIAN_POINT ( 'NONE',  ( 121.9292548109119849, -7.894159318335828068, -9.358103419637847864 ) ) ;
#26546 = ORIENTED_EDGE ( 'NONE', *, *, #30620, .T. ) ;
#26547 = CARTESIAN_POINT ( 'NONE',  ( 120.3439060953690642, -6.001247023715329476, -18.26661038929047720 ) ) ;
#26548 = ADVANCED_FACE ( 'NONE', ( #32778 ), #37194, .T. ) ;
#26549 = CARTESIAN_POINT ( 'NONE',  ( 124.5954081442453116, -3.383040157471821630, -19.15922257007629170 ) ) ;
#26550 = CARTESIAN_POINT ( 'NONE',  ( 115.1220548109119761, -1.833838273342658809, -17.42832698103878286 ) ) ;
#26551 = CARTESIAN_POINT ( 'NONE',  ( 123.8012348109119642, 0.2603800115204892296, -16.42320221600525088 ) ) ;
#26552 = CARTESIAN_POINT ( 'NONE',  ( 106.3153796295248412, -4.863998795839590272, -19.15521520033831493 ) ) ;
#26553 = FACE_OUTER_BOUND ( 'NONE', #11274, .T. ) ;
#26554 = VERTEX_POINT ( 'NONE', #34088 ) ;
#26555 = CARTESIAN_POINT ( 'NONE',  ( 128.1199079201516327, -2.703369936665986462, -15.02142562904077039 ) ) ;
#26556 = CARTESIAN_POINT ( 'NONE',  ( 110.4825671295247815, 0.1403307496149613920, -13.39321520033831447 ) ) ;
#26557 = EDGE_CURVE ( 'NONE', #8479, #20261, #1539, .T. ) ;
#26558 = LINE ( 'NONE', #43438, #7390 ) ;
#26559 = CARTESIAN_POINT ( 'NONE',  ( 118.6958348109119754, -3.505236298600246325, -18.68346056562440793 ) ) ;
#26560 = CARTESIAN_POINT ( 'NONE',  ( 113.6471614775786492, -4.153390946401321671, -8.397313243818183892 ) ) ;
#26561 = CARTESIAN_POINT ( 'NONE',  ( 126.4038788492663770, -6.085149154362555990, -18.33735632256993142 ) ) ;
#26562 = ORIENTED_EDGE ( 'NONE', *, *, #43752, .F. ) ;
#26563 = CARTESIAN_POINT ( 'NONE',  ( 109.2294421295247844, -11.83367149576868727, -19.39321520033831447 ) ) ;
#26564 = CARTESIAN_POINT ( 'NONE',  ( 118.0718414775786442, -0.8288870151387760510, -10.36305467784173118 ) ) ;
#26565 = CIRCLE ( 'NONE', #39678, 2.000000000000000444 ) ;
#26566 = CARTESIAN_POINT ( 'NONE',  ( 112.8529881442453302, -7.894159318335828068, -9.358103419637847864 ) ) ;
#26567 = CARTESIAN_POINT ( 'NONE',  ( 67.74656486299329572, -0.3633886386785405986, -10.39321520033831625 ) ) ;
#26568 = DIRECTION ( 'NONE',  ( 0.7071067811865520136, 8.659560562354881089E-17, 0.7071067811865431318 ) ) ;
#26570 = CARTESIAN_POINT ( 'NONE',  ( 123.8012348109119642, 0.2603800115204892296, -16.42320221600525088 ) ) ;
#26569 = CARTESIAN_POINT ( 'NONE',  ( 113.9077908578216807, 0.04929351793716424401, -12.14321520033834467 ) ) ;
#26571 = CARTESIAN_POINT ( 'NONE',  ( 123.8012348109119642, -9.565557343593413364, -10.61323700422348004 ) ) ;
#26572 = ORIENTED_EDGE ( 'NONE', *, *, #3062, .T. ) ;
#26573 = FACE_OUTER_BOUND ( 'NONE', #30758, .T. ) ;
#26574 = DIRECTION ( 'NONE',  ( -0.9908103287288505534, 0.1352586133457945317, 0.000000000000000000 ) ) ;
#26575 = CARTESIAN_POINT ( 'NONE',  ( 111.1770983795247787, -8.402594152722688392, -16.93181055722141792 ) ) ;
#26576 = CARTESIAN_POINT ( 'NONE',  ( 126.5808414775786446, -9.859900752359378018, -12.68260735090039759 ) ) ;
#26577 = CARTESIAN_POINT ( 'NONE',  ( 118.2987481442453088, -7.894159318335828068, -9.358103419637847864 ) ) ;
#26578 = CARTESIAN_POINT ( 'NONE',  ( 125.2512653913891114, 1.177777608218840255, -17.42223183254473184 ) ) ;
#26579 = CARTESIAN_POINT ( 'NONE',  ( 113.3301452545248083, -9.868328341294098749, -15.46607636864997204 ) ) ;
#26580 = CARTESIAN_POINT ( 'NONE',  ( 116.9373081442452929, -8.166667518702805495, -8.995218007635850554 ) ) ;
#26581 = FACE_OUTER_BOUND ( 'NONE', #34417, .T. ) ;
#26582 = CARTESIAN_POINT ( 'NONE',  ( 113.2858169107182107, -2.467220198592768199, -17.83387418641523325 ) ) ;
#26583 = ADVANCED_FACE ( 'NONE', ( #30682 ), #10167, .T. ) ;
#26584 = CARTESIAN_POINT ( 'NONE',  ( 112.2883483795247770, -0.7896495226426338832, -9.318865927141430916 ) ) ;
#26585 = CARTESIAN_POINT ( 'NONE',  ( -13.56828339430762398, -4.779084841531242134, -17.94044720194083808 ) ) ;
#26586 = CARTESIAN_POINT ( 'NONE',  ( 113.3995983795247895, -0.7896495226426338832, -9.318865927141430916 ) ) ;
#26587 = CARTESIAN_POINT ( 'NONE',  ( 119.8303681442453126, -10.63000616557722466, -14.87417383870573495 ) ) ;
#26588 = CARTESIAN_POINT ( 'NONE',  ( 120.6812681442452941, -10.30919188438810075, -12.61870101168855918 ) ) ;
#26589 = LINE ( 'NONE', #5382, #34974 ) ;
#26590 = CARTESIAN_POINT ( 'NONE',  ( 115.6325948109119821, 0.2603800115204892296, -16.42320221600525088 ) ) ;
#26591 = CARTESIAN_POINT ( 'NONE',  ( 111.7751814775786556, -7.893985811506177619, -18.51759400769804742 ) ) ;
#26592 = ORIENTED_EDGE ( 'NONE', *, *, #20333, .T. ) ;
#26593 = CARTESIAN_POINT ( 'NONE',  ( 114.4980614775786734, -2.084020599724406786, -8.691656652584148546 ) ) ;
#26594 = AXIS2_PLACEMENT_3D ( 'NONE', #39900, #4784, #18704 ) ;
#26595 = CARTESIAN_POINT ( 'NONE',  ( 112.9664414775786412, -9.859900752359374465, -12.68260735090039404 ) ) ;
#26596 = CARTESIAN_POINT ( 'NONE',  ( 118.6958348109119754, -6.344957434206665248, -7.627207830600338134 ) ) ;
#26597 = CARTESIAN_POINT ( 'NONE',  ( 124.1983214775786166, -1.833838273342659697, -17.42832698103878286 ) ) ;
#26598 = CARTESIAN_POINT ( 'NONE',  ( 112.0588148109119828, -9.859900752359374465, -12.68260735090039404 ) ) ;
#26599 = EDGE_LOOP ( 'NONE', ( #27903, #22142, #6751, #5105, #39509 ) ) ;
#26600 = CARTESIAN_POINT ( 'NONE',  ( 119.1496481442453046, -6.222761293078241884, -8.102969835052219238 ) ) ;
#26601 = CARTESIAN_POINT ( 'NONE',  ( 126.0703014775786102, -9.988377603198980381, -10.36322818467138518 ) ) ;
#26602 = CARTESIAN_POINT ( 'NONE',  ( 108.1211608795247798, -8.938348069036489818, -9.318865927141430916 ) ) ;
#26603 = CARTESIAN_POINT ( 'NONE',  ( 119.8303681442453126, 0.4262465694468514643, -12.03445270309931736 ) ) ;
#26604 = DIRECTION ( 'NONE',  ( 0.9609149988134837450, -0.1028163501681639419, 0.2570431154366518145 ) ) ;
#26605 = DIRECTION ( 'NONE',  ( 0.000000000000000000, -0.3818493186865927203, 0.9242245927363029745 ) ) ;
#26606 = ORIENTED_EDGE ( 'NONE', *, *, #37137, .T. ) ;
#26607 = CARTESIAN_POINT ( 'NONE',  ( 121.7575954359119805, 0.5291689781388270175, -13.89700978578772705 ) ) ;
#26608 = CARTESIAN_POINT ( 'NONE',  ( 124.4819548109119722, -7.893985811506177619, -18.51759400769804742 ) ) ;
#26609 = CARTESIAN_POINT ( 'NONE',  ( 112.9828796295247884, -4.863998795839638234, -8.388885654883775800 ) ) ;
#26610 = CARTESIAN_POINT ( 'NONE',  ( 112.1722681442453222, -0.4660016031367893996, -10.09054647747474043 ) ) ;
#26611 = EDGE_CURVE ( 'NONE', #6975, #16083, #39406, .T. ) ;
#26612 = CARTESIAN_POINT ( 'NONE',  ( 116.9333032873346383, 1.865211299501440712, -5.695039816857145887 ) ) ;
#26613 = DIRECTION ( 'NONE',  ( 0.000000000000000000, -0.9242245927363028635, -0.3818493186865930533 ) ) ;
#26614 = CARTESIAN_POINT ( 'NONE',  ( 106.8015515045248378, -6.936859964151250502, -18.39754474579286025 ) ) ;
#26615 = B_SPLINE_CURVE_WITH_KNOTS ( 'NONE', 3,
 ( #15367, #38612, #42956, #7617, #21306, #21530, #22203, #4870, #42288, #21757 ),
 .UNSPECIFIED., .F., .F.,
 ( 4, 3, 3, 4 ),
 ( 3.127317220692749988E-18, 0.0002476486808869839996, 0.0004952973797228660095, 0.0009539399846111540045 ),
 .UNSPECIFIED. ) ;
#26616 = CARTESIAN_POINT ( 'NONE',  ( 67.37136766119182596, -67.53150897494617766, -41.09057840265009531 ) ) ;
#26617 = CARTESIAN_POINT ( 'NONE',  ( 135.6920194349522717, -4.118011552333871172, -19.32288967780376865 ) ) ;
#26618 = CONICAL_SURFACE ( 'NONE', #29547, 3.499999999999999556, 1.325817663668031887 ) ;
#26619 = CARTESIAN_POINT ( 'NONE',  ( 125.2473467947029206, -11.99112074166402842, -14.81453580268809134 ) ) ;
#26620 = CARTESIAN_POINT ( 'NONE',  ( 111.9261565460472099, -2.191907684172563986, -18.20049396185734025 ) ) ;
#26621 = CARTESIAN_POINT ( 'NONE',  ( 116.7104014775786425, -8.899110576539710493, -16.42337572283490132 ) ) ;
#26622 = CARTESIAN_POINT ( 'NONE',  ( 125.6732148109119862, -9.859900752359378018, -12.68260735090039759 ) ) ;
#26623 = ORIENTED_EDGE ( 'NONE', *, *, #3581, .F. ) ;
#26624 = CARTESIAN_POINT ( 'NONE',  ( 122.8936081442453059, 0.2603800115204892296, -16.42320221600525088 ) ) ;
#26625 = CARTESIAN_POINT ( 'NONE',  ( 116.1431348109119881, -10.30919188438810075, -12.61870101168855918 ) ) ;
#26626 = CARTESIAN_POINT ( 'NONE',  ( 116.6638952545248031, -9.868328341294098749, -15.46607636864997204 ) ) ;
#26627 = CARTESIAN_POINT ( 'NONE',  ( 65.19189222814998175, -41.76310523276723785, -6.393215200338315363 ) ) ;
#26628 = CIRCLE ( 'NONE', #6977, 1.199999999999999734 ) ;
#26629 = CARTESIAN_POINT ( 'NONE',  ( 124.5386814775786206, -4.153390946401325223, -8.397313243818185668 ) ) ;
#26630 = CARTESIAN_POINT ( 'NONE',  ( 123.5176014775786228, -9.261995988541697145, -16.69588392320189030 ) ) ;
#26631 = CARTESIAN_POINT ( 'NONE',  ( 106.3848327545248651, -6.936859964151250502, -8.388885654883777576 ) ) ;
#26632 = CARTESIAN_POINT ( 'NONE',  ( 109.7880358795247986, -8.402594152722688392, -9.854619843455216355 ) ) ;
#26633 = CARTESIAN_POINT ( 'NONE',  ( 82.80200173989635459, -31.79535628182557971, -23.14532950183733462 ) ) ;
#26634 = CARTESIAN_POINT ( 'NONE',  ( 116.1431348109119881, 0.1319031606808879209, -14.10382304977623669 ) ) ;
#26635 = CARTESIAN_POINT ( 'NONE',  ( 115.6893214775786447, -9.859900752359374465, -12.68260735090039404 ) ) ;
#26636 = LINE ( 'NONE', #40549, #21164 ) ;
#26637 = CARTESIAN_POINT ( 'NONE',  ( 114.3719421295247827, -9.868328341294093420, -13.39321520033831447 ) ) ;
#26638 = ORIENTED_EDGE ( 'NONE', *, *, #42590, .T. ) ;
#26639 = CARTESIAN_POINT ( 'NONE',  ( 109.2296068920433783, -0.1296147630240877813, -15.30322596940846758 ) ) ;
#26640 = CARTESIAN_POINT ( 'NONE',  ( 124.8790414775786246, -8.899110576539710493, -16.42337572283490132 ) ) ;
#26641 = CARTESIAN_POINT ( 'NONE',  ( 123.9106423109119675, -9.959231468620755479, -10.70263013195267199 ) ) ;
#26642 = CARTESIAN_POINT ( 'NONE',  ( 122.7993923109119692, -9.959231468620755479, -10.70263013195267199 ) ) ;
#26643 = ORIENTED_EDGE ( 'NONE', *, *, #40899, .F. ) ;
#26644 = CARTESIAN_POINT ( 'NONE',  ( 123.9680514173871018, -8.493878760966627084, -17.54745775818410536 ) ) ;
#26645 = CARTESIAN_POINT ( 'NONE',  ( 117.0091510799717014, -11.49078741053932085, -21.62708738602523084 ) ) ;
#26646 = ORIENTED_EDGE ( 'NONE', *, *, #11421, .F. ) ;
#26647 = CARTESIAN_POINT ( 'NONE',  ( 117.8449348109119938, -8.166667518702817929, -8.995218007635861213 ) ) ;
#26648 = CARTESIAN_POINT ( 'NONE',  ( 124.9357681442453014, -7.643976991954077427, -18.09477374809248928 ) ) ;
#26649 = CARTESIAN_POINT ( 'NONE',  ( 115.2355081442453155, 0.1319031606808879209, -14.10382304977623669 ) ) ;
#26650 = CARTESIAN_POINT ( 'NONE',  ( 116.4642898793805443, -2.191907684172563986, -18.20049396185734025 ) ) ;
#26651 = CARTESIAN_POINT ( 'NONE',  ( 124.0848681442452772, -4.089484607189435295, -7.948022111789469157 ) ) ;
#26652 = CARTESIAN_POINT ( 'NONE',  ( 114.0442481442453300, -1.834011780172310813, -8.268836392978581529 ) ) ;
#26653 = AXIS2_PLACEMENT_3D ( 'NONE', #3889, #24650, #25103 ) ;
#26654 = CARTESIAN_POINT ( 'NONE',  ( 110.7603796295247918, -4.863998795839590272, -8.388885654883775800 ) ) ;
#26655 = CARTESIAN_POINT ( 'NONE',  ( 125.2194014775786286, -10.30919188438810075, -12.61870101168855918 ) ) ;
#26656 = DIRECTION ( 'NONE',  ( -1.000000000000000000, 0.000000000000000000, 0.000000000000000000 ) ) ;
#26657 = ORIENTED_EDGE ( 'NONE', *, *, #17831, .F. ) ;
#26658 = CARTESIAN_POINT ( 'NONE',  ( 112.8529881442453302, -1.561330072975668060, -17.79121239304076596 ) ) ;
#26659 = CARTESIAN_POINT ( 'NONE',  ( 115.6325948109119821, -9.565557343593413364, -10.61323700422348004 ) ) ;
#26660 = AXIS2_PLACEMENT_3D ( 'NONE', #8273, #1858, #31906 ) ;
#26661 = CARTESIAN_POINT ( 'NONE',  ( 126.3115243456300050, -5.212275628432266217, -18.42773177175248733 ) ) ;
#26662 = CARTESIAN_POINT ( 'NONE',  ( 125.6732148109119862, -9.859900752359378018, -12.68260735090039759 ) ) ;
#26663 = EDGE_LOOP ( 'NONE', ( #9612, #15578, #33909, #37534, #6421, #43086, #28033, #13646, #37100, #41153, #7590, #43065, #14601, #10107, #9011, #4139, #18744, #36831, #36642, #38439, #28892, #12436, #17983 ) ) ;
#26664 = CARTESIAN_POINT ( 'NONE',  ( 123.2339681442453241, -6.344957434206665248, -7.627207830600338134 ) ) ;
#26665 = AXIS2_PLACEMENT_3D ( 'NONE', #15488, #5215, #15259 ) ;
#26666 = CARTESIAN_POINT ( 'NONE',  ( 74.47157298427187300, -3.053873105668316601, -7.147228641687434880 ) ) ;
#26667 = CARTESIAN_POINT ( 'NONE',  ( 110.2742077545248236, -2.791137627527887410, -18.39754474579284249 ) ) ;
#26668 = CARTESIAN_POINT ( 'NONE',  ( 79.05243529145373316, 4.793396140045460108, -14.64321520033831447 ) ) ;
#26669 = CARTESIAN_POINT ( 'NONE',  ( 117.6747548109119919, -7.643976991954077427, -18.09477374809248928 ) ) ;
#26670 = CARTESIAN_POINT ( 'NONE',  ( 112.5745671540078661, -2.348512537728058902, -17.99195118506215962 ) ) ;
#26671 = CARTESIAN_POINT ( 'NONE',  ( 113.0231681442453180, -10.15424416112533912, -14.75197769757731336 ) ) ;
#26672 = EDGE_CURVE ( 'NONE', #27457, #12848, #38184, .T. ) ;
#26673 = DIRECTION ( 'NONE',  ( 0.7871354856660167654, -0.6167752151498625546, -0.002461946824136807422 ) ) ;
#26674 = CARTESIAN_POINT ( 'NONE',  ( 124.1207852356725709, -3.874282071529665750, -21.33170422639506469 ) ) ;
#26675 = TOROIDAL_SURFACE ( 'NONE', #27406, 4.700000000000000178, 0.2999999999999999889 ) ;
#26676 = CARTESIAN_POINT ( 'NONE',  ( 116.5969481442453031, -9.859900752359374465, -12.68260735090039404 ) ) ;
#26677 = CARTESIAN_POINT ( 'NONE',  ( 116.7671281442453335, -1.834011780172310813, -8.268836392978581529 ) ) ;
#26678 = CARTESIAN_POINT ( 'NONE',  ( 123.0077516859119839, -0.6942167230862511529, -9.935906262978006609 ) ) ;
#26679 = CARTESIAN_POINT ( 'NONE',  ( 113.9875214775786532, -0.4660016031367893996, -10.09054647747474043 ) ) ;
#26680 = CARTESIAN_POINT ( 'NONE',  ( 114.4413348109119823, -0.8288870151387760510, -10.36305467784173118 ) ) ;
#26681 = CARTESIAN_POINT ( 'NONE',  ( 123.2906948109119867, -8.166667518702819706, -8.995218007635861213 ) ) ;
#26682 = CARTESIAN_POINT ( 'NONE',  ( 123.6310548109119765, -5.638512984488999180, -18.83840828888717311 ) ) ;
#26683 = ORIENTED_EDGE ( 'NONE', *, *, #25847, .T. ) ;
#26684 = CARTESIAN_POINT ( 'NONE',  ( 114.2711548109119803, -9.988377603198976828, -10.36322818467138340 ) ) ;
#26685 = EDGE_CURVE ( 'NONE', #38550, #6765, #41850, .T. ) ;
#26686 = CARTESIAN_POINT ( 'NONE',  ( 110.2742077545248094, -7.250697342233347165, -7.631215200338321125 ) ) ;
#26687 = AXIS2_PLACEMENT_3D ( 'NONE', #13892, #10254, #24161 ) ;
#26688 = CARTESIAN_POINT ( 'NONE',  ( 105.4124890045248293, -9.868328341294098749, -11.32035403202665869 ) ) ;
#26689 = CARTESIAN_POINT ( 'NONE',  ( 107.0793640045248196, 0.1403307496149616695, -15.46607636864997204 ) ) ;
#26690 = CARTESIAN_POINT ( 'NONE',  ( 120.2841814775786276, 0.9020085738987339008, -11.91225656197089222 ) ) ;
#26691 = ORIENTED_EDGE ( 'NONE', *, *, #31803, .F. ) ;
#26692 = CARTESIAN_POINT ( 'NONE',  ( 124.6521348109119884, -1.561330072975668948, -17.79121239304076951 ) ) ;
#26693 = CARTESIAN_POINT ( 'NONE',  ( 87.68939540009954214, -27.84333996136784961, -14.15691383771150136 ) ) ;
#26694 = CARTESIAN_POINT ( 'NONE',  ( 116.1998614775786507, 0.4262465694468514643, -12.03445270309931736 ) ) ;
#26695 = CARTESIAN_POINT ( 'NONE',  ( 105.1346765045248475, -2.791137627527939813, -8.388885654883777576 ) ) ;
#26696 = VECTOR ( 'NONE', #33477, 1000.000000000000227 ) ;
#26697 = CARTESIAN_POINT ( 'NONE',  ( 118.1285681442453068, -7.893985811506177619, -18.51759400769804742 ) ) ;
#26698 = CARTESIAN_POINT ( 'NONE',  ( 114.9970202545248412, 0.1403307496149616695, -11.32035403202665336 ) ) ;
#26699 = DIRECTION ( 'NONE',  ( 0.9908103287288505534, -0.1352586133457944206, 0.000000000000000000 ) ) ;
#26700 = ORIENTED_EDGE ( 'NONE', *, *, #11402, .F. ) ;
#26701 = CARTESIAN_POINT ( 'NONE',  ( 110.7102801496069873, 0.3591747506842615789, -14.64321520033831447 ) ) ;
#26702 = CARTESIAN_POINT ( 'NONE',  ( 123.4608748109119745, 0.4262465694468514643, -12.03445270309931736 ) ) ;
#26703 = CARTESIAN_POINT ( 'NONE',  ( 121.2485348109119769, -0.4660016031367893996, -10.09054647747474043 ) ) ;
#26704 = CARTESIAN_POINT ( 'NONE',  ( 70.19189222814998175, -100.0979043305785581, -53.24182196210380624 ) ) ;
#26705 = CARTESIAN_POINT ( 'NONE',  ( 117.2776681442452968, -5.638512984488999180, -18.83840828888717311 ) ) ;
#26706 = EDGE_CURVE ( 'NONE', #3839, #38119, #28609, .T. ) ;
#26707 = CARTESIAN_POINT ( 'NONE',  ( 128.2184548109119930, -2.520019956603805511, -15.26558354049377009 ) ) ;
#26708 =( BOUNDED_SURFACE ( )  B_SPLINE_SURFACE ( 1, 2, ( 
 ( #36506, #36727, #13035, #2076, #20104, #30357, #5277, #29676, #43822, #15774, #26035, #33522, #2758, #16684, #33300, #12360, #40396, #43364, #43588, #16000, #29907, #5948, #2529, #2302, #19637, #12133, #33761, #9380, #40168, #40856, #33990, #39941, #19196, #9160, #23064, #19872, #36948, #44282, #33073, #8932, #12588, #22833, #8702, #16232, #22607, #1845, #26492, #5493, #5719, #19414, #30135, #44049, #12813, #16456, #9610, #40623, #23290, #37174, #23529, #37415, #44730, #28061, #21212, #30577, #6419, #41532, #10290, #7080, #27618, #34862, #24196, #38517, #27167, #44497, #6863, #13711, #13261, #38087, #20771, #34651, #17136, #7295, #31243, #27394, #3436, #35089, #31464, #10510, #41316, #23977, #41088, #233, #10075, #37863, #17354, #34213, #13489, #9846, #20989, #3650, #6641, #14146, #10736, #15, #3872, #3210, #41970, #13927, #37645, #31023, #20550, #34431, #44954, #27836, #23755, #24635, #20327, #41750, #24411, #38301, #2985, #17570, #16912, #30805, #22333, #904, #10954, #11408, #35548, #42863, #15262, #8428, #25314, #31687, #18693, #18013, #7520, #32136, #1351, #14594, #42193, #36000, #35778, #4771, #7974, #25085, #38749, #36229, #7748, #455, #14371, #21436, #4546, #21660, #35318, #18473, #32582, #11183, #38980, #21882, #24857, #4320, #29170, #18241, #25759, #11623, #14824, #43084, #28284, #15046, #11852, #28735, #17791, #32361, #4090, #31911, #42639, #39665, #25535, #39208, #676, #28513, #28958, #42417, #1128, #39441, #8202, #22111, #29398, #22772, #8875, #29621, #5219, #12078, #40569, #26432, #33466, #44224, #26880, #32796, #4994, #5666, #19362, #9329, #8650, #2023, #15947, #39888, #36671, #40799, #43993, #18907, #43309, #19584, #9102, #25983, #33250, #29849, #22550, #12985, #1570, #26204, #2245, #36451, #15491, #12306, #43765, #23471, #23237, #16399, #19136, #16175, #33019, #37119, #5893, #12754, #9554, #30079, #26655, #12531, #1793, #15720, #19815, #30297, #5442, #40338, #43537, #33702, #2474, #23003, #40111, #36896, #10236, #20047, #20940, #27782, #10459 ),
 ( #3161, #17083, #13872, #34380, #41695, #30975, #176, #33930, #37356, #13657, #20501, #6128, #44899, #27565, #41479, #23928, #14091, #38037, #34159, #24144, #28010, #38248, #17303, #2931, #30752, #2700, #7028, #16860, #20273, #16629, #24362, #34813, #44674, #3597, #17510, #6812, #41916, #10019, #31409, #20720, #44445, #37808, #13437, #41261, #27341, #34599, #10680, #30523, #13212, #3384, #31194, #6583, #27111, #45114, #41034, #9790, #23701, #37590, #6362, #18183, #42364, #4495, #22056, #15212, #32078, #38466, #25482, #24801, #14317, #38920, #8152, #21377, #3813, #42812, #42584, #11574, #14768, #31858, #402, #29118, #14538, #7240, #21155, #28233, #11345, #28454, #42140, #25257, #39386, #17959, #626, #28681, #17735, #11125, #35948, #25025, #32527, #4720, #31633, #10901, #7689, #38693, #35030, #39154, #43030, #24582, #21604, #7459, #35492, #35260, #4036, #4264, #846, #32310, #28902, #7919, #21828, #35722, #14988, #18418, #1076, #18637, #1300, #11798, #32745, #22720, #36620, #33411, #8819, #16118, #5395, #19762, #8373, #25706, #33193, #40053, #39611, #19313, #1969, #15895, #43486, #33644, #12478, #8599, #29795, #2420, #12703, #36843, #22499, #5164, #22280, #26603, #36393, #19081, #43706, #15440, #32968, #40517, #30020, #26149, #26377, #40288, #23187, #39836, #2191, #12255, #1743, #36173, #15667, #5838, #9050, #5612, #22952, #9279, #4939, #19535, #37065, #43938, #16344, #30247, #18854, #1519, #29568, #29346, #43259, #12025, #25927, #6069, #10186, #13156, #23644, #40743, #27511, #9734, #23415, #16807, #2878, #37531, #44392, #19989, #34547, #20448, #41429, #38814, #21497, #26831, #44171, #44849, #13386, #3328, #2645, #41203, #9962, #33876, #30700, #35382, #37986, #12934, #37303, #13601, #3105, #16577, #27290, #23875, #30472, #7583, #9501, #20222, #24092, #27058, #40978, #6303, #37761, #18076, #17250, #11017, #34108, #6762, #44620, #31138, #521, #20671, #4161, #14433, #28341, #6530, #34331, #17032, #42254, #24918, #30922, #29016, #42702, #39723, #8488, #18529, #28796 ) ),
 .UNSPECIFIED., .F., .F., .F. ) 
 B_SPLINE_SURFACE_WITH_KNOTS ( ( 2, 2 ),
 ( 3, 2, 2, 2, 2, 2, 2, 2, 2, 2, 2, 2, 2, 2, 2, 2, 2, 2, 2, 2, 2, 2, 2, 2, 2, 2, 2, 2, 2, 2, 2, 2, 2, 2, 2, 2, 2, 2, 2, 2, 2, 2, 2, 2, 2, 2, 2, 2, 2, 2, 2, 2, 2, 2, 2, 2, 2, 2, 2, 2, 2, 2, 2, 2, 2, 2, 2, 2, 2, 2, 2, 2, 2, 2, 2, 2, 2, 2, 2, 2, 2, 2, 2, 2, 2, 2, 2, 2, 2, 2, 2, 2, 2, 2, 2, 2, 2, 2, 2, 2, 2, 2, 2, 2, 2, 2, 2, 2, 2, 2, 2, 2, 2, 2, 2, 2, 2, 2, 2, 2, 2, 2, 2, 2, 2, 2, 2, 2, 3 ),
 ( 0.000000000000000000, 1.000000000000000000 ),
 ( 0.000000000000000000, 0.007812500000000000000, 0.01562500000000000000, 0.02343750000000000000, 0.03125000000000000000, 0.03906250000000000000, 0.04687500000000000000, 0.05468750000000000000, 0.06250000000000000000, 0.07031250000000000000, 0.07812500000000000000, 0.08593750000000000000, 0.09375000000000000000, 0.1015625000000000000, 0.1093750000000000000, 0.1171875000000000000, 0.1250000000000000000, 0.1328125000000000000, 0.1406250000000000000, 0.1484375000000000000, 0.1562500000000000000, 0.1640625000000000000, 0.1718750000000000000, 0.1796875000000000000, 0.1875000000000000000, 0.1953125000000000000, 0.2031250000000000000, 0.2109375000000000000, 0.2187500000000000000, 0.2265625000000000000, 0.2343750000000000000, 0.2421875000000000000, 0.2500000000000000000, 0.2578125000000000000, 0.2656250000000000000, 0.2734375000000000000, 0.2812500000000000000, 0.2890625000000000000, 0.2968750000000000000, 0.3046875000000000000, 0.3125000000000000000, 0.3203125000000000000, 0.3281250000000000000, 0.3359375000000000000, 0.3437500000000000000, 0.3515625000000000000, 0.3593750000000000000, 0.3671875000000000000, 0.3750000000000000000, 0.3828125000000000000, 0.3906250000000000000, 0.3984375000000000000, 0.4062500000000000000, 0.4140625000000000000, 0.4218750000000000000, 0.4296875000000000000, 0.4375000000000000000, 0.4453125000000000000, 0.4531250000000000000, 0.4609375000000000000, 0.4687500000000000000, 0.4765625000000000000, 0.4843750000000000000, 0.4921875000000000000, 0.5000000000000000000, 0.5078125000000000000, 0.5156250000000000000, 0.5234375000000000000, 0.5312500000000000000, 0.5390625000000000000, 0.5468750000000000000, 0.5546875000000000000, 0.5625000000000000000, 0.5703125000000000000, 0.5781250000000000000, 0.5859375000000000000, 0.5937500000000000000, 0.6015625000000000000, 0.6093750000000000000, 0.6171875000000000000, 0.6250000000000000000, 0.6328125000000000000, 0.6406250000000000000, 0.6484375000000000000, 0.6562500000000000000, 0.6640625000000000000, 0.6718750000000000000, 0.6796875000000000000, 0.6875000000000000000, 0.6953125000000000000, 0.7031250000000000000, 0.7109375000000000000, 0.7187500000000000000, 0.7265625000000000000, 0.7343750000000000000, 0.7421875000000000000, 0.7500000000000000000, 0.7578125000000000000, 0.7656250000000000000, 0.7734375000000000000, 0.7812500000000000000, 0.7890625000000000000, 0.7968750000000000000, 0.8046875000000000000, 0.8125000000000000000, 0.8203125000000000000, 0.8281250000000000000, 0.8359375000000000000, 0.8437500000000000000, 0.8515625000000000000, 0.8593750000000000000, 0.8671875000000000000, 0.8750000000000000000, 0.8828125000000000000, 0.8906250000000000000, 0.8984375000000000000, 0.9062500000000000000, 0.9140625000000000000, 0.9218750000000000000, 0.9296875000000000000, 0.9375000000000000000, 0.9453125000000000000, 0.9531250000000000000, 0.9609375000000000000, 0.9687500000000000000, 0.9765625000000000000, 0.9843750000000000000, 0.9921875000000000000, 1.000000000000000000 ),
 .UNSPECIFIED. ) 
 GEOMETRIC_REPRESENTATION_ITEM ( )  RATIONAL_B_SPLINE_SURFACE ( (
 ( 1.000000000000000000, 0.9238795325112869605, 1.000000000000000000, 0.9238795325112869605, 1.000000000000000000, 0.9238795325112869605, 1.000000000000000000, 0.9238795325112869605, 1.000000000000000000, 0.9238795325112869605, 1.000000000000000000, 0.9238795325112869605, 1.000000000000000000, 0.9238795325112869605, 1.000000000000000000, 0.9238795325112869605, 1.000000000000000000, 0.9238795325112869605, 1.000000000000000000, 0.9238795325112869605, 1.000000000000000000, 0.9238795325112869605, 1.000000000000000000, 0.9238795325112869605, 1.000000000000000000, 0.9238795325112869605, 1.000000000000000000, 0.9238795325112869605, 1.000000000000000000, 0.9238795325112869605, 1.000000000000000000, 0.9238795325112869605, 1.000000000000000000, 0.9238795325112869605, 1.000000000000000000, 0.9238795325112869605, 1.000000000000000000, 0.9238795325112869605, 1.000000000000000000, 0.9238795325112869605, 1.000000000000000000, 0.9238795325112869605, 1.000000000000000000, 0.9238795325112869605, 1.000000000000000000, 0.9238795325112869605, 1.000000000000000000, 0.9238795325112869605, 1.000000000000000000, 0.9238795325112869605, 1.000000000000000000, 0.9238795325112869605, 1.000000000000000000, 0.9238795325112869605, 1.000000000000000000, 0.9238795325112869605, 1.000000000000000000, 0.9238795325112869605, 1.000000000000000000, 0.9238795325112869605, 1.000000000000000000, 0.9238795325112869605, 1.000000000000000000, 0.9238795325112869605, 1.000000000000000000, 0.9238795325112869605, 1.000000000000000000, 0.9238795325112869605, 1.000000000000000000, 0.9238795325112869605, 1.000000000000000000, 0.9238795325112869605, 1.000000000000000000, 0.9238795325112869605, 1.000000000000000000, 0.9238795325112869605, 1.000000000000000000, 0.9238795325112869605, 1.000000000000000000, 0.9238795325112869605, 1.000000000000000000, 0.9238795325112869605, 1.000000000000000000, 0.9238795325112869605, 1.000000000000000000, 0.9238795325112869605, 1.000000000000000000, 0.9238795325112869605, 1.000000000000000000, 0.9238795325112869605, 1.000000000000000000, 0.9238795325112869605, 1.000000000000000000, 0.9238795325112869605, 1.000000000000000000, 0.9238795325112869605, 1.000000000000000000, 0.9238795325112869605, 1.000000000000000000, 0.9238795325112869605, 1.000000000000000000, 0.9238795325112869605, 1.000000000000000000, 0.9238795325112869605, 1.000000000000000000, 0.9238795325112869605, 1.000000000000000000, 0.9238795325112869605, 1.000000000000000000, 0.9238795325112869605, 1.000000000000000000, 0.9238795325112869605, 1.000000000000000000, 0.9238795325112869605, 1.000000000000000000, 0.9238795325112869605, 1.000000000000000000, 0.9238795325112869605, 1.000000000000000000, 0.9238795325112869605, 1.000000000000000000, 0.9238795325112869605, 1.000000000000000000, 0.9238795325112869605, 1.000000000000000000, 0.9238795325112869605, 1.000000000000000000, 0.9238795325112869605, 1.000000000000000000, 0.9238795325112869605, 1.000000000000000000, 0.9238795325112869605, 1.000000000000000000, 0.9238795325112869605, 1.000000000000000000, 0.9238795325112869605, 1.000000000000000000, 0.9238795325112869605, 1.000000000000000000, 0.9238795325112869605, 1.000000000000000000, 0.9238795325112869605, 1.000000000000000000, 0.9238795325112869605, 1.000000000000000000, 0.9238795325112869605, 1.000000000000000000, 0.9238795325112869605, 1.000000000000000000, 0.9238795325112869605, 1.000000000000000000, 0.9238795325112869605, 1.000000000000000000, 0.9238795325112869605, 1.000000000000000000, 0.9238795325112869605, 1.000000000000000000, 0.9238795325112869605, 1.000000000000000000, 0.9238795325112869605, 1.000000000000000000, 0.9238795325112869605, 1.000000000000000000, 0.9238795325112869605, 1.000000000000000000, 0.9238795325112869605, 1.000000000000000000, 0.9238795325112869605, 1.000000000000000000, 0.9238795325112869605, 1.000000000000000000, 0.9238795325112869605, 1.000000000000000000, 0.9238795325112869605, 1.000000000000000000, 0.9238795325112869605, 1.000000000000000000, 0.9238795325112869605, 1.000000000000000000, 0.9238795325112869605, 1.000000000000000000, 0.9238795325112869605, 1.000000000000000000, 0.9238795325112869605, 1.000000000000000000, 0.9238795325112869605, 1.000000000000000000, 0.9238795325112869605, 1.000000000000000000, 0.9238795325112869605, 1.000000000000000000, 0.9238795325112869605, 1.000000000000000000, 0.9238795325112869605, 1.000000000000000000, 0.9238795325112869605, 1.000000000000000000, 0.9238795325112869605, 1.000000000000000000, 0.9238795325112869605, 1.000000000000000000, 0.9238795325112869605, 1.000000000000000000, 0.9238795325112869605, 1.000000000000000000, 0.9238795325112869605, 1.000000000000000000, 0.9238795325112869605, 1.000000000000000000, 0.9238795325112869605, 1.000000000000000000, 0.9238795325112869605, 1.000000000000000000, 0.9238795325112869605, 1.000000000000000000, 0.9238795325112869605, 1.000000000000000000, 0.9238795325112869605, 1.000000000000000000, 0.9238795325112869605, 1.000000000000000000, 0.9238795325112869605, 1.000000000000000000, 0.9238795325112869605, 1.000000000000000000, 0.9238795325112869605, 1.000000000000000000, 0.9238795325112869605, 1.000000000000000000, 0.9238795325112869605, 1.000000000000000000, 0.9238795325112869605, 1.000000000000000000, 0.9238795325112869605, 1.000000000000000000, 0.9238795325112869605, 1.000000000000000000, 0.9238795325112869605, 1.000000000000000000, 0.9238795325112869605, 1.000000000000000000, 0.9238795325112869605, 1.000000000000000000, 0.9238795325112869605, 1.000000000000000000, 0.9238795325112869605, 1.000000000000000000, 0.9238795325112869605, 1.000000000000000000, 0.9238795325112869605, 1.000000000000000000, 0.9238795325112869605, 1.000000000000000000, 0.9238795325112869605, 1.000000000000000000, 0.9238795325112869605, 1.000000000000000000),
 ( 1.000000000000000000, 0.9238795325112869605, 1.000000000000000000, 0.9238795325112869605, 1.000000000000000000, 0.9238795325112869605, 1.000000000000000000, 0.9238795325112869605, 1.000000000000000000, 0.9238795325112869605, 1.000000000000000000, 0.9238795325112869605, 1.000000000000000000, 0.9238795325112869605, 1.000000000000000000, 0.9238795325112869605, 1.000000000000000000, 0.9238795325112869605, 1.000000000000000000, 0.9238795325112869605, 1.000000000000000000, 0.9238795325112869605, 1.000000000000000000, 0.9238795325112869605, 1.000000000000000000, 0.9238795325112869605, 1.000000000000000000, 0.9238795325112869605, 1.000000000000000000, 0.9238795325112869605, 1.000000000000000000, 0.9238795325112869605, 1.000000000000000000, 0.9238795325112869605, 1.000000000000000000, 0.9238795325112869605, 1.000000000000000000, 0.9238795325112869605, 1.000000000000000000, 0.9238795325112869605, 1.000000000000000000, 0.9238795325112869605, 1.000000000000000000, 0.9238795325112869605, 1.000000000000000000, 0.9238795325112869605, 1.000000000000000000, 0.9238795325112869605, 1.000000000000000000, 0.9238795325112869605, 1.000000000000000000, 0.9238795325112869605, 1.000000000000000000, 0.9238795325112869605, 1.000000000000000000, 0.9238795325112869605, 1.000000000000000000, 0.9238795325112869605, 1.000000000000000000, 0.9238795325112869605, 1.000000000000000000, 0.9238795325112869605, 1.000000000000000000, 0.9238795325112869605, 1.000000000000000000, 0.9238795325112869605, 1.000000000000000000, 0.9238795325112869605, 1.000000000000000000, 0.9238795325112869605, 1.000000000000000000, 0.9238795325112869605, 1.000000000000000000, 0.9238795325112869605, 1.000000000000000000, 0.9238795325112869605, 1.000000000000000000, 0.9238795325112869605, 1.000000000000000000, 0.9238795325112869605, 1.000000000000000000, 0.9238795325112869605, 1.000000000000000000, 0.9238795325112869605, 1.000000000000000000, 0.9238795325112869605, 1.000000000000000000, 0.9238795325112869605, 1.000000000000000000, 0.9238795325112869605, 1.000000000000000000, 0.9238795325112869605, 1.000000000000000000, 0.9238795325112869605, 1.000000000000000000, 0.9238795325112869605, 1.000000000000000000, 0.9238795325112869605, 1.000000000000000000, 0.9238795325112869605, 1.000000000000000000, 0.9238795325112869605, 1.000000000000000000, 0.9238795325112869605, 1.000000000000000000, 0.9238795325112869605, 1.000000000000000000, 0.9238795325112869605, 1.000000000000000000, 0.9238795325112869605, 1.000000000000000000, 0.9238795325112869605, 1.000000000000000000, 0.9238795325112869605, 1.000000000000000000, 0.9238795325112869605, 1.000000000000000000, 0.9238795325112869605, 1.000000000000000000, 0.9238795325112869605, 1.000000000000000000, 0.9238795325112869605, 1.000000000000000000, 0.9238795325112869605, 1.000000000000000000, 0.9238795325112869605, 1.000000000000000000, 0.9238795325112869605, 1.000000000000000000, 0.9238795325112869605, 1.000000000000000000, 0.9238795325112869605, 1.000000000000000000, 0.9238795325112869605, 1.000000000000000000, 0.9238795325112869605, 1.000000000000000000, 0.9238795325112869605, 1.000000000000000000, 0.9238795325112869605, 1.000000000000000000, 0.9238795325112869605, 1.000000000000000000, 0.9238795325112869605, 1.000000000000000000, 0.9238795325112869605, 1.000000000000000000, 0.9238795325112869605, 1.000000000000000000, 0.9238795325112869605, 1.000000000000000000, 0.9238795325112869605, 1.000000000000000000, 0.9238795325112869605, 1.000000000000000000, 0.9238795325112869605, 1.000000000000000000, 0.9238795325112869605, 1.000000000000000000, 0.9238795325112869605, 1.000000000000000000, 0.9238795325112869605, 1.000000000000000000, 0.9238795325112869605, 1.000000000000000000, 0.9238795325112869605, 1.000000000000000000, 0.9238795325112869605, 1.000000000000000000, 0.9238795325112869605, 1.000000000000000000, 0.9238795325112869605, 1.000000000000000000, 0.9238795325112869605, 1.000000000000000000, 0.9238795325112869605, 1.000000000000000000, 0.9238795325112869605, 1.000000000000000000, 0.9238795325112869605, 1.000000000000000000, 0.9238795325112869605, 1.000000000000000000, 0.9238795325112869605, 1.000000000000000000, 0.9238795325112869605, 1.000000000000000000, 0.9238795325112869605, 1.000000000000000000, 0.9238795325112869605, 1.000000000000000000, 0.9238795325112869605, 1.000000000000000000, 0.9238795325112869605, 1.000000000000000000, 0.9238795325112869605, 1.000000000000000000, 0.9238795325112869605, 1.000000000000000000, 0.9238795325112869605, 1.000000000000000000, 0.9238795325112869605, 1.000000000000000000, 0.9238795325112869605, 1.000000000000000000, 0.9238795325112869605, 1.000000000000000000, 0.9238795325112869605, 1.000000000000000000, 0.9238795325112869605, 1.000000000000000000, 0.9238795325112869605, 1.000000000000000000, 0.9238795325112869605, 1.000000000000000000, 0.9238795325112869605, 1.000000000000000000, 0.9238795325112869605, 1.000000000000000000, 0.9238795325112869605, 1.000000000000000000, 0.9238795325112869605, 1.000000000000000000, 0.9238795325112869605, 1.000000000000000000, 0.9238795325112869605, 1.000000000000000000, 0.9238795325112869605, 1.000000000000000000, 0.9238795325112869605, 1.000000000000000000, 0.9238795325112869605, 1.000000000000000000, 0.9238795325112869605, 1.000000000000000000, 0.9238795325112869605, 1.000000000000000000, 0.9238795325112869605, 1.000000000000000000, 0.9238795325112869605, 1.000000000000000000, 0.9238795325112869605, 1.000000000000000000, 0.9238795325112869605, 1.000000000000000000, 0.9238795325112869605, 1.000000000000000000, 0.9238795325112869605, 1.000000000000000000, 0.9238795325112869605, 1.000000000000000000, 0.9238795325112869605, 1.000000000000000000, 0.9238795325112869605, 1.000000000000000000, 0.9238795325112869605, 1.000000000000000000) ) ) 
 REPRESENTATION_ITEM ( '' )  SURFACE ( )  );
#26709 = CARTESIAN_POINT ( 'NONE',  ( 125.6164881442453094, -9.565557343593413364, -10.61323700422348004 ) ) ;
#26710 = CARTESIAN_POINT ( 'NONE',  ( 118.0718414775786442, -0.8288870151387760510, -10.36305467784173118 ) ) ;
#26711 = ORIENTED_EDGE ( 'NONE', *, *, #41864, .T. ) ;
#26712 = EDGE_CURVE ( 'NONE', #21997, #26397, #38572, .T. ) ;
#26713 = CARTESIAN_POINT ( 'NONE',  ( 121.4797829359119987, -4.283928203966213211, -7.183505701512925334 ) ) ;
#26714 = CIRCLE ( 'NONE', #16571, 2.999999999999999556 ) ;
#26715 = CARTESIAN_POINT ( 'NONE',  ( 119.8303681442453126, 0.4262465694468514643, -12.03445270309931736 ) ) ;
#26716 = ORIENTED_EDGE ( 'NONE', *, *, #216, .T. ) ;
#26717 = CARTESIAN_POINT ( 'NONE',  ( 123.0772048109119652, -2.527210466738041728, -8.967976844669124148 ) ) ;
#26718 = CARTESIAN_POINT ( 'NONE',  ( 117.9583881442453048, -10.30919188438810075, -12.61870101168855918 ) ) ;
#26719 = CARTESIAN_POINT ( 'NONE',  ( 112.7050671295247923, -10.62599879583958540, -13.39321520033831447 ) ) ;
#26720 = CARTESIAN_POINT ( 'NONE',  ( 116.7671281442453335, -7.643976991954077427, -18.09477374809248928 ) ) ;
#26721 = CONICAL_SURFACE ( 'NONE', #10706, 5.999999999999997335, 0.4636476090008060935 ) ;
#26722 = ORIENTED_EDGE ( 'NONE', *, *, #37597, .T. ) ;
#26723 = ORIENTED_EDGE ( 'NONE', *, *, #26557, .F. ) ;
#26724 = CARTESIAN_POINT ( 'NONE',  ( 125.5597614775786326, -7.894159318335828068, -9.358103419637847864 ) ) ;
#26725 = CARTESIAN_POINT ( 'NONE',  ( 120.8514481442452961, -2.084020599724406786, -8.691656652584148546 ) ) ;
#26726 = FACE_OUTER_BOUND ( 'NONE', #9331, .T. ) ;
#26727 = AXIS2_PLACEMENT_3D ( 'NONE', #14727, #31820, #24987 ) ;
#26728 = CARTESIAN_POINT ( 'NONE',  ( 143.3676850761856940, -49.76310523276723785, -13.39321520033831447 ) ) ;
#26729 = CARTESIAN_POINT ( 'NONE',  ( 117.5613014775786525, 0.9020085738987339008, -11.91225656197089222 ) ) ;
#26730 = EDGE_CURVE ( 'NONE', #43772, #23418, #35193, .T. ) ;
#26731 = CARTESIAN_POINT ( 'NONE',  ( 108.2600671295247992, -10.62599879583958540, -13.39321520033831447 ) ) ;
#26732 = CARTESIAN_POINT ( 'NONE',  ( 118.6958348109119754, -6.344957434206665248, -7.627207830600338134 ) ) ;
#26733 = PRODUCT_DEFINITION_SHAPE ( 'NONE', 'NONE',  #45155 ) ;
#26735 = CARTESIAN_POINT ( 'NONE',  ( 114.6115148109119986, -6.222761293078241884, -8.102969835052219238 ) ) ;
#26734 = CARTESIAN_POINT ( 'NONE',  ( 115.3489614775786407, -9.261995988541697145, -16.69588392320189030 ) ) ;
#26736 = CYLINDRICAL_SURFACE ( 'NONE', #4329, 25.00000000000000355 ) ;
#26737 = CARTESIAN_POINT ( 'NONE',  ( 114.1577014775786552, -6.344957434206662583, -7.627207830600332805 ) ) ;
#26738 = ORIENTED_EDGE ( 'NONE', *, *, #401, .T. ) ;
#26739 = CARTESIAN_POINT ( 'NONE',  ( 123.6877814775786533, -6.222761293078241884, -8.102969835052219238 ) ) ;
#26740 = CARTESIAN_POINT ( 'NONE',  ( 123.5176014775786228, -9.261995988541684710, -16.69588392320190806 ) ) ;
#26741 = EDGE_CURVE ( 'NONE', #16290, #22059, #10293, .T. ) ;
#26742 = B_SPLINE_CURVE_WITH_KNOTS ( 'NONE', 3,
 ( #9802, #2486, #16640, #44687, #6140, #27353, #16872, #33715, #40581, #34611 ),
 .UNSPECIFIED., .F., .F.,
 ( 4, 3, 3, 4 ),
 ( 0.000000000000000000, 0.0001671877548681284921, 0.0003343755096277705222, 0.0006463528481650609656 ),
 .UNSPECIFIED. ) ;
#26743 = DIRECTION ( 'NONE',  ( 0.9908103287288504424, -0.1352586133457958917, 0.000000000000000000 ) ) ;
#26744 = CARTESIAN_POINT ( 'NONE',  ( 111.8021765045248372, -7.250697342233347165, -19.15521520033831138 ) ) ;
#26745 = CARTESIAN_POINT ( 'NONE',  ( 111.6632702545248605, 0.1403307496149616695, -11.32035403202665336 ) ) ;
#26746 = CARTESIAN_POINT ( 'NONE',  ( 111.1770983795247787, -0.7896495226426338832, -9.318865927141430916 ) ) ;
#26747 = AXIS2_PLACEMENT_3D ( 'NONE', #21734, #531, #25160 ) ;
#26748 = CARTESIAN_POINT ( 'NONE',  ( 122.4965214775786251, -10.30919188438810075, -12.61870101168855918 ) ) ;
#26749 = VERTEX_POINT ( 'NONE', #1006 ) ;
#26750 = CARTESIAN_POINT ( 'NONE',  ( 120.5678148109119832, -8.166667518702819706, -8.995218007635861213 ) ) ;
#26751 = CARTESIAN_POINT ( 'NONE',  ( 112.5126281442453120, 0.1319031606808879209, -14.10382304977623669 ) ) ;
#26752 = CARTESIAN_POINT ( 'NONE',  ( 59.95220766929347889, -14.75932518950460981, -19.37269899291708697 ) ) ;
#26753 = CARTESIAN_POINT ( 'NONE',  ( 121.4187148109119789, -6.344957434206665248, -7.627207830600338134 ) ) ;
#26754 = CARTESIAN_POINT ( 'NONE',  ( 121.9292548109119849, -1.561330072975668948, -17.79121239304076951 ) ) ;
#26755 = CARTESIAN_POINT ( 'NONE',  ( 62.61495183759026162, -3.463885907106070139, -19.20140212329127039 ) ) ;
#26756 = CARTESIAN_POINT ( 'NONE',  ( 123.0637881442452937, -8.899110576539710493, -16.42337572283490132 ) ) ;
#26757 = CARTESIAN_POINT ( 'NONE',  ( 125.4584548109120021, -8.650253244288707677, -17.84358828606593050 ) ) ;
#26758 = CARTESIAN_POINT ( 'NONE',  ( 111.8471337256649036, -1.063912429576150842, -17.20460841810474406 ) ) ;
#26759 = ORIENTED_EDGE ( 'NONE', *, *, #22236, .F. ) ;
#26760 = CARTESIAN_POINT ( 'NONE',  ( -2.793826376213096818, -7.122619984182616548, -7.420824263456360370 ) ) ;
#26761 = CARTESIAN_POINT ( 'NONE',  ( 118.7342755643466745, -1.244021962887374544, -16.96476564598603076 ) ) ;
#26762 = CARTESIAN_POINT ( 'NONE',  ( 123.9146881442452894, -10.15424416112533912, -14.75197769757731336 ) ) ;
#26763 = CARTESIAN_POINT ( 'NONE',  ( 107.9822546295247889, -4.863998795839590272, -18.39754474579285315 ) ) ;
#26764 = CARTESIAN_POINT ( 'NONE',  ( 112.9134265045247645, -2.791137627527939813, -8.388885654883777576 ) ) ;
#26765 = CARTESIAN_POINT ( 'NONE',  ( 116.3133148109120043, -2.084020599724406786, -8.691656652584148546 ) ) ;
#26766 = DIRECTION ( 'NONE',  ( 0.000000000000000000, 0.000000000000000000, 1.000000000000000000 ) ) ;
#26767 = CARTESIAN_POINT ( 'NONE',  ( 71.45370786120086848, -25.93374482621613808, -5.221195830126694304 ) ) ;
#26768 = CARTESIAN_POINT ( 'NONE',  ( 115.6893214775786447, -9.859900752359374465, -12.68260735090039404 ) ) ;
#26769 = CARTESIAN_POINT ( 'NONE',  ( 121.8158014775786171, -5.638512984488999180, -18.83840828888717311 ) ) ;
#26770 = ORIENTED_EDGE ( 'NONE', *, *, #27842, .F. ) ;
#26771 = EDGE_CURVE ( 'NONE', #7134, #21997, #42518, .T. ) ;
#26772 = CARTESIAN_POINT ( 'NONE',  ( 120.8514481442452961, -2.084020599724406786, -8.691656652584148546 ) ) ;
#26773 = CARTESIAN_POINT ( 'NONE',  ( 117.6180281442453150, -0.4660016031367893996, -10.09054647747474043 ) ) ;
#26774 = CARTESIAN_POINT ( 'NONE',  ( 123.4041481442452834, -10.30919188438810075, -12.61870101168855918 ) ) ;
#26775 = CARTESIAN_POINT ( 'NONE',  ( 121.7023481442452777, -0.8288870151387760510, -10.36305467784173118 ) ) ;
#26776 = ORIENTED_EDGE ( 'NONE', *, *, #27007, .F. ) ;
#26777 = EDGE_CURVE ( 'NONE', #39048, #31742, #37549, .T. ) ;
#26778 = CARTESIAN_POINT ( 'NONE',  ( 120.9241579359119925, -4.360204210389833968, -8.000047426360245240 ) ) ;
#26779 = CARTESIAN_POINT ( 'NONE',  ( 123.5743281442453139, -7.893985811506177619, -18.51759400769804742 ) ) ;
#26780 = CARTESIAN_POINT ( 'NONE',  ( 113.3068014775786594, -1.833838273342658809, -17.42832698103878286 ) ) ;
#26781 = CONICAL_SURFACE ( 'NONE', #29668, 2.445500000000001339, 0.7853981633974680410 ) ;
#26782 = CARTESIAN_POINT ( 'NONE',  ( 124.1983214775786166, -8.166667518702819706, -8.995218007635861213 ) ) ;
#26783 = CARTESIAN_POINT ( 'NONE',  ( 108.8851452545248151, 0.8980012041604421569, -11.00651665394454071 ) ) ;
#26784 = DIRECTION ( 'NONE',  ( 0.1352586133458071049, 0.9908103287288489991, 0.000000000000000000 ) ) ;
#26785 = VERTEX_POINT ( 'NONE', #24200 ) ;
#26786 = CARTESIAN_POINT ( 'NONE',  ( 110.2742077545248094, -2.791137627527939813, -18.39754474579286025 ) ) ;
#26787 = CARTESIAN_POINT ( 'NONE',  ( 123.0077516859119839, -0.6942167230862511529, -9.935906262978006609 ) ) ;
#26788 = CARTESIAN_POINT ( 'NONE',  ( 120.9649014775786355, -6.222761293078241884, -8.102969835052219238 ) ) ;
#26789 = CARTESIAN_POINT ( 'NONE',  ( 115.1787814775786387, -0.1624402480850797581, -16.17319339645315424 ) ) ;
#26790 = CARTESIAN_POINT ( 'NONE',  ( 127.0545391123781798, -6.690369086889063510, -18.49686471125335530 ) ) ;
#26791 = ORIENTED_EDGE ( 'NONE', *, *, #20500, .T. ) ;
#26792 = CARTESIAN_POINT ( 'NONE',  ( 86.34560043013698305, -9.320000780048239619, -16.89321520033831447 ) ) ;
#26793 = CARTESIAN_POINT ( 'NONE',  ( 117.5045748109119756, -9.859900752359374465, -12.68260735090039404 ) ) ;
#26794 = CARTESIAN_POINT ( 'NONE',  ( 113.4202548109119846, 0.1319031606808879209, -14.10382304977623669 ) ) ;
#26795 = DIRECTION ( 'NONE',  ( 0.000000000000000000, -0.3818493186865936084, 0.9242245927363024194 ) ) ;
#26797 = CARTESIAN_POINT ( 'NONE',  ( 121.8158014775786171, -5.638512984488999180, -18.83840828888717311 ) ) ;
#26796 = CARTESIAN_POINT ( 'NONE',  ( 128.2184548109119930, -4.863998795839242995, -13.39321520033831447 ) ) ;
#26798 = CARTESIAN_POINT ( 'NONE',  ( 112.7962614775786676, -3.383040157471821630, -19.15922257007629170 ) ) ;
#26799 = EDGE_LOOP ( 'NONE', ( #37306, #5841, #26638, #8211 ) ) ;
#26800 = FACE_BOUND ( 'NONE', #38804, .T. ) ;
#26801 = CARTESIAN_POINT ( 'NONE',  ( 126.7702028005564756, 0.1629706377663181216, -14.99492149720868994 ) ) ;
#26802 = CARTESIAN_POINT ( 'NONE',  ( 107.1488171295247867, 0.1403307496149613920, -13.39321520033831447 ) ) ;
#26803 = EDGE_CURVE ( 'NONE', #21214, #3126, #237, .T. ) ;
#26804 = CARTESIAN_POINT ( 'NONE',  ( 111.7184548109119788, -9.261995988541697145, -16.69588392320189030 ) ) ;
#26805 = CARTESIAN_POINT ( 'NONE',  ( 120.6245414775786458, -0.1624402480850797581, -16.17319339645315424 ) ) ;
#26806 = DIRECTION ( 'NONE',  ( -1.000000000000000000, 0.000000000000000000, -0.000000000000000000 ) ) ;
#26807 = CARTESIAN_POINT ( 'NONE',  ( 112.4967077545247633, -2.791137627527939813, -18.39754474579286025 ) ) ;
#26808 = CARTESIAN_POINT ( 'NONE',  ( 9.052690036452151645, -4.182915634381243919, -19.39321520033831447 ) ) ;
#26809 = DIRECTION ( 'NONE',  ( 0.7871354856660198740, 0.4483307682966886643, 0.4235767337848242442 ) ) ;
#26810 = CARTESIAN_POINT ( 'NONE',  ( 113.5337081442453240, -0.8288870151387760510, -10.36305467784173118 ) ) ;
#26811 = CARTESIAN_POINT ( 'NONE',  ( 111.3854577545248645, -7.250697342233347165, -7.631215200338321125 ) ) ;
#26812 = DIRECTION ( 'NONE',  ( 0.000000000000000000, -0.8842819633428466997, 0.4669533266896385149 ) ) ;
#26813 = CARTESIAN_POINT ( 'NONE',  ( 112.0799890045248475, 0.8980012041604421569, -15.77991374673208469 ) ) ;
#26814 = CARTESIAN_POINT ( 'NONE',  ( 125.1626748109119802, -9.988377603198980381, -10.36322818467138518 ) ) ;
#26815 = CARTESIAN_POINT ( 'NONE',  ( 120.9081748109119872, -5.638512984488999180, -18.83840828888717311 ) ) ;
#26816 = DIRECTION ( 'NONE',  ( 0.000000000000000000, 0.000000000000000000, -1.000000000000000000 ) ) ;
#26817 = CARTESIAN_POINT ( 'NONE',  ( 118.3554748109119998, 0.2603800115204892296, -16.42320221600525088 ) ) ;
#26818 = CARTESIAN_POINT ( 'NONE',  ( 112.2289948109119848, -1.834011780172310813, -8.268836392978581529 ) ) ;
#26819 = EDGE_LOOP ( 'NONE', ( #16826, #40170, #26922, #11669, #716, #28787, #37553, #23951, #7088, #28905 ) ) ;
#26820 = CARTESIAN_POINT ( 'NONE',  ( 113.9307948109119764, -10.15424416112533912, -14.75197769757731336 ) ) ;
#26821 = CARTESIAN_POINT ( 'NONE',  ( 112.3424481442453384, -3.505236298600246325, -18.68346056562440793 ) ) ;
#26822 = CARTESIAN_POINT ( 'NONE',  ( 120.1140014775786398, -1.561330072975668504, -17.79121239304076951 ) ) ;
#26823 = ADVANCED_FACE ( 'NONE', ( #13493 ), #34655, .F. ) ;
#26824 = CARTESIAN_POINT ( 'NONE',  ( 113.3635281442453504, -9.988377603198976828, -10.36322818467138340 ) ) ;
#26825 = EDGE_CURVE ( 'NONE', #22022, #40242, #3322, .T. ) ;
#26826 = CARTESIAN_POINT ( 'NONE',  ( 126.1837548109119211, -10.63000616557722466, -14.87417383870573495 ) ) ;
#26827 = EDGE_LOOP ( 'NONE', ( #26942, #11690, #1348, #35499, #4859 ) ) ;
#26828 = CARTESIAN_POINT ( 'NONE',  ( 117.5045748109119756, -9.859900752359374465, -12.68260735090039404 ) ) ;
#26829 = CARTESIAN_POINT ( 'NONE',  ( 124.8223148109119762, 0.9020085738987339008, -11.91225656197089222 ) ) ;
#26830 = CARTESIAN_POINT ( 'NONE',  ( 107.4266296295248821, -4.863998795839590272, -19.15521520033831493 ) ) ;
#26831 = CARTESIAN_POINT ( 'NONE',  ( 122.8936081442453059, -9.565557343593413364, -10.61323700422348004 ) ) ;
#26832 = DIRECTION ( 'NONE',  ( 0.000000000000000000, -0.3818493186865927203, 0.9242245927363029745 ) ) ;
#26833 = DIRECTION ( 'NONE',  ( 1.000000000000000000, 0.000000000000000000, 0.000000000000000000 ) ) ;
#26834 = ORIENTED_EDGE ( 'NONE', *, *, #14554, .T. ) ;
#26835 = CARTESIAN_POINT ( 'NONE',  ( 122.5215798109119874, -7.200787124940443817, -17.81845355600750835 ) ) ;
#26836 = CARTESIAN_POINT ( 'NONE',  ( 124.4252281442452812, -9.261995988541697145, -16.69588392320189030 ) ) ;
#26837 = DIRECTION ( 'NONE',  ( 0.7871354856660167654, -0.6167752151498625546, -0.002461946824136807422 ) ) ;
#26838 = CARTESIAN_POINT ( 'NONE',  ( 111.9453614775786434, -1.561330072975668060, -17.79121239304076596 ) ) ;
#26839 = AXIS2_PLACEMENT_3D ( 'NONE', #2011, #29384, #16163 ) ;
#26840 = CARTESIAN_POINT ( 'NONE',  ( 116.4318426488974580, 2.234111456617531744, -6.383118217132903283 ) ) ;
#26841 = CARTESIAN_POINT ( 'NONE',  ( 96.46827370896536991, -25.38949206727775731, -12.58586697536825660 ) ) ;
#26842 = CARTESIAN_POINT ( 'NONE',  ( 106.7320983795247855, -8.402594152722688392, -16.93181055722141792 ) ) ;
#26843 = CARTESIAN_POINT ( 'NONE',  ( 123.6462803923315334, -1.063912429576147511, -17.20460841810472985 ) ) ;
#26844 = CARTESIAN_POINT ( 'NONE',  ( 137.3111100276077821, -4.833481128352631551, -18.60023654913463531 ) ) ;
#26845 = DIRECTION ( 'NONE',  ( 0.000000000000000000, 0.4669533266896288004, 0.8842819633428518067 ) ) ;
#26846 = CARTESIAN_POINT ( 'NONE',  ( 125.3895814775786448, -7.893985811506177619, -18.51759400769804742 ) ) ;
#26847 = CARTESIAN_POINT ( 'NONE',  ( 121.4754414775786131, -1.833838273342659697, -17.42832698103878286 ) ) ;
#26848 = CARTESIAN_POINT ( 'NONE',  ( 119.7434548109119703, 0.1812605887601431154, -12.07667898593298617 ) ) ;
#26849 = ORIENTED_EDGE ( 'NONE', *, *, #27017, .T. ) ;
#26850 = CARTESIAN_POINT ( 'NONE',  ( 121.8725281442453223, -3.383040157471821630, -19.15922257007629170 ) ) ;
#26851 = CARTESIAN_POINT ( 'NONE',  ( 118.6391081442452986, -4.089484607189486809, -7.948022111789456723 ) ) ;
#26852 = CARTESIAN_POINT ( 'NONE',  ( 114.1635827545248389, -6.936859964151250502, -8.388885654883777576 ) ) ;
#26853 = CARTESIAN_POINT ( 'NONE',  ( 113.2500748109119968, -3.505236298600246325, -18.68346056562440793 ) ) ;
#26854 = CARTESIAN_POINT ( 'NONE',  ( 112.7395348109119766, -5.638512984488999180, -18.83840828888717311 ) ) ;
#26855 = CARTESIAN_POINT ( 'NONE',  ( 125.2761281442453054, -10.63000616557722466, -14.87417383870573495 ) ) ;
#26856 = CARTESIAN_POINT ( 'NONE',  ( 111.9410827545248708, -2.477300249445798297, -19.15521520033831138 ) ) ;
#26857 = CARTESIAN_POINT ( 'NONE',  ( 107.5655358795247736, -8.402594152722688392, -9.854619843455216355 ) ) ;
#26858 = CARTESIAN_POINT ( 'NONE',  ( 82.85202896377741411, -31.80474036673594540, -23.17876345974346819 ) ) ;
#26859 = CARTESIAN_POINT ( 'NONE',  ( 115.8595014775786609, -7.643976991954077427, -18.09477374809248928 ) ) ;
#26860 = CARTESIAN_POINT ( 'NONE',  ( 115.5758681442453053, -7.894159318335828068, -9.358103419637847864 ) ) ;
#26861 = DIRECTION ( 'NONE',  ( 1.000000000000000000, 0.000000000000000000, -0.000000000000000000 ) ) ;
#26862 = CARTESIAN_POINT ( 'NONE',  ( 112.3578015045248861, -6.936859964151250502, -18.39754474579286025 ) ) ;
#26863 = EDGE_LOOP ( 'NONE', ( #25056, #3371, #25954, #45064 ) ) ;
#26864 = DIRECTION ( 'NONE',  ( -0.000000000000000000, -0.9284778069183721172, -0.3713878862591650232 ) ) ;
#26865 = CARTESIAN_POINT ( 'NONE',  ( 123.8579614775786126, -9.859900752359378018, -12.68260735090039759 ) ) ;
#26866 = CARTESIAN_POINT ( 'NONE',  ( 111.9453614775786434, -1.561330072975668060, -17.79121239304076596 ) ) ;
#26867 = CARTESIAN_POINT ( 'NONE',  ( 119.7434548109119703, -2.527210466738041728, -8.967976844669124148 ) ) ;
#26868 = CARTESIAN_POINT ( 'NONE',  ( 120.4379860609119675, -3.387241619883791355, -18.17469012370385073 ) ) ;
#26869 = EDGE_LOOP ( 'NONE', ( #43071, #15815, #24691, #16182 ) ) ;
#26870 = CARTESIAN_POINT ( 'NONE',  ( 105.1346765045248475, -2.791137627527939813, -8.388885654883777576 ) ) ;
#26871 = ORIENTED_EDGE ( 'NONE', *, *, #9118, .T. ) ;
#26872 = CARTESIAN_POINT ( 'NONE',  ( 117.4478481442453131, 0.2603800115204892296, -16.42320221600525088 ) ) ;
#26873 = CARTESIAN_POINT ( 'NONE',  ( 125.5030348109119558, -6.222761293078241884, -8.102969835052219238 ) ) ;
#26874 = ADVANCED_FACE ( 'NONE', ( #24862 ), #4549, .F. ) ;
#26875 = CARTESIAN_POINT ( 'NONE',  ( 115.9162281442453235, -5.574606645277164318, -18.38911715685844683 ) ) ;
#26876 = SURFACE_STYLE_FILL_AREA ( #20041 ) ;
#26877 = CARTESIAN_POINT ( 'NONE',  ( 120.1140014775786398, -1.561330072975668504, -17.79121239304076951 ) ) ;
#26878 = CARTESIAN_POINT ( 'NONE',  ( 115.4056881442453459, -7.893985811506177619, -18.51759400769804742 ) ) ;
#26879 = CARTESIAN_POINT ( 'NONE',  ( 111.0381921295247878, -9.868328341294093420, -13.39321520033831447 ) ) ;
#26880 = CARTESIAN_POINT ( 'NONE',  ( 122.9503348109119827, 0.5811942927096110934, -14.16772938898807510 ) ) ;
#26881 = CARTESIAN_POINT ( 'NONE',  ( 83.82415148905927538, -46.76310523276723785, -4.893215200338314474 ) ) ;
#26882 = ORIENTED_EDGE ( 'NONE', *, *, #11970, .T. ) ;
#26883 = CARTESIAN_POINT ( 'NONE',  ( 119.6601881442453106, -8.166667518702819706, -8.995218007635861213 ) ) ;
#26884 = CARTESIAN_POINT ( 'NONE',  ( 113.4769814775786330, 0.4262465694468514643, -12.03445270309931736 ) ) ;
#26885 = CARTESIAN_POINT ( 'NONE',  ( 126.5561942423801014, -4.902127430340050829, -18.56199476000752568 ) ) ;
#26886 = CARTESIAN_POINT ( 'NONE',  ( 125.9001214775786224, -5.574606645277164318, -18.38911715685844683 ) ) ;
#26887 = EDGE_LOOP ( 'NONE', ( #12736, #742, #44842, #29349 ) ) ;
#26888 = CARTESIAN_POINT ( 'NONE',  ( 122.6099748109119929, -9.261995988541697145, -16.69588392320189030 ) ) ;
#26889 = CYLINDRICAL_SURFACE ( 'NONE', #34709, 3.000000000000001776 ) ;
#26890 = CARTESIAN_POINT ( 'NONE',  ( 115.8542891344827552, -1.149058757900091265, -17.09122335155388939 ) ) ;
#26891 = DIRECTION ( 'NONE',  ( 0.000000000000000000, -0.8842819633428518067, 0.4669533266896290780 ) ) ;
#26892 = LINE ( 'NONE', #26050, #40507 ) ;
#26893 = CARTESIAN_POINT ( 'NONE',  ( 116.2565881442453133, -0.8288870151387760510, -10.36305467784173118 ) ) ;
#26894 = CARTESIAN_POINT ( 'NONE',  ( 137.3374356171257489, -3.432627534740069652, -8.412905839694147403 ) ) ;
#26895 = CARTESIAN_POINT ( 'NONE',  ( 117.1642148109119859, -0.8288870151387760510, -10.36305467784173118 ) ) ;
#26896 = CARTESIAN_POINT ( 'NONE',  ( 114.5108483795247878, -8.402594152722688392, -16.93181055722141792 ) ) ;
#26897 = CONICAL_SURFACE ( 'NONE', #34153, 1.610000000000000986, 0.9599310885968765916 ) ;
#26898 = CYLINDRICAL_SURFACE ( 'NONE', #34667, 3.000000000000001776 ) ;
#26899 = CARTESIAN_POINT ( 'NONE',  ( 115.5758681442453053, -7.894159318335828068, -9.358103419637847864 ) ) ;
#26900 = CARTESIAN_POINT ( 'NONE',  ( 115.8595014775786609, -1.834011780172310813, -8.268836392978581529 ) ) ;
#26901 = CARTESIAN_POINT ( 'NONE',  ( 122.8688454359119646, 0.5291689781388270175, -13.89700978578772705 ) ) ;
#26902 = VECTOR ( 'NONE', #4184, 1000.000000000000114 ) ;
#26903 = CARTESIAN_POINT ( 'NONE',  ( 112.1155414775786454, 0.9020085738987339008, -11.91225656197089222 ) ) ;
#26904 = CARTESIAN_POINT ( 'NONE',  ( 115.1220548109119761, -1.833838273342658809, -17.42832698103878286 ) ) ;
#26905 = CARTESIAN_POINT ( 'NONE',  ( 124.0281414775786146, -1.834011780172310813, -8.268836392978581529 ) ) ;
#26906 = CARTESIAN_POINT ( 'NONE',  ( 120.2274548109119934, 0.5811942927096110934, -14.16772938898807510 ) ) ;
#26907 = ORIENTED_EDGE ( 'NONE', *, *, #11791, .F. ) ;
#26908 = CARTESIAN_POINT ( 'NONE',  ( 114.7249681442453237, 0.2603800115204892296, -16.42320221600525088 ) ) ;
#26909 = CARTESIAN_POINT ( 'NONE',  ( 111.6632702545248605, -10.62599879583958717, -15.77991374673208469 ) ) ;
#26910 = DIRECTION ( 'NONE',  ( 0.000000000000000000, -0.3818493186865936084, 0.9242245927363024194 ) ) ;
#26911 = DIRECTION ( 'NONE',  ( 0.9609149988134843001, -0.1028163501681632064, 0.2570431154366505933 ) ) ;
#26912 = CARTESIAN_POINT ( 'NONE',  ( 128.0094361930251523, -4.111821299675517238, -15.64381207447768851 ) ) ;
#26913 = CARTESIAN_POINT ( 'NONE',  ( 119.4900081442453086, -1.834011780172310813, -8.268836392978581529 ) ) ;
#26914 = ORIENTED_EDGE ( 'NONE', *, *, #24189, .T. ) ;
#26915 = CARTESIAN_POINT ( 'NONE',  ( 125.1059481442452750, -8.166667518702819706, -8.995218007635861213 ) ) ;
#26916 = FACE_OUTER_BOUND ( 'NONE', #736, .T. ) ;
#26917 = CARTESIAN_POINT ( 'NONE',  ( 114.6682414775786469, -7.894159318335828068, -9.358103419637847864 ) ) ;
#26918 = CARTESIAN_POINT ( 'NONE',  ( 124.0980514478796408, -9.877548923986811502, -16.68609415519377137 ) ) ;
#26919 = CARTESIAN_POINT ( 'NONE',  ( 121.7023481442452777, -9.261995988541697145, -16.69588392320189030 ) ) ;
#26920 = CARTESIAN_POINT ( 'NONE',  ( 106.1764733795248219, -8.938348069036489818, -17.46756447353520159 ) ) ;
#26921 = CARTESIAN_POINT ( 'NONE',  ( 128.2184548109119930, -4.863998795839242995, -13.39321520033831447 ) ) ;
#26922 = ORIENTED_EDGE ( 'NONE', *, *, #44897, .T. ) ;
#26923 = DIRECTION ( 'NONE',  ( -1.000000000000000000, 0.000000000000000000, -0.000000000000000000 ) ) ;
#26924 = CARTESIAN_POINT ( 'NONE',  ( 123.9714148109119805, -8.899110576539710493, -16.42337572283490132 ) ) ;
#26925 = CARTESIAN_POINT ( 'NONE',  ( 120.5110881442453206, -6.344957434206665248, -7.627207830600338134 ) ) ;
#26926 = CARTESIAN_POINT ( 'NONE',  ( 113.1933481442453058, -5.574606645277164318, -18.38911715685844683 ) ) ;
#26927 = CARTESIAN_POINT ( 'NONE',  ( 115.9162281442453235, -4.089484607189486809, -7.948022111789456723 ) ) ;
#26928 = CARTESIAN_POINT ( 'NONE',  ( 94.99177781699742695, -29.35906829345538682, -14.78314672035751443 ) ) ;
#26929 = FACE_OUTER_BOUND ( 'NONE', #22184, .T. ) ;
#26930 = CARTESIAN_POINT ( 'NONE',  ( 120.1707281442453166, -9.565557343593413364, -10.61323700422348004 ) ) ;
#26931 = EDGE_LOOP ( 'NONE', ( #4834, #28086, #21295, #25986 ) ) ;
#26932 = CARTESIAN_POINT ( 'NONE',  ( 119.9438214775786520, -7.893985811506198047, -18.51759400769803676 ) ) ;
#26933 = AXIS2_PLACEMENT_3D ( 'NONE', #35664, #8091, #39095 ) ;
#26934 = CARTESIAN_POINT ( 'NONE',  ( 67.84197459855160162, -51.79774043821656448, -34.65109778699235221 ) ) ;
#26935 = CARTESIAN_POINT ( 'NONE',  ( 121.2485348109119769, -8.899110576539710493, -16.42337572283490132 ) ) ;
#26936 = VERTEX_POINT ( 'NONE', #32140 ) ;
#26937 = CARTESIAN_POINT ( 'NONE',  ( 122.7299391859119737, -1.406689858478933353, -17.56299727309130887 ) ) ;
#26938 = CARTESIAN_POINT ( 'NONE',  ( 120.1707281442453166, 0.2603800115204892296, -16.42320221600525088 ) ) ;
#26939 = CARTESIAN_POINT ( 'NONE',  ( 111.5938171295247940, -10.62599879583958540, -13.39321520033831447 ) ) ;
#26940 = CARTESIAN_POINT ( 'NONE',  ( 116.1431348109119881, 0.1319031606808879209, -14.10382304977623669 ) ) ;
#26941 = VERTEX_POINT ( 'NONE', #42422 ) ;
#26942 = ORIENTED_EDGE ( 'NONE', *, *, #33669, .F. ) ;
#26943 = VECTOR ( 'NONE', #44966, 1000.000000000000114 ) ;
#26944 = CARTESIAN_POINT ( 'NONE',  ( 112.1722681442453222, -0.4660016031367893996, -10.09054647747474043 ) ) ;
#26945 = CARTESIAN_POINT ( 'NONE',  ( 119.2631014775786298, -9.565557343593413364, -10.61323700422348004 ) ) ;
#26946 = AXIS2_PLACEMENT_3D ( 'NONE', #4948, #1526, #14997 ) ;
#26947 = B_SPLINE_CURVE_WITH_KNOTS ( 'NONE', 3,
 ( #5488, #40390, #5270, #43358, #36719, #2071, #15994, #29899 ),
 .UNSPECIFIED., .F., .F.,
 ( 4, 2, 2, 4 ),
 ( 0.000000000000000000, 0.2499999999999995559, 0.4999999999999991118, 1.000000000000000000 ),
 .UNSPECIFIED. ) ;
#26948 = PRESENTATION_STYLE_ASSIGNMENT (( #6875 ) ) ;
#26949 = LINE ( 'NONE', #33537, #18495 ) ;
#26950 = CARTESIAN_POINT ( 'NONE',  ( 117.2209414775786485, -7.893985811506177619, -18.51759400769804742 ) ) ;
#26951 = CARTESIAN_POINT ( 'NONE',  ( 107.0099108795247815, -8.938348069036489818, -9.318865927141430916 ) ) ;
#26952 = CARTESIAN_POINT ( 'NONE',  ( 118.8092881442453290, -9.988377603198976828, -10.36322818467138340 ) ) ;
#26954 = CARTESIAN_POINT ( 'NONE',  ( 119.2063748109119814, -7.894159318335828068, -9.358103419637847864 ) ) ;
#26953 = CARTESIAN_POINT ( 'NONE',  ( 117.7882081442453170, -6.344957434206665248, -7.627207830600338134 ) ) ;
#26955 = CARTESIAN_POINT ( 'NONE',  ( 123.4041481442452834, 0.1319031606808879209, -14.10382304977623669 ) ) ;
#26956 = CARTESIAN_POINT ( 'NONE',  ( 112.0020881442453344, 0.2603800115204892296, -16.42320221600525088 ) ) ;
#26957 = EDGE_CURVE ( 'NONE', #33070, #39008, #1127, .T. ) ;
#26958 = ORIENTED_EDGE ( 'NONE', *, *, #6666, .T. ) ;
#26959 = CARTESIAN_POINT ( 'NONE',  ( 123.5743281442453139, -2.084020599724406786, -8.691656652584148546 ) ) ;
#26960 = DIRECTION ( 'NONE',  ( -1.237391069487127839E-47, -1.069961080215129965E-32, 1.000000000000000000 ) ) ;
#26961 = DIRECTION ( 'NONE',  ( 0.000000000000000000, 0.000000000000000000, 1.000000000000000000 ) ) ;
#26962 = CARTESIAN_POINT ( 'NONE',  ( 107.2877233795247776, -8.938348069036489818, -17.46756447353520159 ) ) ;
#26963 = CARTESIAN_POINT ( 'NONE',  ( 113.5385046295247804, -4.863998795839590272, -18.39754474579285315 ) ) ;
#26964 = CARTESIAN_POINT ( 'NONE',  ( 107.0793640045248196, -10.62599879583958717, -11.00651665394454604 ) ) ;
#26965 = AXIS2_PLACEMENT_3D ( 'NONE', #28756, #18934, #25556 ) ;
#26966 = CARTESIAN_POINT ( 'NONE',  ( 121.3619881442452879, -4.089484607189486809, -7.948022111789456723 ) ) ;
#26967 = CARTESIAN_POINT ( 'NONE',  ( 121.4754414775786131, -1.833838273342659697, -17.42832698103878286 ) ) ;
#26968 = ORIENTED_EDGE ( 'NONE', *, *, #18240, .F. ) ;
#26969 = CARTESIAN_POINT ( 'NONE',  ( 125.3895814775786448, -7.893985811506177619, -18.51759400769804742 ) ) ;
#26970 = CARTESIAN_POINT ( 'NONE',  ( 113.0798948109119948, -8.899110576539710493, -16.42337572283490132 ) ) ;
#26971 = CARTESIAN_POINT ( 'NONE',  ( 121.5888948109119809, 0.1319031606808809820, -14.10382304977626156 ) ) ;
#26972 = CARTESIAN_POINT ( 'NONE',  ( 120.9081748109119872, -5.638512984488999180, -18.83840828888717311 ) ) ;
#26973 =( BOUNDED_CURVE ( )  B_SPLINE_CURVE ( 3, ( #27141, #20747, #37149, #10051 ),
 .UNSPECIFIED., .F., .F. ) 
 B_SPLINE_CURVE_WITH_KNOTS ( ( 4, 4 ),
 ( 3.141592653589795336, 4.712388980384689674 ),
 .UNSPECIFIED. ) 
 CURVE ( )  GEOMETRIC_REPRESENTATION_ITEM ( )  RATIONAL_B_SPLINE_CURVE ( ( 1.000000000000000000, 0.8047378541243659367, 0.8047378541243659367, 1.000000000000000000 ) ) 
 REPRESENTATION_ITEM ( '' )  );
#26974 = CARTESIAN_POINT ( 'NONE',  ( 120.0005481442453146, -5.638512984488999180, -18.83840828888717311 ) ) ;
#26975 = CARTESIAN_POINT ( 'NONE',  ( 123.4848705389825199, -6.126425863531494542, -18.50366489541501380 ) ) ;
#26976 = CARTESIAN_POINT ( 'NONE',  ( 125.2194014775786286, 0.1319031606808879209, -14.10382304977623669 ) ) ;
#26977 = CARTESIAN_POINT ( 'NONE',  ( 69.36136150295220659, -59.25864353191045808, -33.80145235246007474 ) ) ;
#26978 = FACE_OUTER_BOUND ( 'NONE', #19473, .T. ) ;
#26979 = ORIENTED_EDGE ( 'NONE', *, *, #43722, .F. ) ;
#26980 = DIRECTION ( 'NONE',  ( 0.000000000000000000, -0.3818493186865927203, 0.9242245927363029745 ) ) ;
#26981 = AXIS2_PLACEMENT_3D ( 'NONE', #7792, #29211, #37101 ) ;
#26982 = CARTESIAN_POINT ( 'NONE',  ( 90.15753105894957287, -11.66076665495339348, -14.14321520033831625 ) ) ;
#26983 = CARTESIAN_POINT ( 'NONE',  ( 122.8368814775786291, -7.894159318335828068, -9.358103419637847864 ) ) ;
#26984 = CARTESIAN_POINT ( 'NONE',  ( 106.4542858795248179, -8.402594152722688392, -9.854619843455216355 ) ) ;
#26985 = CARTESIAN_POINT ( 'NONE',  ( 113.1912390045248031, -9.868328341294098749, -11.32035403202665869 ) ) ;
#26986 = AXIS2_PLACEMENT_3D ( 'NONE', #7094, #31040, #6878 ) ;
#26987 = CARTESIAN_POINT ( 'NONE',  ( 118.0718414775786442, -0.8288870151387760510, -10.36305467784173118 ) ) ;
#26988 = CARTESIAN_POINT ( 'NONE',  ( 114.7816948109119863, -9.859900752359374465, -12.68260735090039404 ) ) ;
#26989 = CARTESIAN_POINT ( 'NONE',  ( 123.8012348109119642, 0.2603800115204892296, -16.42320221600525088 ) ) ;
#26990 = ORIENTED_EDGE ( 'NONE', *, *, #14827, .T. ) ;
#26991 = EDGE_CURVE ( 'NONE', #37423, #15070, #907, .T. ) ;
#26992 = CARTESIAN_POINT ( 'NONE',  ( 123.6310548109119765, -4.153390946401325223, -8.397313243818185668 ) ) ;
#26993 = CARTESIAN_POINT ( 'NONE',  ( 119.7169148109119874, -9.988377603198976828, -10.36322818467138340 ) ) ;
#26994 = CARTESIAN_POINT ( 'NONE',  ( 123.7445081442452874, -1.561330072975668948, -17.79121239304076951 ) ) ;
#26995 = CARTESIAN_POINT ( 'NONE',  ( 124.0848681442452772, -5.574606645277164318, -18.38911715685844683 ) ) ;
#26996 = ORIENTED_EDGE ( 'NONE', *, *, #25431, .T. ) ;
#26997 = CYLINDRICAL_SURFACE ( 'NONE', #6305, 3.000000000000001776 ) ;
#26998 = EDGE_CURVE ( 'NONE', #27773, #4363, #27676, .T. ) ;
#26999 = EDGE_CURVE ( 'NONE', #39653, #32876, #25583, .T. ) ;
#27000 = CARTESIAN_POINT ( 'NONE',  ( 125.5030348109119558, -3.383040157471821630, -19.15922257007629170 ) ) ;
#27001 = AXIS2_PLACEMENT_3D ( 'NONE', #42271, #14904, #32440 ) ;
#27002 = CARTESIAN_POINT ( 'NONE',  ( 116.1998614775786507, 0.4262465694468514643, -12.03445270309931736 ) ) ;
#27003 = CARTESIAN_POINT ( 'NONE',  ( 124.8223148109119762, 0.9020085738987339008, -11.91225656197089222 ) ) ;
#27004 = DIRECTION ( 'NONE',  ( -0.000000000000000000, -0.9284778069183718952, -0.3713878862591649677 ) ) ;
#27005 = CARTESIAN_POINT ( 'NONE',  ( 122.1048610609119720, -6.340755971794695078, -8.611740276972781771 ) ) ;
#27006 = VERTEX_POINT ( 'NONE', #4775 ) ;
#27007 = EDGE_CURVE ( 'NONE', #30187, #22775, #23299, .T. ) ;
#27008 = DIRECTION ( 'NONE',  ( -0.000000000000000000, -0.9284778069183721172, -0.3713878862591650232 ) ) ;
#27009 = CARTESIAN_POINT ( 'NONE',  ( 111.1076452545248259, -9.868328341294098749, -15.46607636864997204 ) ) ;
#27010 = TOROIDAL_SURFACE ( 'NONE', #26258, 26.50000000000000000, 1.500000000000000000 ) ;
#27011 = CARTESIAN_POINT ( 'NONE',  ( 64.24243542014160369, -41.01918285936451269, -10.89321520033831447 ) ) ;
#27012 = VECTOR ( 'NONE', #36470, 1000.000000000000000 ) ;
#27013 = ADVANCED_FACE ( 'NONE', ( #28738 ), #16863, .T. ) ;
#27014 = CARTESIAN_POINT ( 'NONE',  ( 120.3409081442453044, -8.899110576539710493, -16.42337572283490132 ) ) ;
#27015 = CARTESIAN_POINT ( 'NONE',  ( 112.6828081442453282, -2.084020599724406786, -8.691656652584148546 ) ) ;
#27016 = CARTESIAN_POINT ( 'NONE',  ( 126.3618269276777255, -6.022947313180186946, -18.33077713658678221 ) ) ;
#27017 = EDGE_CURVE ( 'NONE', #22843, #42191, #7989, .T. ) ;
#27018 = EDGE_CURVE ( 'NONE', #35636, #25810, #23989, .T. ) ;
#27019 = ORIENTED_EDGE ( 'NONE', *, *, #11844, .T. ) ;
#27020 = CARTESIAN_POINT ( 'NONE',  ( 126.2184548109119788, -2.495269033102075262, -17.79652296963211455 ) ) ;
#27021 = CARTESIAN_POINT ( 'NONE',  ( 118.8660148109119774, 0.1319031606808879209, -14.10382304977623669 ) ) ;
#27022 = CARTESIAN_POINT ( 'NONE',  ( 113.7038881442453402, -6.222761293078241884, -8.102969835052219238 ) ) ;
#27023 = DIRECTION ( 'NONE',  ( -0.9908103287288505534, 0.1352586133457945317, 0.000000000000000000 ) ) ;
#27024 = CARTESIAN_POINT ( 'NONE',  ( 111.3213681442453264, -7.643976991954077427, -18.09477374809248928 ) ) ;
#27026 = CARTESIAN_POINT ( 'NONE',  ( 124.0848681442452772, -4.089484607189486809, -7.948022111789456723 ) ) ;
#27025 = CARTESIAN_POINT ( 'NONE',  ( 70.91713523389951490, -26.53035501928088635, -5.366017652747787636 ) ) ;
#27027 = CARTESIAN_POINT ( 'NONE',  ( 113.0798948109119948, -0.4660016031367893996, -10.09054647747474043 ) ) ;
#27028 = ORIENTED_EDGE ( 'NONE', *, *, #9456, .F. ) ;
#27029 = CARTESIAN_POINT ( 'NONE',  ( 114.6682414775786469, -1.561330072975668060, -17.79121239304076596 ) ) ;
#27030 = CARTESIAN_POINT ( 'NONE',  ( 84.49707967414211396, -25.23119213852205789, -15.24166438581092109 ) ) ;
#27031 = CARTESIAN_POINT ( 'NONE',  ( 114.3024890045248156, 0.8980012041604421569, -15.77991374673208469 ) ) ;
#27032 = CARTESIAN_POINT ( 'NONE',  ( 126.0135748109119902, -1.833838273342660141, -17.42832698103878286 ) ) ;
#27033 = CARTESIAN_POINT ( 'NONE',  ( 119.8303681442453126, 0.4262465694468514643, -12.03445270309931736 ) ) ;
#27034 = DIRECTION ( 'NONE',  ( -0.000000000000000000, -0.9284778069183718952, -0.3713878862591649677 ) ) ;
#27035 = CARTESIAN_POINT ( 'NONE',  ( 113.0523327545247838, -6.936859964151250502, -8.388885654883777576 ) ) ;
#27036 = DIRECTION ( 'NONE',  ( -0.8636456077245080465, 0.5040994586965603652, 0.000000000000000000 ) ) ;
#27037 = CARTESIAN_POINT ( 'NONE',  ( 115.9947331777918862, -0.01829820670803256055, -14.64321520033831447 ) ) ;
#27038 = CARTESIAN_POINT ( 'NONE',  ( 113.3068014775786594, -1.833838273342658809, -17.42832698103878286 ) ) ;
#27039 = CARTESIAN_POINT ( 'NONE',  ( 112.8439733795247832, -8.938348069036489818, -17.46756447353520159 ) ) ;
#27040 = DIRECTION ( 'NONE',  ( 0.7202110682883375858, 0.2576522076061144029, -0.6441361323747234469 ) ) ;
#27041 = CARTESIAN_POINT ( 'NONE',  ( 115.0664733795247798, -8.938348069036489818, -17.46756447353520159 ) ) ;
#27042 = CARTESIAN_POINT ( 'NONE',  ( 123.8012348109119642, 0.2603800115204892296, -16.42320221600525088 ) ) ;
#27043 = CARTESIAN_POINT ( 'NONE',  ( 120.3976348109119812, -1.834011780172310813, -8.268836392978581529 ) ) ;
#27044 = CARTESIAN_POINT ( 'NONE',  ( 114.9970202545248554, -10.62599879583958540, -15.77991374673209179 ) ) ;
#27045 = CARTESIAN_POINT ( 'NONE',  ( 119.2631014775786298, 0.2603800115204892296, -16.42320221600525088 ) ) ;
#27046 = CARTESIAN_POINT ( 'NONE',  ( 113.5337081442453240, -9.261995988541697145, -16.69588392320189030 ) ) ;
#27047 = ORIENTED_EDGE ( 'NONE', *, *, #790, .T. ) ;
#27048 = CARTESIAN_POINT ( 'NONE',  ( 112.8529881442453302, -7.894159318335828068, -9.358103419637847864 ) ) ;
#27049 = CARTESIAN_POINT ( 'NONE',  ( 124.5954081442453116, -3.383040157471821630, -19.15922257007629170 ) ) ;
#27050 = CONICAL_SURFACE ( 'NONE', #9563, 2.000000000000000444, 0.9599310885968830309 ) ;
#27051 = CARTESIAN_POINT ( 'NONE',  ( 125.3895814775786448, -7.893985811506177619, -18.51759400769804742 ) ) ;
#27052 = CARTESIAN_POINT ( 'NONE',  ( 112.5693548109119888, -10.63000616557722466, -14.87417383870573495 ) ) ;
#27053 = CARTESIAN_POINT ( 'NONE',  ( 111.8319081442453182, -4.153390946401321671, -8.397313243818183892 ) ) ;
#27054 = ORIENTED_EDGE ( 'NONE', *, *, #22576, .F. ) ;
#27055 = CARTESIAN_POINT ( 'NONE',  ( 117.2776681442452968, -4.153390946401325223, -8.397313243818185668 ) ) ;
#27056 = CARTESIAN_POINT ( 'NONE',  ( 112.9664414775786412, 0.5811942927096154232, -14.16772938898807155 ) ) ;
#27057 = CARTESIAN_POINT ( 'NONE',  ( 110.8992858795247827, -8.402594152722688392, -9.854619843455216355 ) ) ;
#27058 = CARTESIAN_POINT ( 'NONE',  ( 124.2550481442452792, -0.1624402480850797581, -16.17319339645315424 ) ) ;
#27059 = CARTESIAN_POINT ( 'NONE',  ( 94.20708369096698220, -25.99489077589524300, -13.39321520033831447 ) ) ;
#27060 = CARTESIAN_POINT ( 'NONE',  ( 112.0105358795247810, -0.7896495226426338832, -17.46756447353520159 ) ) ;
#27061 = VERTEX_POINT ( 'NONE', #41100 ) ;
#27062 = CARTESIAN_POINT ( 'NONE',  ( 114.4917429525735741, -1.111561923218669534, -17.14115599315433869 ) ) ;
#27063 = CARTESIAN_POINT ( 'NONE',  ( 113.1259820646196914, 0.6269505268395592079, -14.64321520033833579 ) ) ;
#27064 = EDGE_CURVE ( 'NONE', #25805, #3754, #41544, .T. ) ;
#27065 = CARTESIAN_POINT ( 'NONE',  ( 113.3301452545248083, -9.868328341294102302, -15.46607636865002355 ) ) ;
#27066 = CIRCLE ( 'NONE', #35767, 5.999999999999998224 ) ;
#27067 =( NAMED_UNIT ( * ) PLANE_ANGLE_UNIT ( ) SI_UNIT ( $, .RADIAN. ) );
#27068 = CARTESIAN_POINT ( 'NONE',  ( 116.3808264296373807, 2.254317590850374309, -6.449063452130288532 ) ) ;
#27069 = DIRECTION ( 'NONE',  ( 1.000000000000000000, 0.000000000000000000, -0.000000000000000000 ) ) ;
#27070 = CARTESIAN_POINT ( 'NONE',  ( 108.7462390045248242, -9.868328341294098749, -11.32035403202665869 ) ) ;
#27071 = CARTESIAN_POINT ( 'NONE',  ( 121.9470836909669913, -25.99489077589524300, -13.39321520033831447 ) ) ;
#27072 = CARTESIAN_POINT ( 'NONE',  ( 119.3198281442452924, 0.5811942927096110934, -14.16772938898807510 ) ) ;
#27073 = CARTESIAN_POINT ( 'NONE',  ( 136.9082792203374197, -4.441316609263642690, -18.90303633254767846 ) ) ;
#27074 = AXIS2_PLACEMENT_3D ( 'NONE', #41789, #6896, #4356 ) ;
#27075 = CARTESIAN_POINT ( 'NONE',  ( 116.0829010812576882, -0.01829820670803256055, -12.14321520033834290 ) ) ;
#27076 = CARTESIAN_POINT ( 'NONE',  ( 123.9106423109119817, -0.4387604401699203294, -15.73000352943926927 ) ) ;
#27077 = CARTESIAN_POINT ( 'NONE',  ( 122.4397948109119767, -0.1624402480850797581, -16.17319339645315424 ) ) ;
#27078 = CARTESIAN_POINT ( 'NONE',  ( 125.3328548109119964, -0.8288870151387760510, -10.36305467784173118 ) ) ;
#27079 = ORIENTED_EDGE ( 'NONE', *, *, #12343, .F. ) ;
#27080 = CARTESIAN_POINT ( 'NONE',  ( 122.7234281442452755, -5.638512984488999180, -18.83840828888717311 ) ) ;
#27081 = ADVANCED_FACE ( 'NONE', ( #3449 ), #26, .T. ) ;
#27082 = CARTESIAN_POINT ( 'NONE',  ( 118.2420214775786320, -3.383040157471821630, -19.15922257007629170 ) ) ;
#27083 = CARTESIAN_POINT ( 'NONE',  ( 125.8433948109119456, -1.834011780172310813, -8.268836392978581529 ) ) ;
#27084 = CARTESIAN_POINT ( 'NONE',  ( 113.4769814775786330, 0.4262465694468514643, -12.03445270309931736 ) ) ;
#27085 = CARTESIAN_POINT ( 'NONE',  ( 125.5597614775786326, -1.561330072975669392, -17.79121239304076951 ) ) ;
#27086 = CARTESIAN_POINT ( 'NONE',  ( 110.3436608795247764, -8.938348069036489818, -9.318865927141430916 ) ) ;
#27087 = CARTESIAN_POINT ( 'NONE',  ( 106.0375671295248310, 0.1403307496149613920, -13.39321520033831447 ) ) ;
#27088 = CARTESIAN_POINT ( 'NONE',  ( 83.37840489759373952, -32.03678395546867819, -23.58446301471671802 ) ) ;
#27089 = CARTESIAN_POINT ( 'NONE',  ( 115.9162281442453235, -5.574606645277164318, -18.38911715685844683 ) ) ;
#27090 = CARTESIAN_POINT ( 'NONE',  ( 118.4122014775786340, -9.859900752359374465, -12.68260735090039404 ) ) ;
#27091 = DIRECTION ( 'NONE',  ( -1.000000000000000000, 0.000000000000000000, 0.000000000000000000 ) ) ;
#27092 = CARTESIAN_POINT ( 'NONE',  ( 114.4413952545248350, -9.868328341294098749, -15.46607636864997204 ) ) ;
#27093 = ORIENTED_EDGE ( 'NONE', *, *, #29098, .T. ) ;
#27094 = CARTESIAN_POINT ( 'NONE',  ( 61.27778620743471549, -25.99489077589588604, -15.39321520033831625 ) ) ;
#27095 = CARTESIAN_POINT ( 'NONE',  ( 112.4559014775786494, -9.988377603198976828, -10.36322818467138340 ) ) ;
#27096 = DIRECTION ( 'NONE',  ( 0.000000000000000000, -0.3818493186865927203, 0.9242245927363029745 ) ) ;
#27097 = CARTESIAN_POINT ( 'NONE',  ( 123.0077516859119839, -0.6942167230862511529, -9.935906262978006609 ) ) ;
#27098 = CARTESIAN_POINT ( 'NONE',  ( 119.7434548109119703, -2.527210466738041728, -8.967976844669124148 ) ) ;
#27099 = ORIENTED_EDGE ( 'NONE', *, *, #10044, .T. ) ;
#27100 = CARTESIAN_POINT ( 'NONE',  ( 114.0941296295247867, -4.863998795839590272, -19.15521520033831493 ) ) ;
#27101 = DIRECTION ( 'NONE',  ( 0.7871354856660198740, 0.4483307682966886643, 0.4235767337848242442 ) ) ;
#27102 = ORIENTED_EDGE ( 'NONE', *, *, #39833, .F. ) ;
#27103 = CARTESIAN_POINT ( 'NONE',  ( 117.9583881442453048, -10.30919188438810075, -12.61870101168855918 ) ) ;
#27104 = AXIS2_PLACEMENT_3D ( 'NONE', #17352, #35088, #34861 ) ;
#27105 = CARTESIAN_POINT ( 'NONE',  ( 111.9453614775786434, -1.561330072975668060, -17.79121239304076596 ) ) ;
#27106 = CARTESIAN_POINT ( 'NONE',  ( 116.5969481442453031, -9.859900752359374465, -12.68260735090039404 ) ) ;
#27107 = CARTESIAN_POINT ( 'NONE',  ( 120.2526890279447116, -8.246306354371270686, -17.07862329173823568 ) ) ;
#27108 = CARTESIAN_POINT ( 'NONE',  ( 122.2128881442453263, -1.834011780172310813, -8.268836392978581529 ) ) ;
#27109 = CARTESIAN_POINT ( 'NONE',  ( 117.1642148109119859, -9.261995988541697145, -16.69588392320189030 ) ) ;
#27110 = CARTESIAN_POINT ( 'NONE',  ( 109.3018640045248304, 0.1403307496149616695, -15.46607636864997204 ) ) ;
#27111 = CARTESIAN_POINT ( 'NONE',  ( 114.2144281442453178, -1.833838273342658809, -17.42832698103878286 ) ) ;
#27112 = ORIENTED_EDGE ( 'NONE', *, *, #33087, .T. ) ;
#27113 = CARTESIAN_POINT ( 'NONE',  ( 117.1642148109119859, -9.261995988541697145, -16.69588392320189030 ) ) ;
#27114 = ADVANCED_FACE ( 'NONE', ( #15275 ), #22121, .T. ) ;
#27115 = DIRECTION ( 'NONE',  ( 1.000000000000000000, 0.000000000000000000, -0.000000000000000000 ) ) ;
#27116 = CARTESIAN_POINT ( 'NONE',  ( 115.9162281442453235, -4.089484607189486809, -7.948022111789456723 ) ) ;
#27117 = EDGE_LOOP ( 'NONE', ( #6299, #33663, #3424, #17849 ) ) ;
#27118 = CARTESIAN_POINT ( 'NONE',  ( 120.5678148109119832, -8.166667518702819706, -8.995218007635861213 ) ) ;
#27119 = DIRECTION ( 'NONE',  ( 1.000000000000000000, 0.000000000000000000, -0.000000000000000000 ) ) ;
#27120 = CARTESIAN_POINT ( 'NONE',  ( 113.0231681442453180, -10.15424416112533912, -14.75197769757731336 ) ) ;
#27121 = LINE ( 'NONE', #33944, #23675 ) ;
#27122 = CARTESIAN_POINT ( 'NONE',  ( 117.9583881442453048, 0.1319031606808879209, -14.10382304977623669 ) ) ;
#27123 = CARTESIAN_POINT ( 'NONE',  ( 123.4754274106697522, -4.049225749020625820, -15.72719735404760577 ) ) ;
#27124 = AXIS2_PLACEMENT_3D ( 'NONE', #38340, #24449, #38128 ) ;
#27125 = CARTESIAN_POINT ( 'NONE',  ( 118.6958348109119754, -3.505236298600246325, -18.68346056562440793 ) ) ;
#27126 = EDGE_CURVE ( 'NONE', #13419, #31913, #18251, .T. ) ;
#27127 = DIRECTION ( 'NONE',  ( -0.2768435750659241079, -0.3568721902840695792, 0.8921882507333129819 ) ) ;
#27128 = CARTESIAN_POINT ( 'NONE',  ( 115.4056881442453459, -2.084020599724406786, -8.691656652584148546 ) ) ;
#27129 = CARTESIAN_POINT ( 'NONE',  ( 115.6325948109119821, 0.2603800115204892296, -16.42320221600525088 ) ) ;
#27130 = CARTESIAN_POINT ( 'NONE',  ( 121.3408766859119794, -9.033780868592240054, -16.85052413769862056 ) ) ;
#27131 = CARTESIAN_POINT ( 'NONE',  ( 126.4106614775786284, -6.222761293078241884, -8.102969835052219238 ) ) ;
#27132 = CARTESIAN_POINT ( 'NONE',  ( 115.6893214775786447, -9.859900752359374465, -12.68260735090039404 ) ) ;
#27133 = CARTESIAN_POINT ( 'NONE',  ( 121.7590748109119687, -7.893985811506177619, -18.51759400769804742 ) ) ;
#27134 = COLOUR_RGB ( '',0.7921568627450980005, 0.8196078431372548767, 0.9333333333333333481 ) ;
#27135 = CARTESIAN_POINT ( 'NONE',  ( 116.5402214775786405, -9.565557343593413364, -10.61323700422348004 ) ) ;
#27136 = VERTEX_POINT ( 'NONE', #28745 ) ;
#27137 = CARTESIAN_POINT ( 'NONE',  ( 114.1009748109119784, -4.089484607189486809, -7.948022111789456723 ) ) ;
#27138 = CARTESIAN_POINT ( 'NONE',  ( 107.9822546295247889, -4.863998795839590272, -7.631215200338315796 ) ) ;
#27139 = CARTESIAN_POINT ( 'NONE',  ( 106.9404577545248145, -2.791137627527939813, -18.39754474579286025 ) ) ;
#27140 = CIRCLE ( 'NONE', #3113, 15.89999999999999680 ) ;
#27141 = CARTESIAN_POINT ( 'NONE',  ( 87.44708369096657918, -21.99489077589588604, -7.893215200338315363 ) ) ;
#27142 = B_SPLINE_CURVE_WITH_KNOTS ( 'NONE', 3,
 ( #39546, #8307, #31455, #17561, #5766, #17128, #13704, #27611, #10068, #23969, #20764, #14137 ),
 .UNSPECIFIED., .F., .F.,
 ( 4, 2, 2, 2, 2, 4 ),
 ( 0.000000000000000000, 0.1126714536578860004, 0.2901371629263108098, 0.4676028721947325661, 0.6450685814631537118, 1.000000000000000000 ),
 .UNSPECIFIED. ) ;
#27143 = CARTESIAN_POINT ( 'NONE',  ( 109.6491296295247793, -4.863998795839590272, -19.15521520033831493 ) ) ;
#27144 = CARTESIAN_POINT ( 'NONE',  ( 118.1285681442453068, -7.893985811506177619, -18.51759400769804742 ) ) ;
#27145 = ORIENTED_EDGE ( 'NONE', *, *, #1583, .T. ) ;
#27146 = LINE ( 'NONE', #40836, #3411 ) ;
#27147 = CARTESIAN_POINT ( 'NONE',  ( 79.00611218289952831, -44.99489077589586827, -6.893215200338315363 ) ) ;
#27148 = CARTESIAN_POINT ( 'NONE',  ( 116.7104014775786425, -8.899110576539710493, -16.42337572283490132 ) ) ;
#27149 = CARTESIAN_POINT ( 'NONE',  ( 120.8933699480702586, -6.365377317481695663, -18.95617363400926081 ) ) ;
#27150 = CARTESIAN_POINT ( 'NONE',  ( 124.8790414775786246, -0.4660016031367893996, -10.09054647747474043 ) ) ;
#27151 = CARTESIAN_POINT ( 'NONE',  ( 105.6903015045248253, -2.477300249445798297, -7.631215200338321125 ) ) ;
#27152 = CARTESIAN_POINT ( 'NONE',  ( 89.29151511389673601, -9.887673028482419468, -13.35680558263691609 ) ) ;
#27153 = ORIENTED_EDGE ( 'NONE', *, *, #28781, .F. ) ;
#27154 = CARTESIAN_POINT ( 'NONE',  ( 112.8529881442453302, -1.561330072975668060, -17.79121239304076596 ) ) ;
#27155 = CARTESIAN_POINT ( 'NONE',  ( 123.5176014775786228, -0.8288870151387760510, -10.36305467784173118 ) ) ;
#27156 = CARTESIAN_POINT ( 'NONE',  ( 121.0783548109119749, 0.2603800115204892296, -16.42320221600525088 ) ) ;
#27157 = EDGE_CURVE ( 'NONE', #29699, #44941, #15385, .T. ) ;
#27158 = CARTESIAN_POINT ( 'NONE',  ( 112.7395348109119766, -4.153390946401321671, -8.397313243818183892 ) ) ;
#27159 = CARTESIAN_POINT ( 'NONE',  ( 118.5823814775786360, -1.834011780172310813, -8.268836392978581529 ) ) ;
#27160 = FACE_OUTER_BOUND ( 'NONE', #16720, .T. ) ;
#27161 = CARTESIAN_POINT ( 'NONE',  ( 114.4099712410415748, 0.7607806665037644134, -12.14321520033829316 ) ) ;
#27162 = CARTESIAN_POINT ( 'NONE',  ( 124.3117748109119844, 0.1319031606808879209, -14.10382304977623669 ) ) ;
#27163 = ORIENTED_EDGE ( 'NONE', *, *, #23174, .F. ) ;
#27164 = CIRCLE ( 'NONE', #14041, 1.500000000000000666 ) ;
#27165 = CARTESIAN_POINT ( 'NONE',  ( 123.8411891859119862, -8.844754642576884152, -8.592115655440050404 ) ) ;
#27166 = AXIS2_PLACEMENT_3D ( 'NONE', #44368, #34083, #2850 ) ;
#27167 = CARTESIAN_POINT ( 'NONE',  ( 115.8027748109119841, -0.4660016031367893996, -10.09054647747474043 ) ) ;
#27168 = CARTESIAN_POINT ( 'NONE',  ( 119.7169148109119874, -0.1624402480850797581, -16.17319339645315424 ) ) ;
#27169 = ORIENTED_EDGE ( 'NONE', *, *, #17038, .T. ) ;
#27170 = CARTESIAN_POINT ( 'NONE',  ( 122.5910329359119970, -5.367793381288652910, -18.78638297431638904 ) ) ;
#27171 = CARTESIAN_POINT ( 'NONE',  ( 60.02417077683579549, -12.62998352332487606, -9.398546866638605835 ) ) ;
#27172 = CARTESIAN_POINT ( 'NONE',  ( 118.8092881442453290, -9.988377603198976828, -10.36322818467138340 ) ) ;
#27173 = CARTESIAN_POINT ( 'NONE',  ( 112.2883483795247770, -0.7896495226426338832, -9.318865927141430916 ) ) ;
#27174 = CARTESIAN_POINT ( 'NONE',  ( 117.2209414775786485, -2.084020599724406786, -8.691656652584148546 ) ) ;
#27175 = ORIENTED_EDGE ( 'NONE', *, *, #914, .F. ) ;
#27176 = AXIS2_PLACEMENT_3D ( 'NONE', #43650, #26784, #9445 ) ;
#27177 = ORIENTED_EDGE ( 'NONE', *, *, #35587, .T. ) ;
#27178 = CARTESIAN_POINT ( 'NONE',  ( 125.8433948109119456, -7.643976991954077427, -18.09477374809248928 ) ) ;
#27179 = CARTESIAN_POINT ( 'NONE',  ( 70.89562859596755118, -66.92613143246303764, -42.60403544796190545 ) ) ;
#27180 = LINE ( 'NONE', #3450, #44078 ) ;
#27181 = DIRECTION ( 'NONE',  ( -0.000000000000000000, -0.9284778069183721172, -0.3713878862591650232 ) ) ;
#27182 = CARTESIAN_POINT ( 'NONE',  ( 122.1561614775786353, -0.4660016031367893996, -10.09054647747474043 ) ) ;
#27183 = CARTESIAN_POINT ( 'NONE',  ( 112.1722566881651915, -8.899626691430476910, -16.42270751673093798 ) ) ;
#27184 = EDGE_CURVE ( 'NONE', #42225, #11850, #29117, .T. ) ;
#27185 = CARTESIAN_POINT ( 'NONE',  ( 116.9163235773848726, -2.467220198592778413, -17.83387418641524391 ) ) ;
#27186 = CARTESIAN_POINT ( 'NONE',  ( 121.0783548109119749, 0.2603800115204892296, -16.42320221600525088 ) ) ;
#27188 = CARTESIAN_POINT ( 'NONE',  ( 118.0151148109119816, 0.4262465694468514643, -12.03445270309931736 ) ) ;
#27187 = CARTESIAN_POINT ( 'NONE',  ( 120.4543614775786295, -4.089484607189486809, -7.948022111789456723 ) ) ;
#27189 = CARTESIAN_POINT ( 'NONE',  ( 124.6521348109119884, -7.894159318335828068, -9.358103419637847864 ) ) ;
#27190 = CARTESIAN_POINT ( 'NONE',  ( 113.1933481442453058, -4.089484607189486809, -7.948022111789456723 ) ) ;
#27191 = ORIENTED_EDGE ( 'NONE', *, *, #23045, .F. ) ;
#27192 = CARTESIAN_POINT ( 'NONE',  ( 122.9503348109119827, -9.859900752359378018, -12.68260735090039759 ) ) ;
#27193 = CARTESIAN_POINT ( 'NONE',  ( 122.9042958072984959, 0.3208234527006196823, -15.99825685930876595 ) ) ;
#27194 = CONICAL_SURFACE ( 'NONE', #28624, 5.999999999999997335, 0.4636476090008060935 ) ;
#27195 = DIRECTION ( 'NONE',  ( -1.000000000000000000, 0.000000000000000000, 0.000000000000000000 ) ) ;
#27196 = CARTESIAN_POINT ( 'NONE',  ( 107.8433483795247838, -0.7896495226426338832, -9.318865927141430916 ) ) ;
#27197 = CIRCLE ( 'NONE', #30087, 2.000000000000000444 ) ;
#27198 = CARTESIAN_POINT ( 'NONE',  ( 114.1635827545248389, -6.936859964151250502, -8.388885654883777576 ) ) ;
#27199 = CARTESIAN_POINT ( 'NONE',  ( 105.5513952545248060, 0.8980012041604421569, -11.00651665394454071 ) ) ;
#27200 = CARTESIAN_POINT ( 'NONE',  ( 120.5110881442453206, -6.344957434206665248, -7.627207830600338134 ) ) ;
#27201 = CARTESIAN_POINT ( 'NONE',  ( 121.4187148109119789, -3.505236298600246325, -18.68346056562440793 ) ) ;
#27202 = VERTEX_POINT ( 'NONE', #32146 ) ;
#27203 = CARTESIAN_POINT ( 'NONE',  ( 125.5030348109119558, -3.383040157471821630, -19.15922257007629170 ) ) ;
#27204 = CARTESIAN_POINT ( 'NONE',  ( 112.2857214775786474, -5.574606645277164318, -18.38911715685844683 ) ) ;
#27205 = CARTESIAN_POINT ( 'NONE',  ( 66.58723489636778936, -20.14619392353143112, -10.89321520033831447 ) ) ;
#27206 = CARTESIAN_POINT ( 'NONE',  ( 121.8158014775786171, -5.638512984488999180, -18.83840828888717311 ) ) ;
#27207 = CARTESIAN_POINT ( 'NONE',  ( 120.6812681442452941, -10.30919188438810075, -12.61870101168855918 ) ) ;
#27208 = CARTESIAN_POINT ( 'NONE',  ( 74.64594387179452895, -42.43939829949535181, -10.39321520033831625 ) ) ;
#27209 = CARTESIAN_POINT ( 'NONE',  ( 112.6260814775786514, -9.261995988541697145, -16.69588392320189030 ) ) ;
#27210 = DIRECTION ( 'NONE',  ( -0.000000000000000000, -0.9284778069183721172, -0.3713878862591650232 ) ) ;
#27211 = CARTESIAN_POINT ( 'NONE',  ( 115.6220983795247861, -8.402594152722688392, -16.93181055722141792 ) ) ;
#27212 = VERTEX_POINT ( 'NONE', #7530 ) ;
#27213 = VECTOR ( 'NONE', #43538, 1000.000000000000000 ) ;
#27214 = CARTESIAN_POINT ( 'NONE',  ( 42.36021970110777346, -12.73296999994090584, -8.893215200338314474 ) ) ;
#27215 = CARTESIAN_POINT ( 'NONE',  ( 113.0798948109119948, -8.899110576539710493, -16.42337572283490132 ) ) ;
#27216 = CARTESIAN_POINT ( 'NONE',  ( 123.1772414775786189, -5.574606645277164318, -18.38911715685844683 ) ) ;
#27217 = CARTESIAN_POINT ( 'NONE',  ( 106.8015515045248378, -6.936859964151250502, -18.39754474579286025 ) ) ;
#27218 = CARTESIAN_POINT ( 'NONE',  ( 110.9687390045248350, -9.868328341294098749, -11.32035403202665869 ) ) ;
#27219 = CARTESIAN_POINT ( 'NONE',  ( 121.3619881442452879, -5.574606645277164318, -18.38911715685844683 ) ) ;
#27220 =( NAMED_UNIT ( * ) SI_UNIT ( $, .STERADIAN. ) SOLID_ANGLE_UNIT ( ) );
#27221 = CARTESIAN_POINT ( 'NONE',  ( 116.3700414775786527, -4.153390946401321671, -8.397313243818183892 ) ) ;
#27222 = CARTESIAN_POINT ( 'NONE',  ( 124.8790414775786246, -0.4660016031367893996, -10.09054647747474043 ) ) ;
#27223 = ORIENTED_EDGE ( 'NONE', *, *, #27392, .F. ) ;
#27224 = CARTESIAN_POINT ( 'NONE',  ( 122.8936081442453059, -9.565557343593413364, -10.61323700422348004 ) ) ;
#27225 = CARTESIAN_POINT ( 'NONE',  ( 117.1074881442453233, -10.63000616557722466, -14.87417383870573495 ) ) ;
#27226 = CARTESIAN_POINT ( 'NONE',  ( 123.8012348109119642, 0.2603800115204892296, -16.42320221600525088 ) ) ;
#27227 = CARTESIAN_POINT ( 'NONE',  ( 124.3117748109119844, 0.1319031606808879209, -14.10382304977623669 ) ) ;
#27228 = ORIENTED_EDGE ( 'NONE', *, *, #35941, .F. ) ;
#27229 = CARTESIAN_POINT ( 'NONE',  ( 123.4268075888223848, -2.372251574601201174, -17.96033910819751611 ) ) ;
#27230 = EDGE_CURVE ( 'NONE', #1558, #44110, #4921, .T. ) ;
#27231 = VECTOR ( 'NONE', #31670, 1000.000000000000114 ) ;
#27232 = AXIS2_PLACEMENT_3D ( 'NONE', #13527, #41357, #31063 ) ;
#27233 = CARTESIAN_POINT ( 'NONE',  ( 125.5597614775786326, -1.561330072975669392, -17.79121239304076951 ) ) ;
#27234 = CARTESIAN_POINT ( 'NONE',  ( 114.4980614775786734, -2.084020599724406786, -8.691656652584148546 ) ) ;
#27235 = CARTESIAN_POINT ( 'NONE',  ( 125.5597614775786326, -1.561330072975669392, -17.79121239304076951 ) ) ;
#27236 = CARTESIAN_POINT ( 'NONE',  ( 114.8951481442453115, -0.4660016031367867906, -10.09054647747474398 ) ) ;
#27237 = CARTESIAN_POINT ( 'NONE',  ( 122.2437673109119629, -9.289237151508434209, -11.05642687123711276 ) ) ;
#27238 = EDGE_LOOP ( 'NONE', ( #28929, #16347, #9369, #5191, #38303 ) ) ;
#27239 = DIRECTION ( 'NONE',  ( 0.000000000000000000, 1.000000000000000000, 0.000000000000000000 ) ) ;
#27240 = CARTESIAN_POINT ( 'NONE',  ( 60.53937939559665438, -4.256997083809236138, -7.393215200338315363 ) ) ;
#27241 = CARTESIAN_POINT ( 'NONE',  ( 107.0099108795247815, -1.325403438956436419, -16.93181055722141792 ) ) ;
#27242 = CIRCLE ( 'NONE', #11938, 5.635000000000000675 ) ;
#27243 = CARTESIAN_POINT ( 'NONE',  ( 115.0664733795247798, -1.325403438956533675, -9.854619843455179051 ) ) ;
#27244 = CARTESIAN_POINT ( 'NONE',  ( 123.7445081442452874, -7.894159318335828068, -9.358103419637847864 ) ) ;
#27245 = CARTESIAN_POINT ( 'NONE',  ( 113.0231681442453180, -10.15424416112533912, -14.75197769757731336 ) ) ;
#27246 = CARTESIAN_POINT ( 'NONE',  ( 126.4852516627911427, -0.4199418574856381703, -10.82374662991991343 ) ) ;
#27247 = EDGE_LOOP ( 'NONE', ( #10977, #1153, #43977, #13953, #40900, #17178, #24258, #16850, #23122, #36330 ) ) ;
#27248 = DIRECTION ( 'NONE',  ( 0.000000000000000000, 0.9554676365605390131, 0.2950959089608289343 ) ) ;
#27249 = CARTESIAN_POINT ( 'NONE',  ( 112.9097148109120070, -9.565557343593413364, -10.61323700422348004 ) ) ;
#27250 = EDGE_CURVE ( 'NONE', #14709, #14403, #18022, .T. ) ;
#27251 = CARTESIAN_POINT ( 'NONE',  ( 112.1874712410415924, 0.7607806665037644134, -12.14321520033829493 ) ) ;
#27252 = CARTESIAN_POINT ( 'NONE',  ( 111.7857214775786474, -4.159894987975828684, -8.443039665293898821 ) ) ;
#27254 = CARTESIAN_POINT ( 'NONE',  ( 124.8790414775786246, -0.4660016031367893996, -10.09054647747474043 ) ) ;
#27253 = LINE ( 'NONE', #13349, #2527 ) ;
#27255 = CARTESIAN_POINT ( 'NONE',  ( 126.0703014775786102, -0.1624402480850797581, -16.17319339645315424 ) ) ;
#27256 = EDGE_LOOP ( 'NONE', ( #8155, #26380, #43443, #24421, #26044 ) ) ;
#27257 = CARTESIAN_POINT ( 'NONE',  ( 114.0442481442453300, -1.834011780172310813, -8.268836392978581529 ) ) ;
#27258 = CARTESIAN_POINT ( 'NONE',  ( 85.15861813568058380, -27.84333996136784961, -14.15691383771150136 ) ) ;
#27259 = CARTESIAN_POINT ( 'NONE',  ( 114.3719421295247827, 0.8980012041604618078, -13.39321520033831447 ) ) ;
#27260 = EDGE_CURVE ( 'NONE', #34483, #21278, #17804, .T. ) ;
#27261 = CARTESIAN_POINT ( 'NONE',  ( 124.5954081442453116, -6.222761293078241884, -8.102969835052219238 ) ) ;
#27262 = CARTESIAN_POINT ( 'NONE',  ( 123.9714148109119805, -8.899110576539710493, -16.42337572283490132 ) ) ;
#27263 = EDGE_CURVE ( 'NONE', #2604, #8725, #35012, .T. ) ;
#27264 = CARTESIAN_POINT ( 'NONE',  ( 138.2184548109119930, -3.657522433324904565, -16.24880879654457289 ) ) ;
#27265 = CARTESIAN_POINT ( 'NONE',  ( 114.4413952545248350, -9.868328341294098749, -15.46607636864997204 ) ) ;
#27266 = CARTESIAN_POINT ( 'NONE',  ( 120.2065265278262700, -1.036737761566197014, -17.24079555149560861 ) ) ;
#27267 = CARTESIAN_POINT ( 'NONE',  ( 70.19189222814998175, -58.18802696105826300, -36.47801710466001879 ) ) ;
#27268 = CARTESIAN_POINT ( 'NONE',  ( 113.4202548109119846, 0.1319031606808879209, -14.10382304977623669 ) ) ;
#27269 = CARTESIAN_POINT ( 'NONE',  ( 106.9404577545248145, -7.250697342233347165, -7.631215200338321125 ) ) ;
#27270 = CARTESIAN_POINT ( 'NONE',  ( 117.2294421295248270, -10.07080413108645267, -4.893215200338313586 ) ) ;
#27271 = CARTESIAN_POINT ( 'NONE',  ( 114.6497546295247929, -4.863998795839590272, -7.631215200338315796 ) ) ;
#27272 = CARTESIAN_POINT ( 'NONE',  ( 125.9568481442452850, -6.344957434206665248, -7.627207830600338134 ) ) ;
#27273 = CARTESIAN_POINT ( 'NONE',  ( 123.6877814775786533, -3.383040157471821630, -19.15922257007629170 ) ) ;
#27274 = CARTESIAN_POINT ( 'NONE',  ( 114.7192077545248452, -7.250697342233347165, -7.631215200338321125 ) ) ;
#27275 = CARTESIAN_POINT ( 'NONE',  ( 119.0929214775786278, -5.638512984488999180, -18.83840828888717311 ) ) ;
#27276 = CARTESIAN_POINT ( 'NONE',  ( 113.3068014775786594, -8.166667518702817929, -8.995218007635859436 ) ) ;
#27277 = ORIENTED_EDGE ( 'NONE', *, *, #10583, .F. ) ;
#27278 = CARTESIAN_POINT ( 'NONE',  ( 112.4559014775786778, -0.1624402480850797581, -16.17319339645315424 ) ) ;
#27279 = CARTESIAN_POINT ( 'NONE',  ( 112.8529881442453160, -7.894159318335828068, -9.358103419637847864 ) ) ;
#27280 = CARTESIAN_POINT ( 'NONE',  ( 124.1415948109119540, -6.344957434206665248, -7.627207830600338134 ) ) ;
#27281 = CARTESIAN_POINT ( 'NONE',  ( 112.6828081442453282, -7.893985811506177619, -18.51759400769804742 ) ) ;
#27282 = CARTESIAN_POINT ( 'NONE',  ( 112.1155414775786454, -10.15424416112533912, -14.75197769757731336 ) ) ;
#27283 = ORIENTED_EDGE ( 'NONE', *, *, #38229, .F. ) ;
#27284 = EDGE_CURVE ( 'NONE', #28048, #970, #15390, .T. ) ;
#27285 = CARTESIAN_POINT ( 'NONE',  ( 118.2987481442453088, -7.894159318335828068, -9.358103419637847864 ) ) ;
#27286 = ADVANCED_FACE ( 'NONE', ( #42649 ), #11417, .F. ) ;
#27287 = EDGE_CURVE ( 'NONE', #19939, #5495, #24868, .T. ) ;
#27288 = CARTESIAN_POINT ( 'NONE',  ( 106.2459265045248173, -7.250697342233347165, -19.15521520033831138 ) ) ;
#27289 = AXIS2_PLACEMENT_3D ( 'NONE', #8784, #9242, #22689 ) ;
#27290 = CARTESIAN_POINT ( 'NONE',  ( 123.8579614775786126, -9.859900752359378018, -12.68260735090039759 ) ) ;
#27291 = CARTESIAN_POINT ( 'NONE',  ( 116.8392602215938751, -1.056629477399154915, -17.00092880501178527 ) ) ;
#27292 = CARTESIAN_POINT ( 'NONE',  ( 111.6632702545248605, -10.62599879583958717, -15.77991374673208469 ) ) ;
#27293 = ORIENTED_EDGE ( 'NONE', *, *, #11769, .F. ) ;
#27294 = CARTESIAN_POINT ( 'NONE',  ( 72.54180985774836188, -51.37213739997068984, -33.02251202313252065 ) ) ;
#27295 = CARTESIAN_POINT ( 'NONE',  ( 125.8433948109119456, -1.834011780172310813, -8.268836392978581529 ) ) ;
#27296 = DIRECTION ( 'NONE',  ( -1.000000000000000000, 0.000000000000000000, -0.000000000000000000 ) ) ;
#27297 = CARTESIAN_POINT ( 'NONE',  ( 112.9097148109120070, 0.2603800115204892296, -16.42320221600525088 ) ) ;
#27298 = CARTESIAN_POINT ( 'NONE',  ( 117.0059805889377316, 1.765016726092817789, -5.580912673505509680 ) ) ;
#27299 = FACE_OUTER_BOUND ( 'NONE', #13092, .T. ) ;
#27300 = CARTESIAN_POINT ( 'NONE',  ( 105.4819421295248247, -9.868328341294093420, -13.39321520033831447 ) ) ;
#27301 = DIRECTION ( 'NONE',  ( 0.000000000000000000, 0.000000000000000000, 1.000000000000000000 ) ) ;
#27302 = CARTESIAN_POINT ( 'NONE',  ( 118.7525614775786380, -8.166667518702819706, -8.995218007635861213 ) ) ;
#27303 = CARTESIAN_POINT ( 'NONE',  ( 122.7299391859119737, -1.406689858478935573, -17.56299727309130887 ) ) ;
#27304 = CARTESIAN_POINT ( 'NONE',  ( 70.19189222814998175, -61.33395589173652951, -37.73637771078367109 ) ) ;
#27305 = CARTESIAN_POINT ( 'NONE',  ( 124.1190016859119822, -0.6942167230864397798, -9.935906262977766801 ) ) ;
#27306 = CARTESIAN_POINT ( 'NONE',  ( 119.5467348109119712, -5.574606645277164318, -18.38911715685844683 ) ) ;
#27307 = ORIENTED_EDGE ( 'NONE', *, *, #6990, .F. ) ;
#27308 = DIRECTION ( 'NONE',  ( 0.9908103287288505534, -0.1352586133457944206, 0.000000000000000000 ) ) ;
#27309 = CARTESIAN_POINT ( 'NONE',  ( 118.4122014775786340, 0.5811942927096110934, -14.16772938898807510 ) ) ;
#27310 = DIRECTION ( 'NONE',  ( -0.000000000000000000, -0.9284778069183718952, -0.3713878862591649677 ) ) ;
#27311 = CARTESIAN_POINT ( 'NONE',  ( 115.0086014775786509, -5.574606645277164318, -18.38911715685844683 ) ) ;
#27312 = CARTESIAN_POINT ( 'NONE',  ( 123.8579614775786126, 0.5811942927096110934, -14.16772938898807510 ) ) ;
#27313 = CARTESIAN_POINT ( 'NONE',  ( 112.6356140045247827, -10.62599879583958717, -11.00651665394454604 ) ) ;
#27314 = ADVANCED_FACE ( 'NONE', ( #31921 ), #1139, .T. ) ;
#27315 = CARTESIAN_POINT ( 'NONE',  ( 106.2459265045248173, -2.791137627527939813, -8.388885654883777576 ) ) ;
#27316 = CARTESIAN_POINT ( 'NONE',  ( 83.54882120758564668, -32.57787328110440939, -23.89321520033832513 ) ) ;
#27317 = CIRCLE ( 'NONE', #39706, 6.479565957685751165 ) ;
#27318 = CARTESIAN_POINT ( 'NONE',  ( 116.4267681442453153, -6.222761293078241884, -8.102969835052219238 ) ) ;
#27319 = CARTESIAN_POINT ( 'NONE',  ( 119.5467348109119712, -5.574606645277164318, -18.38911715685844683 ) ) ;
#27320 = DIRECTION ( 'NONE',  ( 0.000000000000000000, 0.000000000000000000, -1.000000000000000000 ) ) ;
#27321 = DIRECTION ( 'NONE',  ( -0.5735764363510450492, -0.3127926500124816878, 0.7570804645221038687 ) ) ;
#27322 = CARTESIAN_POINT ( 'NONE',  ( 108.6073327545248048, -6.936859964151250502, -8.388885654883777576 ) ) ;
#27323 = EDGE_LOOP ( 'NONE', ( #32370, #44278, #41520, #35780 ) ) ;
#27324 = CARTESIAN_POINT ( 'NONE',  ( 109.2294421526880086, -0.4654583522832261289, -15.91752710485221733 ) ) ;
#27325 = CARTESIAN_POINT ( 'NONE',  ( 112.3424481442453384, -6.344957434206662583, -7.627207830600332805 ) ) ;
#27326 = CARTESIAN_POINT ( 'NONE',  ( 123.0525060002550788, -2.334846009198419559, -18.01015021110789505 ) ) ;
#27327 = CARTESIAN_POINT ( 'NONE',  ( 79.79010115959992788, 5.106172230548961188, -19.89321520033831447 ) ) ;
#27328 = CARTESIAN_POINT ( 'NONE',  ( 119.6740016859119748, -0.6942167230862511529, -9.935906262978006609 ) ) ;
#27329 = EDGE_LOOP ( 'NONE', ( #35392, #43830, #13068, #42022, #37714 ) ) ;
#27330 = CARTESIAN_POINT ( 'NONE',  ( 114.2818621053768737, 0.3967854368539331933, -16.28112951403851838 ) ) ;
#27331 = VECTOR ( 'NONE', #38213, 1000.000000000000114 ) ;
#27332 = EDGE_LOOP ( 'NONE', ( #12706, #20297, #16263, #20489, #16994, #5428 ) ) ;
#27333 = CARTESIAN_POINT ( 'NONE',  ( 123.1205148109119563, -1.834011780172310813, -8.268836392978581529 ) ) ;
#27334 = CARTESIAN_POINT ( 'NONE',  ( 112.4559014775786494, -9.988377603198976828, -10.36322818467138340 ) ) ;
#27335 = CARTESIAN_POINT ( 'NONE',  ( 116.7671281442453335, -7.643976991954077427, -18.09477374809248928 ) ) ;
#27336 = CARTESIAN_POINT ( 'NONE',  ( 121.1350814775786233, 0.5811942927096110934, -14.16772938898807510 ) ) ;
#27337 = CARTESIAN_POINT ( 'NONE',  ( 119.1496481442453046, -3.383040157471821630, -19.15922257007629170 ) ) ;
#27338 = EDGE_CURVE ( 'NONE', #39489, #24400, #9462, .T. ) ;
#27339 = CARTESIAN_POINT ( 'NONE',  ( 116.3860827545247787, -2.477300249445798297, -19.15521520033831138 ) ) ;
#27340 = EDGE_CURVE ( 'NONE', #16620, #18524, #42875, .T. ) ;
#27341 = CARTESIAN_POINT ( 'NONE',  ( 113.7606148109119886, -7.894159318335828068, -9.358103419637847864 ) ) ;
#27342 = CARTESIAN_POINT ( 'NONE',  ( 61.69189222814998175, -69.76310523276724496, -16.89321520033831447 ) ) ;
#27343 = VERTEX_POINT ( 'NONE', #33030 ) ;
#27344 = EDGE_CURVE ( 'NONE', #19363, #25522, #33456, .T. ) ;
#27345 = CARTESIAN_POINT ( 'NONE',  ( 116.5402214775786405, 0.2603800115204892296, -16.42320221600525088 ) ) ;
#27346 = CARTESIAN_POINT ( 'NONE',  ( 121.2714235609119697, 0.6414057260225851653, -11.69287257290600657 ) ) ;
#27347 = CARTESIAN_POINT ( 'NONE',  ( 115.3489614775786407, -9.261995988541697145, -16.69588392320189030 ) ) ;
#27348 = AXIS2_PLACEMENT_3D ( 'NONE', #28021, #38260, #14778 ) ;
#27349 = ORIENTED_EDGE ( 'NONE', *, *, #13318, .F. ) ;
#27350 = CARTESIAN_POINT ( 'NONE',  ( 125.7866681442452688, -0.4660016031367893996, -10.09054647747474043 ) ) ;
#27351 = DIRECTION ( 'NONE',  ( 0.000000000000000000, -1.000000000000000000, 0.000000000000000000 ) ) ;
#27352 = CARTESIAN_POINT ( 'NONE',  ( 125.4584548109119737, -6.456500312860584678, -19.12873567962219568 ) ) ;
#27353 = CARTESIAN_POINT ( 'NONE',  ( 124.9305558011493957, -1.149058757900108585, -17.09122335155391781 ) ) ;
#27354 = CARTESIAN_POINT ( 'NONE',  ( 114.8384214775786489, -10.15424416112533912, -14.75197769757731336 ) ) ;
#27355 = FACE_OUTER_BOUND ( 'NONE', #22093, .T. ) ;
#27356 = CARTESIAN_POINT ( 'NONE',  ( 118.2420214775786320, -6.222761293078241884, -8.102969835052219238 ) ) ;
#27357 = CARTESIAN_POINT ( 'NONE',  ( 67.69189222814998175, -49.76310523276723785, -34.89321520033831092 ) ) ;
#27358 = CARTESIAN_POINT ( 'NONE',  ( 114.6682414775786469, -7.894159318335828068, -9.358103419637847864 ) ) ;
#27359 = CARTESIAN_POINT ( 'NONE',  ( 115.8027748109119841, -0.4660016031367893996, -10.09054647747474043 ) ) ;
#27360 = CARTESIAN_POINT ( 'NONE',  ( 122.6604860609119640, -6.564341423271550902, -7.887810678476487425 ) ) ;
#27361 = CARTESIAN_POINT ( 'NONE',  ( 117.3343948109119737, -3.383040157471821630, -19.15922257007629170 ) ) ;
#27362 = CARTESIAN_POINT ( 'NONE',  ( 112.2289948109119848, -7.643976991954077427, -18.09477374809248928 ) ) ;
#27363 = CARTESIAN_POINT ( 'NONE',  ( 116.6536748109119941, -10.15424416112533912, -14.75197769757731336 ) ) ;
#27364 = VERTEX_POINT ( 'NONE', #43776 ) ;
#27365 = CARTESIAN_POINT ( 'NONE',  ( 112.3424481442453384, -6.344957434206662583, -7.627207830600332805 ) ) ;
#27366 = CARTESIAN_POINT ( 'NONE',  ( 107.0099108795247815, -8.938348069036489818, -9.318865927141430916 ) ) ;
#27367 = CARTESIAN_POINT ( 'NONE',  ( 105.2041296295248287, -4.863998795839590272, -8.388885654883775800 ) ) ;
#27368 = DIRECTION ( 'NONE',  ( -0.9609149988134837450, 0.1028163501681639419, -0.2570431154366518145 ) ) ;
#27369 = CARTESIAN_POINT ( 'NONE',  ( 109.2324108795247923, -8.938348069036489818, -9.318865927141436245 ) ) ;
#27370 = CARTESIAN_POINT ( 'NONE',  ( 118.8660148109119774, -10.30919188438810075, -12.61870101168855918 ) ) ;
#27371 = ORIENTED_EDGE ( 'NONE', *, *, #14186, .F. ) ;
#27372 = CARTESIAN_POINT ( 'NONE',  ( 125.1626748109119802, -9.988377603198957289, -10.36322818467135498 ) ) ;
#27373 = CARTESIAN_POINT ( 'NONE',  ( 116.3133148109120043, -2.084020599724406786, -8.691656652584148546 ) ) ;
#27374 = CARTESIAN_POINT ( 'NONE',  ( 124.2193060444391790, -1.267766418764731728, -16.93314635290706605 ) ) ;
#27375 = EDGE_CURVE ( 'NONE', #27136, #34675, #39883, .T. ) ;
#27376 = CARTESIAN_POINT ( 'NONE',  ( 122.8936081442453059, 0.2603800115204892296, -16.42320221600525088 ) ) ;
#27377 = CARTESIAN_POINT ( 'NONE',  ( 106.3153796295248412, -4.863998795839590272, -19.15521520033831493 ) ) ;
#27378 = DIRECTION ( 'NONE',  ( 0.000000000000000000, 0.3818493186865898892, -0.9242245927363040847 ) ) ;
#27379 = AXIS2_PLACEMENT_3D ( 'NONE', #23944, #38265, #38053 ) ;
#27380 = ORIENTED_EDGE ( 'NONE', *, *, #40058, .T. ) ;
#27381 = DIRECTION ( 'NONE',  ( 0.000000000000000000, 0.000000000000000000, 1.000000000000000000 ) ) ;
#27382 = CARTESIAN_POINT ( 'NONE',  ( 122.2696148109119889, -5.574606645277164318, -18.38911715685844683 ) ) ;
#27383 = CARTESIAN_POINT ( 'NONE',  ( 123.1772414775786189, -4.089484607189486809, -7.948022111789456723 ) ) ;
#27384 = CARTESIAN_POINT ( 'NONE',  ( 118.1285681442453068, -2.084020599724406786, -8.691656652584148546 ) ) ;
#27385 = CARTESIAN_POINT ( 'NONE',  ( 120.2274548109119934, 0.5811942927096110934, -14.16772938898807510 ) ) ;
#27386 = CARTESIAN_POINT ( 'NONE',  ( 94.20708369096698220, -25.89439488952623591, -12.28775498424876211 ) ) ;
#27387 = CARTESIAN_POINT ( 'NONE',  ( 127.0400190879707765, -1.259479977070091294, -9.357869521001603630 ) ) ;
#27388 = CARTESIAN_POINT ( 'NONE',  ( 122.7801548109119665, -6.222761293078241884, -8.102969835052219238 ) ) ;
#27389 = ORIENTED_EDGE ( 'NONE', *, *, #6378, .F. ) ;
#27390 = AXIS2_PLACEMENT_3D ( 'NONE', #17912, #357, #39335 ) ;
#27391 = CARTESIAN_POINT ( 'NONE',  ( 83.83554121260367253, -25.99489077589524300, -13.39321520033831625 ) ) ;
#27392 = EDGE_CURVE ( 'NONE', #7972, #31497, #1122, .T. ) ;
#27393 = CIRCLE ( 'NONE', #26665, 2.000000000000000444 ) ;
#27394 = CARTESIAN_POINT ( 'NONE',  ( 116.4267681442453153, -3.383040157471821630, -19.15922257007629170 ) ) ;
#27395 = CARTESIAN_POINT ( 'NONE',  ( 124.4252281442452812, -0.8288870151387760510, -10.36305467784173118 ) ) ;
#27396 = ORIENTED_EDGE ( 'NONE', *, *, #14986, .F. ) ;
#27397 = CARTESIAN_POINT ( 'NONE',  ( 123.3550173109119612, 0.2312338769422704887, -16.08380026872395874 ) ) ;
#27398 = CARTESIAN_POINT ( 'NONE',  ( 136.5278073585092216, -1.250741748839698575, -8.937135636257391269 ) ) ;
#27399 = CARTESIAN_POINT ( 'NONE',  ( 117.5613014775786525, 0.9020085738987339008, -11.91225656197089222 ) ) ;
#27400 = CARTESIAN_POINT ( 'NONE',  ( 108.0517077545248696, -7.250697342233347165, -7.631215200338321125 ) ) ;
#27401 = CARTESIAN_POINT ( 'NONE',  ( 118.2420214775786320, -6.222761293078241884, -8.102969835052219238 ) ) ;
#27402 = B_SPLINE_CURVE_WITH_KNOTS ( 'NONE', 3,
 ( #8912, #23507, #19617, #22810, #5473, #15755, #2280, #12338, #19393, #6164 ),
 .UNSPECIFIED., .F., .F.,
 ( 4, 2, 2, 2, 4 ),
 ( 0.000000000000000000, 0.2500000000000000000, 0.5000000000000000000, 0.7500000000000000000, 1.000000000000000000 ),
 .UNSPECIFIED. ) ;
#27403 = ORIENTED_EDGE ( 'NONE', *, *, #12343, .T. ) ;
#27404 = ORIENTED_EDGE ( 'NONE', *, *, #32901, .F. ) ;
#27405 = CARTESIAN_POINT ( 'NONE',  ( 111.9453614775786434, -1.561330072975668060, -17.79121239304076596 ) ) ;
#27406 = AXIS2_PLACEMENT_3D ( 'NONE', #6510, #37963, #6740 ) ;
#27407 = CARTESIAN_POINT ( 'NONE',  ( 123.1772414775786189, -5.574606645277164318, -18.38911715685844683 ) ) ;
#27408 =( NAMED_UNIT ( * ) SI_UNIT ( $, .STERADIAN. ) SOLID_ANGLE_UNIT ( ) );
#27409 = CARTESIAN_POINT ( 'NONE',  ( 114.8834831777918879, -0.01829820670803256055, -14.64321520033831447 ) ) ;
#27410 = CARTESIAN_POINT ( 'NONE',  ( 120.9649014775786355, -3.383040157471821630, -19.15922257007629170 ) ) ;
#27411 = VECTOR ( 'NONE', #7421, 1000.000000000000114 ) ;
#27412 = LINE ( 'NONE', #23771, #2195 ) ;
#27413 = CARTESIAN_POINT ( 'NONE',  ( 85.43169907558235820, -26.60966817898065884, -11.90521360603286816 ) ) ;
#27414 = B_SPLINE_CURVE_WITH_KNOTS ( 'NONE', 3,
 ( #8735, #22194, #35859, #29264, #43176, #36090, #11715, #15134, #43621, #1659 ),
 .UNSPECIFIED., .F., .F.,
 ( 4, 3, 3, 4 ),
 ( 0.000000000000000000, 0.0001671877548681239927, 0.0003343755096277610354, 0.0006463528481650629171 ),
 .UNSPECIFIED. ) ;
#27415 = CARTESIAN_POINT ( 'NONE',  ( 118.7525614775786380, -8.166667518702819706, -8.995218007635861213 ) ) ;
#27417 = CARTESIAN_POINT ( 'NONE',  ( 121.3052614775786111, -7.643976991954077427, -18.09477374809248928 ) ) ;
#27416 = CARTESIAN_POINT ( 'NONE',  ( 117.5613014775786525, 0.9020085738987339008, -11.91225656197089222 ) ) ;
#27418 = CARTESIAN_POINT ( 'NONE',  ( 31.16203868753470019, 11.28474725185576055, -19.39321520033831447 ) ) ;
#27419 = CARTESIAN_POINT ( 'NONE',  ( 116.9940348109119839, -9.988377603198976828, -10.36322818467138340 ) ) ;
#27420 = VERTEX_POINT ( 'NONE', #12090 ) ;
#27421 = AXIS2_PLACEMENT_3D ( 'NONE', #25769, #39898, #11863 ) ;
#27422 = CARTESIAN_POINT ( 'NONE',  ( 124.3117748109119844, 0.1319031606808879209, -14.10382304977623669 ) ) ;
#27423 = CARTESIAN_POINT ( 'NONE',  ( 125.2194014775786286, 0.1319031606810284196, -14.10382304977525614 ) ) ;
#27424 = CARTESIAN_POINT ( 'NONE',  ( 108.0517077545248696, -7.250697342233347165, -7.631215200338321125 ) ) ;
#27425 = CARTESIAN_POINT ( 'NONE',  ( 115.2748327545248657, -6.936859964151250502, -8.388885654883777576 ) ) ;
#27426 = CARTESIAN_POINT ( 'NONE',  ( 106.9404577545248145, -7.250697342233347165, -7.631215200338321125 ) ) ;
#27427 = CARTESIAN_POINT ( 'NONE',  ( 121.3052614775786111, -1.834011780172310813, -8.268836392978581529 ) ) ;
#27428 = CARTESIAN_POINT ( 'NONE',  ( 122.5532481442453019, 0.4262465694468514643, -12.03445270309931736 ) ) ;
#27429 = ORIENTED_EDGE ( 'NONE', *, *, #30362, .T. ) ;
#27430 = CARTESIAN_POINT ( 'NONE',  ( 124.1983214775786166, -8.166667518702819706, -8.995218007635861213 ) ) ;
#27431 = CARTESIAN_POINT ( 'NONE',  ( 112.4967077545247633, -7.250697342233347165, -7.631215200338321125 ) ) ;
#27432 = FACE_OUTER_BOUND ( 'NONE', #750, .T. ) ;
#27433 = CARTESIAN_POINT ( 'NONE',  ( 122.8368814775786291, -1.561330072975668948, -17.79121239304076951 ) ) ;
#27434 = CARTESIAN_POINT ( 'NONE',  ( 120.7947214775786193, -9.261995988541697145, -16.69588392320189030 ) ) ;
#27435 = LINE ( 'NONE', #16726, #31575 ) ;
#27436 = CARTESIAN_POINT ( 'NONE',  ( 112.9664414775786412, 0.5811942927096154232, -14.16772938898807155 ) ) ;
#27437 = CARTESIAN_POINT ( 'NONE',  ( 111.5849102067643770, -1.223627541775779370, -16.99192386690437928 ) ) ;
#27438 = CARTESIAN_POINT ( 'NONE',  ( 114.0941296295247867, -4.863998795839590272, -8.388885654883775800 ) ) ;
#27439 = ORIENTED_EDGE ( 'NONE', *, *, #44274, .F. ) ;
#27440 = DIRECTION ( 'NONE',  ( 0.000000000000000000, -0.3818493186865927203, 0.9242245927363029745 ) ) ;
#27441 = CARTESIAN_POINT ( 'NONE',  ( 114.3112643147880476, -2.395992375830784837, -17.92872468182854107 ) ) ;
#27442 = CARTESIAN_POINT ( 'NONE',  ( 124.4252281442452812, -0.8288870151387760510, -10.36305467784173118 ) ) ;
#27443 = AXIS2_PLACEMENT_3D ( 'NONE', #1835, #8920, #5937 ) ;
#27444 = CARTESIAN_POINT ( 'NONE',  ( 116.5944421295247793, 0.8980012041604618078, -13.39321520033831447 ) ) ;
#27445 = CARTESIAN_POINT ( 'NONE',  ( 107.2182702545248105, 0.1403307496149616695, -11.32035403202665336 ) ) ;
#27446 = CARTESIAN_POINT ( 'NONE',  ( 123.1772414775786189, -5.574606645277164318, -18.38911715685844683 ) ) ;
#27447 = CARTESIAN_POINT ( 'NONE',  ( 117.3343948109119737, -6.222761293078241884, -8.102969835052219238 ) ) ;
#27448 = CARTESIAN_POINT ( 'NONE',  ( 113.4769814775786330, 0.4262465694468514643, -12.03445270309931736 ) ) ;
#27449 = ORIENTED_EDGE ( 'NONE', *, *, #10351, .F. ) ;
#27450 = CARTESIAN_POINT ( 'NONE',  ( 120.5768923109119868, -0.4387604401700512802, -15.73000352943951619 ) ) ;
#27451 = CARTESIAN_POINT ( 'NONE',  ( 118.9794681442453026, -9.261995988541697145, -16.69588392320189030 ) ) ;
#27452 = EDGE_CURVE ( 'NONE', #30525, #34165, #13827, .T. ) ;
#27453 = LINE ( 'NONE', #41812, #28788 ) ;
#27454 = ORIENTED_EDGE ( 'NONE', *, *, #18643, .T. ) ;
#27455 = CARTESIAN_POINT ( 'NONE',  ( 70.19189222814998175, -100.0979043305785581, -53.24182196210380624 ) ) ;
#27456 = VECTOR ( 'NONE', #24155, 1000.000000000000000 ) ;
#27457 = VERTEX_POINT ( 'NONE', #25995 ) ;
#27458 = CARTESIAN_POINT ( 'NONE',  ( 114.2711548109119803, -0.1624402480850797581, -16.17319339645315424 ) ) ;
#27459 =( BOUNDED_SURFACE ( )  B_SPLINE_SURFACE ( 1, 2, ( 
 ( #24366, #14322, #41483, #27570, #34384, #34818, #31413, #44680, #7034, #10465, #27787, #23705, #3601, #16865, #10241, #38252, #30756, #23932, #17515, #20505, #13441, #180, #27346, #41266, #3166, #17088, #28014, #20724, #14543, #22285, #38924, #21610, #1080, #8156, #7694, #7923, #11578, #32315, #21833, #39617, #42368, #1523, #29123, #22061, #29350, #42589, #24805, #38697, #28460, #7464, #4269, #21382, #8378, #25487, #630, #25710, #852, #36178, #35953, #18188, #4944, #4500, #35265, #18641, #14771 ),
 ( #42816, #14993, #4042, #10905, #18858, #32750, #28686, #15444, #11129, #17964, #35726, #31863, #25031, #35497, #4724, #39390, #32083, #11351, #25262, #39158, #18423, #28907, #32533, #1304, #15216, #11802, #43034, #5168, #29574, #43942, #12938, #15900, #1975, #8823, #9284, #5844, #19085, #26607, #16122, #2196, #16581, #23191, #44175, #5399, #33880, #33199, #32971, #37071, #26835, #29800, #19766, #16349, #43264, #19540, #30250, #26381, #6073, #12707, #33647, #43712, #2424, #40748, #9505, #2649, #19995 ) ),
 .UNSPECIFIED., .F., .F., .F. ) 
 B_SPLINE_SURFACE_WITH_KNOTS ( ( 2, 2 ),
 ( 3, 2, 2, 2, 2, 2, 2, 2, 2, 2, 2, 2, 2, 2, 2, 2, 2, 2, 2, 2, 2, 2, 2, 2, 2, 2, 2, 2, 2, 2, 2, 2, 3 ),
 ( 0.000000000000000000, 1.000000000000000000 ),
 ( 0.000000000000000000, 0.03125000000000000000, 0.06250000000000000000, 0.09375000000000000000, 0.1250000000000000000, 0.1562500000000000000, 0.1875000000000000000, 0.2187500000000000000, 0.2500000000000000000, 0.2812500000000000000, 0.3125000000000000000, 0.3437500000000000000, 0.3750000000000000000, 0.4062500000000000000, 0.4375000000000000000, 0.4687500000000000000, 0.5000000000000000000, 0.5312500000000000000, 0.5625000000000000000, 0.5937500000000000000, 0.6250000000000000000, 0.6562500000000000000, 0.6875000000000000000, 0.7187500000000000000, 0.7500000000000000000, 0.7812500000000000000, 0.8125000000000000000, 0.8437500000000000000, 0.8750000000000000000, 0.9062500000000000000, 0.9375000000000000000, 0.9687500000000000000, 1.000000000000000000 ),
 .UNSPECIFIED. ) 
 GEOMETRIC_REPRESENTATION_ITEM ( )  RATIONAL_B_SPLINE_SURFACE ( (
 ( 1.000000000000000000, 0.9238795325112869605, 1.000000000000000000, 0.9238795325112869605, 1.000000000000000000, 0.9238795325112869605, 1.000000000000000000, 0.9238795325112869605, 1.000000000000000000, 0.9238795325112869605, 1.000000000000000000, 0.9238795325112869605, 1.000000000000000000, 0.9238795325112869605, 1.000000000000000000, 0.9238795325112869605, 1.000000000000000000, 0.9238795325112869605, 1.000000000000000000, 0.9238795325112869605, 1.000000000000000000, 0.9238795325112869605, 1.000000000000000000, 0.9238795325112869605, 1.000000000000000000, 0.9238795325112869605, 1.000000000000000000, 0.9238795325112869605, 1.000000000000000000, 0.9238795325112869605, 1.000000000000000000, 0.9238795325112869605, 1.000000000000000000, 0.9238795325112869605, 1.000000000000000000, 0.9238795325112869605, 1.000000000000000000, 0.9238795325112869605, 1.000000000000000000, 0.9238795325112869605, 1.000000000000000000, 0.9238795325112869605, 1.000000000000000000, 0.9238795325112869605, 1.000000000000000000, 0.9238795325112869605, 1.000000000000000000, 0.9238795325112869605, 1.000000000000000000, 0.9238795325112869605, 1.000000000000000000, 0.9238795325112869605, 1.000000000000000000, 0.9238795325112869605, 1.000000000000000000, 0.9238795325112869605, 1.000000000000000000, 0.9238795325112869605, 1.000000000000000000, 0.9238795325112869605, 1.000000000000000000, 0.9238795325112869605, 1.000000000000000000, 0.9238795325112869605, 1.000000000000000000),
 ( 1.000000000000000000, 0.9238795325112869605, 1.000000000000000000, 0.9238795325112869605, 1.000000000000000000, 0.9238795325112869605, 1.000000000000000000, 0.9238795325112869605, 1.000000000000000000, 0.9238795325112869605, 1.000000000000000000, 0.9238795325112869605, 1.000000000000000000, 0.9238795325112869605, 1.000000000000000000, 0.9238795325112869605, 1.000000000000000000, 0.9238795325112869605, 1.000000000000000000, 0.9238795325112869605, 1.000000000000000000, 0.9238795325112869605, 1.000000000000000000, 0.9238795325112869605, 1.000000000000000000, 0.9238795325112869605, 1.000000000000000000, 0.9238795325112869605, 1.000000000000000000, 0.9238795325112869605, 1.000000000000000000, 0.9238795325112869605, 1.000000000000000000, 0.9238795325112869605, 1.000000000000000000, 0.9238795325112869605, 1.000000000000000000, 0.9238795325112869605, 1.000000000000000000, 0.9238795325112869605, 1.000000000000000000, 0.9238795325112869605, 1.000000000000000000, 0.9238795325112869605, 1.000000000000000000, 0.9238795325112869605, 1.000000000000000000, 0.9238795325112869605, 1.000000000000000000, 0.9238795325112869605, 1.000000000000000000, 0.9238795325112869605, 1.000000000000000000, 0.9238795325112869605, 1.000000000000000000, 0.9238795325112869605, 1.000000000000000000, 0.9238795325112869605, 1.000000000000000000, 0.9238795325112869605, 1.000000000000000000, 0.9238795325112869605, 1.000000000000000000, 0.9238795325112869605, 1.000000000000000000) ) ) 
 REPRESENTATION_ITEM ( '' )  SURFACE ( )  );
#27460 = CARTESIAN_POINT ( 'NONE',  ( 115.2355081442453155, 0.1319031606808879209, -14.10382304977623669 ) ) ;
#27461 = FACE_OUTER_BOUND ( 'NONE', #28803, .T. ) ;
#27462 = CARTESIAN_POINT ( 'NONE',  ( 123.9106423109119675, -0.4387604401700512802, -15.73000352943951619 ) ) ;
#27463 = ORIENTED_EDGE ( 'NONE', *, *, #8044, .F. ) ;
#27464 = DIRECTION ( 'NONE',  ( -0.9908103287288499983, 0.1352586133457985007, -3.469446951953614978E-15 ) ) ;
#27465 = CARTESIAN_POINT ( 'NONE',  ( 124.9774582099998383, 2.655747558278632070, -12.25998410011163031 ) ) ;
#27466 = CARTESIAN_POINT ( 'NONE',  ( 113.8857702545248003, -10.62599879583958717, -15.77991374673208469 ) ) ;
#27467 = AXIS2_PLACEMENT_3D ( 'NONE', #83, #32206, #4169 ) ;
#27468 = CARTESIAN_POINT ( 'NONE',  ( 64.19189222814998175, -49.76310523276725206, -36.33917278160905084 ) ) ;
#27469 = CARTESIAN_POINT ( 'NONE',  ( 123.5743281442453139, -2.084020599724406786, -8.691656652584148546 ) ) ;
#27470 = CARTESIAN_POINT ( 'NONE',  ( 114.2144281442453178, -1.833838273342658809, -17.42832698103878286 ) ) ;
#27471 = FACE_OUTER_BOUND ( 'NONE', #23583, .T. ) ;
#27472 = ORIENTED_EDGE ( 'NONE', *, *, #12948, .T. ) ;
#27473 = CARTESIAN_POINT ( 'NONE',  ( 70.19189222814998175, -70.34019061884472990, -41.33884020749756871 ) ) ;
#27474 = CARTESIAN_POINT ( 'NONE',  ( 63.43088374006683239, -46.96404483173760269, -10.39321520033831625 ) ) ;
#27475 = AXIS2_PLACEMENT_3D ( 'NONE', #40991, #34119, #40298 ) ;
#27476 = CARTESIAN_POINT ( 'NONE',  ( 71.62928943233082180, 0.3619606153155430217, -14.39321520033831625 ) ) ;
#27477 = CARTESIAN_POINT ( 'NONE',  ( -2.511237114481913668, -7.038084878006822365, -19.27282189517453048 ) ) ;
#27479 = CARTESIAN_POINT ( 'NONE',  ( 125.2194014775786286, -10.30919188438810075, -12.61870101168855918 ) ) ;
#27478 = DIRECTION ( 'NONE',  ( -0.2768435750659253847, -0.3568721902840677473, 0.8921882507333133150 ) ) ;
#27480 = CARTESIAN_POINT ( 'NONE',  ( 126.6375681442452930, -10.15424416112533912, -14.75197769757731336 ) ) ;
#27481 = ORIENTED_EDGE ( 'NONE', *, *, #18422, .T. ) ;
#27482 = CARTESIAN_POINT ( 'NONE',  ( 112.9097148109120070, 0.2603800115204892296, -16.42320221600525088 ) ) ;
#27483 = DIRECTION ( 'NONE',  ( 0.000000000000000000, 0.6004852223388321697, -0.7996358532186279566 ) ) ;
#27484 = CARTESIAN_POINT ( 'NONE',  ( 114.0246765045248196, -7.250697342233347165, -19.15521520033831138 ) ) ;
#27485 = CARTESIAN_POINT ( 'NONE',  ( 125.8433948109119456, -7.643976991954077427, -18.09477374809248928 ) ) ;
#27486 = CIRCLE ( 'NONE', #12908, 15.89999999999999680 ) ;
#27487 = CARTESIAN_POINT ( 'NONE',  ( 122.2128881442453263, -7.643976991954077427, -18.09477374809248928 ) ) ;
#27488 = CARTESIAN_POINT ( 'NONE',  ( 112.6119297178594536, -0.3595008806742178709, -15.96590799893915502 ) ) ;
#27489 = CARTESIAN_POINT ( 'NONE',  ( 108.3295202545248657, 0.1403307496149616695, -11.32035403202665336 ) ) ;
#27490 = DIRECTION ( 'NONE',  ( 0.000000000000000000, 0.000000000000000000, 1.000000000000000000 ) ) ;
#27491 = CARTESIAN_POINT ( 'NONE',  ( 84.10271796608054728, -31.10763468207608895, -20.89321520033831447 ) ) ;
#27492 = CARTESIAN_POINT ( 'NONE',  ( 112.7395348109119766, -4.153390946401321671, -8.397313243818183892 ) ) ;
#27493 = DIRECTION ( 'NONE',  ( -0.9908103287288504424, 0.1352586133457954476, 0.000000000000000000 ) ) ;
#27494 = CARTESIAN_POINT ( 'NONE',  ( 117.9016614775786280, -9.988377603198960841, -10.36322818467135853 ) ) ;
#27495 = CARTESIAN_POINT ( 'NONE',  ( 111.6632702545248605, -10.62599879583958717, -15.77991374673208469 ) ) ;
#27496 = CARTESIAN_POINT ( 'NONE',  ( 94.20708369096698220, -26.81768470319947184, -13.17593392366846672 ) ) ;
#27497 = CARTESIAN_POINT ( 'NONE',  ( 112.0020881442453344, -9.565557343593413364, -10.61323700422348004 ) ) ;
#27498 = CARTESIAN_POINT ( 'NONE',  ( 112.1114130180079798, 0.7607806665037644134, -14.64321520033833046 ) ) ;
#27499 = CARTESIAN_POINT ( 'NONE',  ( 120.2841814775786276, 0.9020085738987339008, -11.91225656197089222 ) ) ;
#27500 = CARTESIAN_POINT ( 'NONE',  ( 116.8238548109119819, -4.089484607189486809, -7.948022111789456723 ) ) ;
#27501 = VERTEX_POINT ( 'NONE', #32810 ) ;
#27502 = CARTESIAN_POINT ( 'NONE',  ( 114.3278814775786429, 0.1319031606808879209, -14.10382304977623669 ) ) ;
#27503 = CARTESIAN_POINT ( 'NONE',  ( 111.5482748109120053, -0.1624402480850797581, -16.17319339645315424 ) ) ;
#27504 = CARTESIAN_POINT ( 'NONE',  ( 123.1772414775786189, -4.089484607189486809, -7.948022111789456723 ) ) ;
#27505 = CARTESIAN_POINT ( 'NONE',  ( 113.1366214775786432, -1.834011780172310813, -8.268836392978581529 ) ) ;
#27506 = AXIS2_PLACEMENT_3D ( 'NONE', #38381, #17651, #14229 ) ;
#27507 = CARTESIAN_POINT ( 'NONE',  ( 115.4624148109119943, -4.153390946401321671, -8.397313243818183892 ) ) ;
#27508 = EDGE_LOOP ( 'NONE', ( #16306, #9545, #37106, #347, #68 ) ) ;
#27509 = CARTESIAN_POINT ( 'NONE',  ( 116.8238548109119819, -5.574606645277164318, -18.38911715685844683 ) ) ;
#27510 = CARTESIAN_POINT ( 'NONE',  ( 116.8805814775786445, -6.344957434206662583, -7.627207830600332805 ) ) ;
#27511 = CARTESIAN_POINT ( 'NONE',  ( 122.1561614775786353, -8.899110576539710493, -16.42337572283490132 ) ) ;
#27512 = CARTESIAN_POINT ( 'NONE',  ( 70.19189222814998175, -50.19222220871606766, -33.27972307567368659 ) ) ;
#27513 = CARTESIAN_POINT ( 'NONE',  ( 114.9970202545248412, -10.62599879583958717, -15.77991374673208469 ) ) ;
#27514 = ORIENTED_EDGE ( 'NONE', *, *, #41547, .T. ) ;
#27515 = AXIS2_PLACEMENT_3D ( 'NONE', #35910, #42991, #29306 ) ;
#27516 = LINE ( 'NONE', #41870, #4562 ) ;
#27517 = ADVANCED_FACE ( 'NONE', ( #9339 ), #30309, .F. ) ;
#27518 = CARTESIAN_POINT ( 'NONE',  ( 84.77016061404391678, -25.99489077589524300, -13.39321520033831625 ) ) ;
#27519 = CARTESIAN_POINT ( 'NONE',  ( 113.3277860444392076, -1.267766418764742165, -16.93314635290707315 ) ) ;
#27520 = SURFACE_STYLE_FILL_AREA ( #3114 ) ;
#27521 = CARTESIAN_POINT ( 'NONE',  ( 116.1231069823931961, 2.324083898875324738, -6.775768760798180246 ) ) ;
#27522 = CARTESIAN_POINT ( 'NONE',  ( 112.9097148109120070, -9.565557343593413364, -10.61323700422348004 ) ) ;
#27523 = CARTESIAN_POINT ( 'NONE',  ( 106.9404577545248145, -2.791137627527939813, -18.39754474579286025 ) ) ;
#27524 = CARTESIAN_POINT ( 'NONE',  ( 111.0001630180080809, 0.7607806665038616689, -14.64321520033831447 ) ) ;
#27525 = CARTESIAN_POINT ( 'NONE',  ( 117.7882081442453170, -6.344957434206665248, -7.627207830600338134 ) ) ;
#27526 = CARTESIAN_POINT ( 'NONE',  ( 73.07463722459043254, -61.28190943231786036, -36.82105141712754914 ) ) ;
#27527 = CARTESIAN_POINT ( 'NONE',  ( 115.9923838361194868, 0.1075849324169569909, -12.14321520033831625 ) ) ;
#27529 = CARTESIAN_POINT ( 'NONE',  ( 70.19189222814998175, -56.33107134722149567, -35.73524133214168330 ) ) ;
#27528 = AXIS2_PLACEMENT_3D ( 'NONE', #23895, #3352, #6551 ) ;
#27530 = CARTESIAN_POINT ( 'NONE',  ( 122.2696148109119889, -5.574606645277164318, -18.38911715685844683 ) ) ;
#27531 = EDGE_CURVE ( 'NONE', #14756, #43396, #42981, .T. ) ;
#27532 = ORIENTED_EDGE ( 'NONE', *, *, #41310, .F. ) ;
#27533 = CARTESIAN_POINT ( 'NONE',  ( 125.0492214775786266, -6.344957434206665248, -7.627207830600338134 ) ) ;
#27534 = CARTESIAN_POINT ( 'NONE',  ( 120.3976348109119812, -1.834011780172310813, -8.268836392978581529 ) ) ;
#27535 = CARTESIAN_POINT ( 'NONE',  ( 89.12784890491134604, -27.84333996136784961, -14.15691383771150136 ) ) ;
#27536 = CARTESIAN_POINT ( 'NONE',  ( 115.4056881442453459, -2.084020599724406786, -8.691656652584148546 ) ) ;
#27537 = EDGE_CURVE ( 'NONE', #5046, #18690, #8660, .T. ) ;
#27538 = EDGE_CURVE ( 'NONE', #39963, #30333, #36462, .T. ) ;
#27539 = CARTESIAN_POINT ( 'NONE',  ( 112.7962614775786676, -6.222761293078241884, -8.102969835052219238 ) ) ;
#27540 = CARTESIAN_POINT ( 'NONE',  ( 109.1629577545248395, -7.250697342233347165, -7.631215200338321125 ) ) ;
#27541 = CARTESIAN_POINT ( 'NONE',  ( 106.8015515045248378, -6.936859964151250502, -18.39754474579286025 ) ) ;
#27542 = CARTESIAN_POINT ( 'NONE',  ( 115.0664733795247798, -8.938348069036489818, -17.46756447353520159 ) ) ;
#27543 = CARTESIAN_POINT ( 'NONE',  ( 116.8805814775786445, -3.505236298600246325, -18.68346056562440793 ) ) ;
#27544 = CARTESIAN_POINT ( 'NONE',  ( 120.7947214775786193, -0.8288870151387760510, -10.36305467784173118 ) ) ;
#27545 = DIRECTION ( 'NONE',  ( 0.000000000000000000, 0.000000000000000000, -1.000000000000000000 ) ) ;
#27546 = CARTESIAN_POINT ( 'NONE',  ( 121.2714235609119697, 0.6414057260225851653, -11.69287257290600657 ) ) ;
#27547 = CARTESIAN_POINT ( 'NONE',  ( 110.6214733795247867, -1.325403438956436419, -9.854619843455211026 ) ) ;
#27548 = CARTESIAN_POINT ( 'NONE',  ( 69.69189222815028018, -41.76310523276638520, -7.393215200338315363 ) ) ;
#27549 = CARTESIAN_POINT ( 'NONE',  ( 112.1155414775786454, 0.9020085738987339008, -11.91225656197089222 ) ) ;
#27550 = CARTESIAN_POINT ( 'NONE',  ( 115.9162281442453235, -4.089484607189486809, -7.948022111789456723 ) ) ;
#27551 = CARTESIAN_POINT ( 'NONE',  ( 122.1743141859119817, -8.321307733199551748, -9.223433127585318303 ) ) ;
#27552 = CARTESIAN_POINT ( 'NONE',  ( 120.7157985609119635, -0.08252387247370887580, -11.91645802438286417 ) ) ;
#27553 = ORIENTED_EDGE ( 'NONE', *, *, #6097, .T. ) ;
#27554 = CARTESIAN_POINT ( 'NONE',  ( 123.3791889291123880, -2.608644173476851069, -15.14726574760354261 ) ) ;
#27555 = ORIENTED_EDGE ( 'NONE', *, *, #27531, .F. ) ;
#27556 = CARTESIAN_POINT ( 'NONE',  ( 120.5110881442453206, -6.344957434206665248, -7.627207830600338134 ) ) ;
#27557 = CARTESIAN_POINT ( 'NONE',  ( 114.1009748109119784, -4.089484607189486809, -7.948022111789456723 ) ) ;
#27558 = CARTESIAN_POINT ( 'NONE',  ( 119.4332814775786318, -8.899110576539710493, -16.42337572283490132 ) ) ;
#27559 = CARTESIAN_POINT ( 'NONE',  ( 120.2510376736034345, -8.245233026025740486, -17.07659070123625611 ) ) ;
#27560 = CARTESIAN_POINT ( 'NONE',  ( 122.6099748109119929, -9.261995988541697145, -16.69588392320189030 ) ) ;
#27561 = CARTESIAN_POINT ( 'NONE',  ( 117.9583881442453048, -10.30919188438810075, -12.61870101168855918 ) ) ;
#27562 = EDGE_CURVE ( 'NONE', #20193, #41948, #31578, .T. ) ;
#27563 = CARTESIAN_POINT ( 'NONE',  ( 116.2471765045247594, -7.250697342233347165, -19.15521520033831138 ) ) ;
#27564 = AXIS2_PLACEMENT_3D ( 'NONE', #43754, #39651, #1780 ) ;
#27565 = CARTESIAN_POINT ( 'NONE',  ( 112.0020881442453344, -9.565557343593413364, -10.61323700422348004 ) ) ;
#27566 = FACE_OUTER_BOUND ( 'NONE', #28721, .T. ) ;
#27567 = EDGE_LOOP ( 'NONE', ( #25399, #30041, #37244, #29909 ) ) ;
#27568 = CARTESIAN_POINT ( 'NONE',  ( 116.5969481442453031, 0.5811942927096154232, -14.16772938898807155 ) ) ;
#27569 = EDGE_CURVE ( 'NONE', #18860, #3693, #33479, .T. ) ;
#27570 = CARTESIAN_POINT ( 'NONE',  ( 119.9518141859119851, -0.8832429491016019485, -18.19431474523657855 ) ) ;
#27571 = EDGE_CURVE ( 'NONE', #43318, #26554, #38259, .T. ) ;
#27572 = CARTESIAN_POINT ( 'NONE',  ( 117.2209414775786485, -7.893985811506177619, -18.51759400769804742 ) ) ;
#27573 = EDGE_LOOP ( 'NONE', ( #27949, #32643, #9869, #42514 ) ) ;
#27574 = CARTESIAN_POINT ( 'NONE',  ( 114.7192077545248594, -7.250697342233347165, -7.631215200338321125 ) ) ;
#27575 = CARTESIAN_POINT ( 'NONE',  ( -13.56828337869107948, -4.779084862085587915, -8.893215200338321580 ) ) ;
#27576 = DIRECTION ( 'NONE',  ( -1.000000000000000000, 0.000000000000000000, 0.000000000000000000 ) ) ;
#27577 = CARTESIAN_POINT ( 'NONE',  ( 112.9097148109120070, -9.565557343593413364, -10.61323700422348004 ) ) ;
#27578 = CARTESIAN_POINT ( 'NONE',  ( 78.01081489496232280, -57.59294529755612757, -1.022260109403890782 ) ) ;
#27579 = CARTESIAN_POINT ( 'NONE',  ( 117.4478481442453131, -9.565557343593413364, -10.61323700422348004 ) ) ;
#27580 = CARTESIAN_POINT ( 'NONE',  ( 120.4020503192116820, -2.378957183258601393, -17.95140958770220152 ) ) ;
#27581 = CARTESIAN_POINT ( 'NONE',  ( 117.4478481442453131, -9.565557343593413364, -10.61323700422348004 ) ) ;
#27582 = FACE_OUTER_BOUND ( 'NONE', #23088, .T. ) ;
#27583 = B_SPLINE_CURVE_WITH_KNOTS ( 'NONE', 3,
 ( #9002, #36342, #5347, #16300, #23138, #19483, #43436, #22674, #4890, #19706, #19263, #44120, #33143, #8549, #1915, #36120, #25878, #15845, #43651, #2136 ),
 .UNSPECIFIED., .F., .F.,
 ( 4, 2, 2, 2, 2, 2, 2, 2, 2, 4 ),
 ( 0.000000000000000000, 0.2500000000000117129, 0.3750000000000175415, 0.5000000000000234257, 0.5625000000000199840, 0.6250000000000166533, 0.7500000000000097700, 0.8125000000000064393, 0.8750000000000031086, 1.000000000000000000 ),
 .UNSPECIFIED. ) ;
#27584 = CARTESIAN_POINT ( 'NONE',  ( 115.0086014775786509, -5.574606645277164318, -18.38911715685844683 ) ) ;
#27585 = EDGE_CURVE ( 'NONE', #7925, #30998, #13863, .T. ) ;
#27586 = CARTESIAN_POINT ( 'NONE',  ( 90.72400676789006013, -25.99489077589524300, -13.39321520033831625 ) ) ;
#27587 = CARTESIAN_POINT ( 'NONE',  ( 114.8384214775786489, 0.9020085738987339008, -11.91225656197089222 ) ) ;
#27588 = CARTESIAN_POINT ( 'NONE',  ( 111.6617281442453304, 0.4262465694468514643, -12.03445270309931736 ) ) ;
#27589 = ADVANCED_FACE ( 'NONE', ( #17315 ), #13883, .F. ) ;
#27590 = EDGE_CURVE ( 'NONE', #15883, #2745, #14221, .T. ) ;
#27591 = CARTESIAN_POINT ( 'NONE',  ( 115.3489614775786407, -0.8288870151387760510, -10.36305467784173118 ) ) ;
#27592 = ORIENTED_EDGE ( 'NONE', *, *, #4467, .F. ) ;
#27593 = CARTESIAN_POINT ( 'NONE',  ( 118.1852948109119836, -5.638512984488999180, -18.83840828888717311 ) ) ;
#27594 = CARTESIAN_POINT ( 'NONE',  ( 106.2459265045248173, -7.250697342233347165, -19.15521520033831138 ) ) ;
#27595 = CARTESIAN_POINT ( 'NONE',  ( 106.8015515045248378, -6.936859964151250502, -18.39754474579286025 ) ) ;
#27596 = CARTESIAN_POINT ( 'NONE',  ( 105.8292077545248446, -2.791137627527939813, -18.39754474579286025 ) ) ;
#27597 = CARTESIAN_POINT ( 'NONE',  ( 113.4920311052981816, 0.4930828106259610433, -12.14321520033829849 ) ) ;
#27598 = CARTESIAN_POINT ( 'NONE',  ( 122.8368814775786291, -1.561330072975668948, -17.79121239304076951 ) ) ;
#27599 = ORIENTED_EDGE ( 'NONE', *, *, #18923, .F. ) ;
#27600 = DIRECTION ( 'NONE',  ( -0.000000000000000000, -0.9284778069183720062, -0.3713878862591650232 ) ) ;
#27601 = CARTESIAN_POINT ( 'NONE',  ( 116.4834948109119779, -7.894159318335828068, -9.358103419637847864 ) ) ;
#27602 = CARTESIAN_POINT ( 'NONE',  ( 123.7022829359119811, -4.283928203966204329, -7.183505701512929775 ) ) ;
#27603 = CARTESIAN_POINT ( 'NONE',  ( 123.1772414775786189, -4.089484607189486809, -7.948022111789456723 ) ) ;
#27604 = CARTESIAN_POINT ( 'NONE',  ( 105.5513952545248060, 0.8980012041604421569, -11.00651665394454071 ) ) ;
#27605 = CARTESIAN_POINT ( 'NONE',  ( 89.16143781654311340, -10.35449676759526305, -14.03636009902034409 ) ) ;
#27606 = VERTEX_POINT ( 'NONE', #31204 ) ;
#27607 = CARTESIAN_POINT ( 'NONE',  ( 112.2289948109119848, -1.834011780172310813, -8.268836392978581529 ) ) ;
#27608 = CARTESIAN_POINT ( 'NONE',  ( 112.1155414775786454, 0.9020085738987339008, -11.91225656197089222 ) ) ;
#27609 = CARTESIAN_POINT ( 'NONE',  ( 123.2339681442453241, -6.344957434206665248, -7.627207830600338134 ) ) ;
#27610 = CARTESIAN_POINT ( 'NONE',  ( 117.7314814775786260, -5.574606645277164318, -18.38911715685844683 ) ) ;
#27611 = CARTESIAN_POINT ( 'NONE',  ( 82.66491059565053945, -31.44298744622023989, -22.15403020929251454 ) ) ;
#27612 = CARTESIAN_POINT ( 'NONE',  ( 118.9227414775786400, -10.63000616557722466, -14.87417383870573495 ) ) ;
#27613 = DIRECTION ( 'NONE',  ( 0.000000000000000000, 0.000000000000000000, 1.000000000000000000 ) ) ;
#27614 = B_SPLINE_CURVE_WITH_KNOTS ( 'NONE', 3,
 ( #19234, #32451, #29045, #12631, #36986, #33336, #43859, #39753, #43626, #9199 ),
 .UNSPECIFIED., .F., .F.,
 ( 4, 3, 3, 4 ),
 ( 3.127317220692749988E-18, 0.0002476486808869849754, 0.0004952973797228679611, 0.0009539399846111509687 ),
 .UNSPECIFIED. ) ;
#27615 = CARTESIAN_POINT ( 'NONE',  ( 123.2339681442453241, -3.505236298600246325, -18.68346056562440793 ) ) ;
#27616 = EDGE_LOOP ( 'NONE', ( #41758, #25063, #18123, #33800, #20338 ) ) ;
#27617 = CARTESIAN_POINT ( 'NONE',  ( 74.66232006577804725, -2.500611837642884527, -18.64321520033831803 ) ) ;
#27618 = CARTESIAN_POINT ( 'NONE',  ( 115.5758681442453053, -1.561330072975668060, -17.79121239304076951 ) ) ;
#27619 = CARTESIAN_POINT ( 'NONE',  ( 124.3117748109119844, 0.1319031606808879209, -14.10382304977623669 ) ) ;
#27620 = ORIENTED_EDGE ( 'NONE', *, *, #4845, .F. ) ;
#27621 = CARTESIAN_POINT ( 'NONE',  ( 122.6604860609119640, -6.564341423271550902, -7.887810678476487425 ) ) ;
#27622 = CARTESIAN_POINT ( 'NONE',  ( 136.7860375664297408, -1.264623415989550859, -9.101478292670408976 ) ) ;
#27623 = CARTESIAN_POINT ( 'NONE',  ( 120.6245414775786458, -9.988377603198976828, -10.36322818467138340 ) ) ;
#27624 = CARTESIAN_POINT ( 'NONE',  ( 109.4407702545248355, -10.62599879583958717, -15.77991374673208469 ) ) ;
#27625 = CARTESIAN_POINT ( 'NONE',  ( 118.5823814775786360, -7.643976991954077427, -18.09477374809248928 ) ) ;
#27626 = VERTEX_POINT ( 'NONE', #6825 ) ;
#27627 = ORIENTED_EDGE ( 'NONE', *, *, #5222, .T. ) ;
#27628 = CARTESIAN_POINT ( 'NONE',  ( 113.0231681442453322, 0.9020085738987339008, -11.91225656197089222 ) ) ;
#27629 = CIRCLE ( 'NONE', #7947, 2.000000000000000444 ) ;
#27630 = CARTESIAN_POINT ( 'NONE',  ( 123.5743281442453139, -2.084020599724406786, -8.691656652584148546 ) ) ;
#27631 = CIRCLE ( 'NONE', #29072, 2.000000000000000444 ) ;
#27632 = LINE ( 'NONE', #13502, #15659 ) ;
#27633 = EDGE_CURVE ( 'NONE', #5895, #37436, #2921, .T. ) ;
#27634 = DIRECTION ( 'NONE',  ( -0.000000000000000000, -0.9284778069183718952, -0.3713878862591649677 ) ) ;
#27635 = CARTESIAN_POINT ( 'NONE',  ( 123.4041481442452834, -10.30919188438810075, -12.61870101168855918 ) ) ;
#27636 = CARTESIAN_POINT ( 'NONE',  ( 73.07463722459043254, -53.85408697697087632, -33.84994832705423562 ) ) ;
#27637 = DIRECTION ( 'NONE',  ( 0.000000000000000000, 0.000000000000000000, -1.000000000000000000 ) ) ;
#27638 = CARTESIAN_POINT ( 'NONE',  ( 118.9794681442453026, -9.261995988541697145, -16.69588392320189030 ) ) ;
#27640 = CARTESIAN_POINT ( 'NONE',  ( 118.4122014775786340, -9.859900752359374465, -12.68260735090039404 ) ) ;
#27639 = CARTESIAN_POINT ( 'NONE',  ( 117.7314814775786260, -4.089484607189486809, -7.948022111789456723 ) ) ;
#27641 =( BOUNDED_CURVE ( )  B_SPLINE_CURVE ( 2, ( #21462, #42443, #34512, #41395, #10148, #9925, #44808, #37494, #31712, #37725, #20411, #6496, #34295, #3068, #35344, #24882, #13565 ),
 .UNSPECIFIED., .F., .T. ) 
 B_SPLINE_CURVE_WITH_KNOTS ( ( 3, 2, 2, 2, 2, 2, 2, 2, 3 ),
 ( 0.3035091206787220441, 0.3125000000000000000, 0.3250000000000000111, 0.3375000000000000222, 0.3499999999999999778, 0.3624999999999999889, 0.3750000000000000000, 0.3875000000000000111, 0.3964908793212780225 ),
 .UNSPECIFIED. ) 
 CURVE ( )  GEOMETRIC_REPRESENTATION_ITEM ( )  RATIONAL_B_SPLINE_CURVE ( ( 0.9692594319298230010, 0.9452488050343769155, 1.000000000000000000, 0.9238795325112869605, 1.000000000000000000, 0.9238795325112869605, 1.000000000000000000, 0.9238795325112869605, 1.000000000000000000, 0.9238795325112869605, 1.000000000000000000, 0.9238795325112869605, 1.000000000000000000, 0.9238795325112869605, 1.000000000000000000, 0.9452488050343769155, 0.9692594319298220018 ) ) 
 REPRESENTATION_ITEM ( '' )  );
#27642 = CARTESIAN_POINT ( 'NONE',  ( 125.1733191598100916, -1.295815253274133383, -16.89579513612386563 ) ) ;
#27643 = CARTESIAN_POINT ( 'NONE',  ( 114.8384214775786489, 0.9020085738987339008, -11.91225656197089222 ) ) ;
#27644 = VERTEX_POINT ( 'NONE', #34610 ) ;
#27645 = CARTESIAN_POINT ( 'NONE',  ( 111.8886348109120092, -3.383040157471821630, -19.15922257007629170 ) ) ;
#27646 = CARTESIAN_POINT ( 'NONE',  ( 125.5030348109119842, -6.222761293079280165, -8.102969835052485692 ) ) ;
#27647 = CARTESIAN_POINT ( 'NONE',  ( 109.0240515045248202, -2.477300249445798297, -7.631215200338321125 ) ) ;
#27648 = CARTESIAN_POINT ( 'NONE',  ( 109.5796765045248122, -2.791137627527939813, -8.388885654883777576 ) ) ;
#27649 = CARTESIAN_POINT ( 'NONE',  ( 106.7320983795247855, -0.7896495226426338832, -9.318865927141430916 ) ) ;
#27650 = CARTESIAN_POINT ( 'NONE',  ( 123.0070614775786169, 0.9020085738987339008, -11.91225656197089222 ) ) ;
#27651 = CARTESIAN_POINT ( 'NONE',  ( 112.0588148109119828, 0.5811942927096154232, -14.16772938898807155 ) ) ;
#27652 = VERTEX_POINT ( 'NONE', #3607 ) ;
#27653 = CARTESIAN_POINT ( 'NONE',  ( 126.1270281442452870, -10.30919188438810075, -12.61870101168855918 ) ) ;
#27654 = CARTESIAN_POINT ( 'NONE',  ( 109.7880358795247986, -0.7896495226426338832, -17.46756447353520159 ) ) ;
#27655 = CARTESIAN_POINT ( 'NONE',  ( 70.19189222814998175, -55.40259354030312267, -35.36385344588251911 ) ) ;
#27656 = ADVANCED_FACE ( 'NONE', ( #16639 ), #18306, .T. ) ;
#27657 = CARTESIAN_POINT ( 'NONE',  ( 122.5532481442453019, -10.63000616557722466, -14.87417383870573495 ) ) ;
#27658 = CARTESIAN_POINT ( 'NONE',  ( 123.5743281442453139, -7.893985811506177619, -18.51759400769804742 ) ) ;
#27659 = CARTESIAN_POINT ( 'NONE',  ( 31.16856251326852956, -20.50830283073288385, -19.39321520033831447 ) ) ;
#27660 = CARTESIAN_POINT ( 'NONE',  ( 126.6375681442452930, -10.15424416112533912, -14.75197769757731336 ) ) ;
#27661 = CARTESIAN_POINT ( 'NONE',  ( 70.19189222814998175, -100.0979043305785581, -53.24182196210380624 ) ) ;
#27662 = CARTESIAN_POINT ( 'NONE',  ( 106.1070202545248407, -10.62599879583958717, -15.77991374673208469 ) ) ;
#27663 = ORIENTED_EDGE ( 'NONE', *, *, #16129, .F. ) ;
#27664 = CYLINDRICAL_SURFACE ( 'NONE', #465, 4.500000000000003553 ) ;
#27665 = CARTESIAN_POINT ( 'NONE',  ( 114.4980614775786734, -2.084020599724406786, -8.691656652584148546 ) ) ;
#27666 = CARTESIAN_POINT ( 'NONE',  ( 126.1837548109119496, 0.4262465694468514643, -12.03445270309931736 ) ) ;
#27667 = AXIS2_PLACEMENT_3D ( 'NONE', #17902, #42969, #3757 ) ;
#27668 = CARTESIAN_POINT ( 'NONE',  ( 115.8999108795247821, -8.938348069036489818, -9.318865927141430916 ) ) ;
#27669 = CARTESIAN_POINT ( 'NONE',  ( 108.1211608795247798, -1.325403438956436419, -16.93181055722141792 ) ) ;
#27670 = CARTESIAN_POINT ( 'NONE',  ( 120.8514481442452961, -2.084020599724406786, -8.691656652584148546 ) ) ;
#27671 = CARTESIAN_POINT ( 'NONE',  ( 116.2565881442453133, -0.8288870151387760510, -10.36305467784173118 ) ) ;
#27672 = CARTESIAN_POINT ( 'NONE',  ( 126.0135748109119902, -8.166667518702819706, -8.995218007635861213 ) ) ;
#27673 = VERTEX_POINT ( 'NONE', #20592 ) ;
#27674 = CARTESIAN_POINT ( 'NONE',  ( 120.5074391859119913, -1.406689858478933353, -17.56299727309130887 ) ) ;
#27675 = CARTESIAN_POINT ( 'NONE',  ( 117.4478481442453131, 0.2603800115204892296, -16.42320221600525088 ) ) ;
#27676 = CIRCLE ( 'NONE', #43777, 2.445500000000004448 ) ;
#27677 = CARTESIAN_POINT ( 'NONE',  ( 88.35093386163799778, -25.23119213852205789, -15.24166438581092109 ) ) ;
#27678 = CARTESIAN_POINT ( 'NONE',  ( 113.2500748109119968, -3.505236298600246325, -18.68346056562440793 ) ) ;
#27679 = ORIENTED_EDGE ( 'NONE', *, *, #14610, .T. ) ;
#27680 = CIRCLE ( 'NONE', #11643, 2.200000000000001066 ) ;
#27681 = CARTESIAN_POINT ( 'NONE',  ( 73.07463722459043254, -52.92560917005250332, -33.47856044079506432 ) ) ;
#27682 = EDGE_LOOP ( 'NONE', ( #16729, #24933, #16453, #12991 ) ) ;
#27683 = CARTESIAN_POINT ( 'NONE',  ( 119.1496481442453046, -6.222761293078241884, -8.102969835052219238 ) ) ;
#27684 = CARTESIAN_POINT ( 'NONE',  ( 113.3635281442453504, -0.1624402480850797581, -16.17319339645315424 ) ) ;
#27685 = CARTESIAN_POINT ( 'NONE',  ( 117.8239502440515452, -2.467220198592778413, -17.83387418641524391 ) ) ;
#27686 = CARTESIAN_POINT ( 'NONE',  ( 123.2855641859119942, -8.321307733199551748, -9.223433127585318303 ) ) ;
#27687 = ORIENTED_EDGE ( 'NONE', *, *, #22969, .T. ) ;
#27688 = CARTESIAN_POINT ( 'NONE',  ( 96.54708369096698561, -26.33989114581222424, -11.20947992683166916 ) ) ;
#27689 = CARTESIAN_POINT ( 'NONE',  ( 125.1375072647509228, 2.456438219714048188, -12.13603346852097786 ) ) ;
#27690 = CARTESIAN_POINT ( 'NONE',  ( 113.5385046295247804, -4.863998795839590272, -7.631215200338315796 ) ) ;
#27691 = AXIS2_PLACEMENT_3D ( 'NONE', #23504, #13467, #33966 ) ;
#27692 = CARTESIAN_POINT ( 'NONE',  ( 115.9456797178594343, -0.3595008806742178709, -15.96590799893915857 ) ) ;
#27693 = CARTESIAN_POINT ( 'NONE',  ( 122.4965214775786251, 0.1319031606808879209, -14.10382304977623669 ) ) ;
#27694 = CARTESIAN_POINT ( 'NONE',  ( 118.4689281442453250, -10.15424416112533912, -14.75197769757731336 ) ) ;
#27695 = CARTESIAN_POINT ( 'NONE',  ( 119.8983769549021758, -1.135392229370309369, -17.10942237759952889 ) ) ;
#27696 = ORIENTED_EDGE ( 'NONE', *, *, #16701, .T. ) ;
#27697 = DIRECTION ( 'NONE',  ( 0.000000000000000000, 0.9284778069183721172, 0.3713878862591650232 ) ) ;
#27698 = CARTESIAN_POINT ( 'NONE',  ( 115.6893214775786447, -9.859900752359374465, -12.68260735090039404 ) ) ;
#27699 = VECTOR ( 'NONE', #13446, 1000.000000000000000 ) ;
#27700 = CARTESIAN_POINT ( 'NONE',  ( 125.1418709397587037, -1.276798789163246850, -16.92111840127481059 ) ) ;
#27701 = CARTESIAN_POINT ( 'NONE',  ( 86.75477599865929790, -25.99489077589524300, -13.39321520033831625 ) ) ;
#27702 = ADVANCED_FACE ( 'NONE', ( #10550, #38339 ), #34468, .T. ) ;
#27703 = CARTESIAN_POINT ( 'NONE',  ( 111.7751814775786556, -7.893985811506177619, -18.51759400769804742 ) ) ;
#27704 = ORIENTED_EDGE ( 'NONE', *, *, #1616, .T. ) ;
#27705 = AXIS2_PLACEMENT_3D ( 'NONE', #19430, #9175, #10527 ) ;
#27706 = CARTESIAN_POINT ( 'NONE',  ( 113.7606148109119886, -1.561330072975668060, -17.79121239304076596 ) ) ;
#27707 = CARTESIAN_POINT ( 'NONE',  ( 126.4750299824214324, 0.09325604387533485695, -14.70660372723753895 ) ) ;
#27708 = CARTESIAN_POINT ( 'NONE',  ( 106.8015515045248378, -6.936859964151250502, -18.39754474579286025 ) ) ;
#27709 = CARTESIAN_POINT ( 'NONE',  ( 112.4559014775786494, -9.988377603198976828, -10.36322818467138340 ) ) ;
#27710 = CARTESIAN_POINT ( 'NONE',  ( 115.5758681442453053, -1.561330072975668060, -17.79121239304076951 ) ) ;
#27711 = CARTESIAN_POINT ( 'NONE',  ( 125.1059481442452750, -1.833838273342660141, -17.42832698103878286 ) ) ;
#27712 = DIRECTION ( 'NONE',  ( -1.000000000000000000, 0.000000000000000000, -0.000000000000000000 ) ) ;
#27713 = CARTESIAN_POINT ( 'NONE',  ( 110.9687390045248350, -9.868328341294098749, -11.32035403202665869 ) ) ;
#27714 = CARTESIAN_POINT ( 'NONE',  ( 120.1332064091100733, -0.9924539043446216624, -17.29976612834909133 ) ) ;
#27715 = CARTESIAN_POINT ( 'NONE',  ( 88.19154317003298615, -15.02898452507898241, -8.143215200338314474 ) ) ;
#27716 = CARTESIAN_POINT ( 'NONE',  ( 117.4478481442453131, -9.565557343593413364, -10.61323700422348004 ) ) ;
#27717 = CARTESIAN_POINT ( 'NONE',  ( 107.6349890045248401, 0.8980012041604421569, -15.77991374673208469 ) ) ;
#27718 = DIRECTION ( 'NONE',  ( 0.000000000000000000, -0.3818493186865936084, 0.9242245927363024194 ) ) ;
#27719 = CARTESIAN_POINT ( 'NONE',  ( 111.1770983795247787, -0.7896495226426338832, -9.318865927141430916 ) ) ;
#27720 = CARTESIAN_POINT ( 'NONE',  ( 126.0703014775786102, -9.988377603198980381, -10.36322818467138518 ) ) ;
#27721 = CARTESIAN_POINT ( 'NONE',  ( 126.0135748109119902, -8.166667518702819706, -8.995218007635861213 ) ) ;
#27722 = DIRECTION ( 'NONE',  ( -0.2768435750659241079, -0.3568721902840686355, 0.8921882507333134260 ) ) ;
#27723 = CARTESIAN_POINT ( 'NONE',  ( 118.9794681442453026, -9.261995988541697145, -16.69588392320189030 ) ) ;
#27724 = CARTESIAN_POINT ( 'NONE',  ( 117.7314814775786260, -4.089484607189486809, -7.948022111789456723 ) ) ;
#27725 = ORIENTED_EDGE ( 'NONE', *, *, #14445, .T. ) ;
#27726 = CARTESIAN_POINT ( 'NONE',  ( 113.8740681442453138, -9.859900752359374465, -12.68260735090039404 ) ) ;
#27727 = CARTESIAN_POINT ( 'NONE',  ( 125.3328548109119964, -9.261995988541697145, -16.69588392320189030 ) ) ;
#27729 = EDGE_CURVE ( 'NONE', #2582, #23986, #12044, .T. ) ;
#27728 = CARTESIAN_POINT ( 'NONE',  ( 112.5126281442453120, -10.30919188438810075, -12.61870101168855918 ) ) ;
#27730 =( BOUNDED_CURVE ( )  B_SPLINE_CURVE ( 3, ( #11401, #11619, #25309, #15041 ),
 .UNSPECIFIED., .F., .T. ) 
 B_SPLINE_CURVE_WITH_KNOTS ( ( 4, 4 ),
 ( 1.570796326794895004, 2.173987732404564888 ),
 .UNSPECIFIED. ) 
 CURVE ( )  GEOMETRIC_REPRESENTATION_ITEM ( )  RATIONAL_B_SPLINE_CURVE ( ( 1.000000000000000000, 0.9699091404214869039, 0.9699091404214869039, 1.000000000000000000 ) ) 
 REPRESENTATION_ITEM ( '' )  );
#27731 = CARTESIAN_POINT ( 'NONE',  ( 115.4056881442453459, -2.084020599724406786, -8.691656652584148546 ) ) ;
#27732 = ORIENTED_EDGE ( 'NONE', *, *, #43865, .T. ) ;
#27733 = CARTESIAN_POINT ( 'NONE',  ( 120.5678148109119832, -1.833838273342659253, -17.42832698103878286 ) ) ;
#27734 = AXIS2_PLACEMENT_3D ( 'NONE', #7625, #28614, #3751 ) ;
#27735 = CARTESIAN_POINT ( 'NONE',  ( 117.7882081442453170, -6.344957434206665248, -7.627207830600338134 ) ) ;
#27736 = CARTESIAN_POINT ( 'NONE',  ( 123.6808719482204992, -5.999156839134923480, -18.26265215102791117 ) ) ;
#27737 = CARTESIAN_POINT ( 'NONE',  ( 114.1635827545248389, -2.477300249445798297, -19.15521520033831138 ) ) ;
#27738 = ORIENTED_EDGE ( 'NONE', *, *, #11170, .T. ) ;
#27739 = AXIS2_PLACEMENT_3D ( 'NONE', #5009, #39903, #33264 ) ;
#27740 = DIRECTION ( 'NONE',  ( -0.9970811988817437355, 0.07634843047859309062, 0.000000000000000000 ) ) ;
#27741 = CARTESIAN_POINT ( 'NONE',  ( 125.3895814775786448, -7.893985811506177619, -18.51759400769804742 ) ) ;
#27742 = CARTESIAN_POINT ( 'NONE',  ( 123.9584548109119737, -4.863998795839242995, -13.39321520033831447 ) ) ;
#27743 = CARTESIAN_POINT ( 'NONE',  ( 114.2144281442453178, -8.166667518702817929, -8.995218007635859436 ) ) ;
#27744 = DIRECTION ( 'NONE',  ( -0.9908103287288504424, 0.1352586133457951423, 0.000000000000000000 ) ) ;
#27745 = CARTESIAN_POINT ( 'NONE',  ( 113.3068014775786594, -1.833838273342658809, -17.42832698103878286 ) ) ;
#27746 = CARTESIAN_POINT ( 'NONE',  ( 62.79269271256460172, -12.56645042133913392, -16.65519758901568181 ) ) ;
#27747 = FACE_OUTER_BOUND ( 'NONE', #23297, .T. ) ;
#27748 = CARTESIAN_POINT ( 'NONE',  ( 114.3024890045248156, -9.868328341294098749, -11.32035403202665869 ) ) ;
#27749 = CARTESIAN_POINT ( 'NONE',  ( 117.9583881442453048, -10.30919188438810075, -12.61870101168855918 ) ) ;
#27750 = CARTESIAN_POINT ( 'NONE',  ( 136.8445491832674463, -6.866345705054112791, -18.59485542995252771 ) ) ;
#27751 = AXIS2_PLACEMENT_3D ( 'NONE', #4867, #8077, #29046 ) ;
#27752 = FACE_OUTER_BOUND ( 'NONE', #36579, .T. ) ;
#27753 = DIRECTION ( 'NONE',  ( 0.000000000000000000, -0.4669533266896290225, -0.8842819633428516957 ) ) ;
#27754 = CARTESIAN_POINT ( 'NONE',  ( 120.5110881442453206, -3.505236298600246325, -18.68346056562440793 ) ) ;
#27755 = ORIENTED_EDGE ( 'NONE', *, *, #20936, .F. ) ;
#27756 = CARTESIAN_POINT ( 'NONE',  ( 126.1837548109119211, -10.63000616557722466, -14.87417383870573495 ) ) ;
#27757 = CARTESIAN_POINT ( 'NONE',  ( 118.0151148109119816, -10.63000616557722466, -14.87417383870573495 ) ) ;
#27758 = FACE_OUTER_BOUND ( 'NONE', #17218, .T. ) ;
#27759 = CARTESIAN_POINT ( 'NONE',  ( 117.3911214775786505, -7.894159318335828068, -9.358103419637847864 ) ) ;
#27760 = CARTESIAN_POINT ( 'NONE',  ( 113.7606148109119886, -7.894159318335828068, -9.358103419637847864 ) ) ;
#27761 = CARTESIAN_POINT ( 'NONE',  ( 105.5513952545248060, -9.868328341294098749, -15.46607636864997204 ) ) ;
#27762 = CARTESIAN_POINT ( 'NONE',  ( 111.5938171295247940, -10.62599879583958540, -13.39321520033831447 ) ) ;
#27763 = CARTESIAN_POINT ( 'NONE',  ( 119.6034614775786196, -3.505236298600246325, -18.68346056562440793 ) ) ;
#27764 = CARTESIAN_POINT ( 'NONE',  ( 119.7169148109119874, -0.1624402480850797581, -16.17319339645315424 ) ) ;
#27765 = CARTESIAN_POINT ( 'NONE',  ( 116.5944421295247793, -4.863998795839590272, -13.39321520033831447 ) ) ;
#27766 = FACE_OUTER_BOUND ( 'NONE', #7067, .T. ) ;
#27767 = CARTESIAN_POINT ( 'NONE',  ( 107.5655358795247736, -8.402594152722688392, -9.854619843455216355 ) ) ;
#27768 = AXIS2_PLACEMENT_3D ( 'NONE', #43735, #12280, #16144 ) ;
#27769 = DIRECTION ( 'NONE',  ( 1.000000000000000000, 0.000000000000000000, 0.000000000000000000 ) ) ;
#27770 = CARTESIAN_POINT ( 'NONE',  ( 113.1366214775786432, -1.834011780172310813, -8.268836392978581529 ) ) ;
#27771 = CARTESIAN_POINT ( 'NONE',  ( 114.3278814775786429, -10.30919188438810075, -12.61870101168855918 ) ) ;
#27772 = CARTESIAN_POINT ( 'NONE',  ( 122.1048610609119720, -6.340755971794695078, -8.611740276972781771 ) ) ;
#27773 = VERTEX_POINT ( 'NONE', #4583 ) ;
#27774 = CARTESIAN_POINT ( 'NONE',  ( 113.5385046295247804, -4.863998795839590272, -7.631215200338315796 ) ) ;
#27775 = ORIENTED_EDGE ( 'NONE', *, *, #2542, .F. ) ;
#27776 = CARTESIAN_POINT ( 'NONE',  ( 122.3263414775786373, -6.344957434206665248, -7.627207830600338134 ) ) ;
#27777 = CARTESIAN_POINT ( 'NONE',  ( 111.8886348109120092, -3.383040157471821630, -19.15922257007629170 ) ) ;
#27778 = CARTESIAN_POINT ( 'NONE',  ( 119.1496481442453046, -6.222761293078241884, -8.102969835052219238 ) ) ;
#27779 = CARTESIAN_POINT ( 'NONE',  ( 121.3619881442452879, -4.089484607189486809, -7.948022111789456723 ) ) ;
#27780 = CARTESIAN_POINT ( 'NONE',  ( 118.9794681442453026, -9.261995988541697145, -16.69588392320189030 ) ) ;
#27781 = CARTESIAN_POINT ( 'NONE',  ( 106.5237390045248418, -9.868328341294098749, -11.32035403202665869 ) ) ;
#27782 = CARTESIAN_POINT ( 'NONE',  ( 126.1837548109119211, -10.63000616557722466, -14.87417383870573495 ) ) ;
#27783 = DIRECTION ( 'NONE',  ( 0.000000000000000000, 0.000000000000000000, -1.000000000000000000 ) ) ;
#27784 = ORIENTED_EDGE ( 'NONE', *, *, #39061, .T. ) ;
#27785 = CARTESIAN_POINT ( 'NONE',  ( 119.2631014775786298, 0.2603800115204892296, -16.42320221600525088 ) ) ;
#27786 = ADVANCED_FACE ( 'NONE', ( #25792 ), #18729, .T. ) ;
#27787 = CARTESIAN_POINT ( 'NONE',  ( 120.4379860609119675, -6.564341423271550902, -7.887810678476487425 ) ) ;
#27788 = CARTESIAN_POINT ( 'NONE',  ( 115.8027748109119841, -0.4660016031367893996, -10.09054647747474043 ) ) ;
#27789 = ORIENTED_EDGE ( 'NONE', *, *, #13360, .F. ) ;
#27790 = CARTESIAN_POINT ( 'NONE',  ( 113.9552233795247815, -8.938348069036489818, -17.46756447353520159 ) ) ;
#27791 = AXIS2_PLACEMENT_3D ( 'NONE', #44710, #5930, #34411 ) ;
#27792 = CARTESIAN_POINT ( 'NONE',  ( -13.78505786741674655, -3.796669018538534779, -8.660771829302781555 ) ) ;
#27793 = CARTESIAN_POINT ( 'NONE',  ( 120.0947965460471920, -2.191907684172563986, -18.20049396185734025 ) ) ;
#27794 = CARTESIAN_POINT ( 'NONE',  ( 125.4348241020431800, -6.339323288574539639, -18.90683442488884936 ) ) ;
#27795 = DIRECTION ( 'NONE',  ( -1.000000000000000000, 0.000000000000000000, -0.000000000000000000 ) ) ;
#27796 = CARTESIAN_POINT ( 'NONE',  ( 119.7736414775786358, 0.1319031606808879209, -14.10382304977623669 ) ) ;
#27797 = CARTESIAN_POINT ( 'NONE',  ( 9.052690036452151645, -4.182915634381243919, -17.89321520033831447 ) ) ;
#27798 = CARTESIAN_POINT ( 'NONE',  ( 116.1431348109119881, 0.1319031606808879209, -14.10382304977623669 ) ) ;
#27799 = FACE_OUTER_BOUND ( 'NONE', #34190, .T. ) ;
#27800 = CARTESIAN_POINT ( 'NONE',  ( 120.7379948109119709, 0.4262465694468514643, -12.03445270309931736 ) ) ;
#27801 = CARTESIAN_POINT ( 'NONE',  ( 123.3550173109119612, 0.2312338769422704887, -16.08380026872395874 ) ) ;
#27802 = CARTESIAN_POINT ( 'NONE',  ( 115.8027748109119841, -0.4660016031367893996, -10.09054647747474043 ) ) ;
#27803 = CARTESIAN_POINT ( 'NONE',  ( 116.0296814775786345, -1.833838273342658809, -17.42832698103878286 ) ) ;
#27804 = ORIENTED_EDGE ( 'NONE', *, *, #23359, .F. ) ;
#27805 = CARTESIAN_POINT ( 'NONE',  ( 118.6391081442452986, -4.089484607189486809, -7.948022111789456723 ) ) ;
#27806 = CARTESIAN_POINT ( 'NONE',  ( 106.7320983795247855, -0.7896495226426338832, -9.318865927141430916 ) ) ;
#27807 = EDGE_CURVE ( 'NONE', #42996, #23812, #11447, .T. ) ;
#27808 = CARTESIAN_POINT ( 'NONE',  ( 115.6325948109119821, -9.565557343593402706, -10.61323700422346228 ) ) ;
#27809 = CARTESIAN_POINT ( 'NONE',  ( 105.6208483795248299, -8.402594152722688392, -16.93181055722141792 ) ) ;
#27810 = CIRCLE ( 'NONE', #8151, 2.000000000000001776 ) ;
#27811 = CARTESIAN_POINT ( 'NONE',  ( 123.4124213555256517, -8.364211927971188842, -17.30190421972978143 ) ) ;
#27812 = CARTESIAN_POINT ( 'NONE',  ( 122.9503348109119827, 0.5811942927096110934, -14.16772938898807510 ) ) ;
#27813 = ORIENTED_EDGE ( 'NONE', *, *, #16520, .T. ) ;
#27814 = CARTESIAN_POINT ( 'NONE',  ( 127.2313854076961803, -9.032957600002841758, -9.795810222955712021 ) ) ;
#27815 = CARTESIAN_POINT ( 'NONE',  ( 116.9940348109119839, -0.1624402480850797581, -16.17319339645315424 ) ) ;
#27816 = ADVANCED_FACE ( 'NONE', ( #43973 ), #9313, .F. ) ;
#27817 = CARTESIAN_POINT ( 'NONE',  ( 70.19189222814998175, -67.83330054016514055, -40.33609291459782753 ) ) ;
#27818 = DIRECTION ( 'NONE',  ( -1.156482317317869950E-15, -1.000000000000000000, 0.000000000000000000 ) ) ;
#27819 = CARTESIAN_POINT ( 'NONE',  ( 123.9714148109119805, -0.4660016031367893996, -10.09054647747474043 ) ) ;
#27820 = EDGE_CURVE ( 'NONE', #28126, #6217, #11920, .T. ) ;
#27821 = CARTESIAN_POINT ( 'NONE',  ( 111.2465515045248168, -6.936859964151250502, -18.39754474579286025 ) ) ;
#27822 = CARTESIAN_POINT ( 'NONE',  ( 117.2294421295247844, -10.76310523276723785, -21.89255013987451548 ) ) ;
#27823 = ORIENTED_EDGE ( 'NONE', *, *, #35587, .F. ) ;
#27824 = CARTESIAN_POINT ( 'NONE',  ( 113.2500748109119968, -6.344957434206662583, -7.627207830600332805 ) ) ;
#27825 = CIRCLE ( 'NONE', #17631, 1.500000000000001332 ) ;
#27826 = CARTESIAN_POINT ( 'NONE',  ( 124.8790414775786246, -8.899110576539710493, -16.42337572283490132 ) ) ;
#27827 = CARTESIAN_POINT ( 'NONE',  ( 121.8725281442453223, -3.383040157471821630, -19.15922257007629170 ) ) ;
#27828 = CARTESIAN_POINT ( 'NONE',  ( 116.2565881442453133, -0.8288870151387760510, -10.36305467784173118 ) ) ;
#27829 = CARTESIAN_POINT ( 'NONE',  ( 72.54180985774836188, -56.94300424148091366, -35.25083934068751290 ) ) ;
#27830 = CARTESIAN_POINT ( 'NONE',  ( 119.8303681442453126, -10.63000616557722466, -14.87417383870573495 ) ) ;
#27831 = CARTESIAN_POINT ( 'NONE',  ( 112.7491510812576934, -0.01829820670803256055, -12.14321520033831625 ) ) ;
#27832 = CARTESIAN_POINT ( 'NONE',  ( 122.5532481442453019, 0.4262465694468514643, -12.03445270309931736 ) ) ;
#27833 = ORIENTED_EDGE ( 'NONE', *, *, #23542, .F. ) ;
#27834 = ADVANCED_FACE ( 'NONE', ( #36039 ), #7303, .T. ) ;
#27835 = CARTESIAN_POINT ( 'NONE',  ( 116.5946626450759851, -9.863530430156441042, -13.31021735937817851 ) ) ;
#27836 = CARTESIAN_POINT ( 'NONE',  ( 118.1285681442453068, -7.893985811506177619, -18.51759400769804742 ) ) ;
#27837 = CARTESIAN_POINT ( 'NONE',  ( 136.5847729262652592, -8.473408049995818203, -17.81764962400096763 ) ) ;
#27838 = ORIENTED_EDGE ( 'NONE', *, *, #1500, .T. ) ;
#27839 = ADVANCED_FACE ( 'NONE', ( #19797 ), #33682, .F. ) ;
#27840 = CARTESIAN_POINT ( 'NONE',  ( 123.8411891859119862, -8.844754642576884152, -8.592115655440050404 ) ) ;
#27841 = CARTESIAN_POINT ( 'NONE',  ( 135.7778351055028452, -1.201940516317425711, -8.685489187000964506 ) ) ;
#27842 = EDGE_CURVE ( 'NONE', #40576, #7297, #7672, .T. ) ;
#27843 = B_SPLINE_CURVE_WITH_KNOTS ( 'NONE', 3,
 ( #34825, #38932, #35734, #413 ),
 .UNSPECIFIED., .F., .F.,
 ( 4, 4 ),
 ( 0.004629286548550820037, 0.006869623107310019426 ),
 .UNSPECIFIED. ) ;
#27844 = EDGE_CURVE ( 'NONE', #10287, #44451, #34223, .T. ) ;
#27845 = CARTESIAN_POINT ( 'NONE',  ( 122.2696148109119889, -4.089484607189486809, -7.948022111789456723 ) ) ;
#27846 = CARTESIAN_POINT ( 'NONE',  ( 108.9545983795247821, -0.7896495226426338832, -9.318865927141430916 ) ) ;
#27847 = CARTESIAN_POINT ( 'NONE',  ( 120.9649014775786355, -6.222761293078241884, -8.102969835052219238 ) ) ;
#27848 = VERTEX_POINT ( 'NONE', #34142 ) ;
#27849 = ORIENTED_EDGE ( 'NONE', *, *, #9440, .T. ) ;
#27850 = CIRCLE ( 'NONE', #8180, 6.479565957685750277 ) ;
#27851 = CARTESIAN_POINT ( 'NONE',  ( 115.6325948109119821, 0.2603800115204892296, -16.42320221600525088 ) ) ;
#27852 = CARTESIAN_POINT ( 'NONE',  ( 123.8579614775786126, -9.859900752359378018, -12.68260735090039759 ) ) ;
#27853 = CARTESIAN_POINT ( 'NONE',  ( 79.79010115959992788, 5.106172230548961188, -4.893215200338314474 ) ) ;
#27854 = CARTESIAN_POINT ( 'NONE',  ( 69.36136150295220659, -101.1685209014307674, -50.56525720990386219 ) ) ;
#27855 = CARTESIAN_POINT ( 'NONE',  ( 121.3619881442452879, -4.089484607189486809, -7.948022111789456723 ) ) ;
#27856 = CARTESIAN_POINT ( 'NONE',  ( 70.19189222814998175, -64.81574766768041229, -39.12908228425553858 ) ) ;
#27857 = CIRCLE ( 'NONE', #29307, 0.9999999999999952260 ) ;
#27858 = LINE ( 'NONE', #3228, #40459 ) ;
#27859 = CARTESIAN_POINT ( 'NONE',  ( 123.8012348109119642, 0.2603800115204892296, -16.42320221600525088 ) ) ;
#27861 = CARTESIAN_POINT ( 'NONE',  ( 124.7655881442452852, -9.859900752359378018, -12.68260735090039759 ) ) ;
#27860 = CARTESIAN_POINT ( 'NONE',  ( 120.6245414775786458, -9.988377603198976828, -10.36322818467138340 ) ) ;
#27862 = CARTESIAN_POINT ( 'NONE',  ( 118.6391081442452986, -5.574606645277164318, -18.38911715685844683 ) ) ;
#27863 = CARTESIAN_POINT ( 'NONE',  ( 70.55229225240181279, -24.89194276641628889, -5.467054258871676176 ) ) ;
#27864 = CARTESIAN_POINT ( 'NONE',  ( 115.8595014775786609, -1.834011780172310813, -8.268836392978581529 ) ) ;
#27865 = VERTEX_POINT ( 'NONE', #13639 ) ;
#27866 = DIRECTION ( 'NONE',  ( -0.000000000000000000, -0.9284778069183721172, -0.3713878862591650232 ) ) ;
#27867 = CARTESIAN_POINT ( 'NONE',  ( 106.3848327545248651, -2.477300249445798297, -19.15521520033831138 ) ) ;
#27868 = CARTESIAN_POINT ( 'NONE',  ( 107.4266296295248821, -4.863998795839590272, -8.388885654883775800 ) ) ;
#27869 = CARTESIAN_POINT ( 'NONE',  ( 106.4542858795248179, -0.7896495226426338832, -17.46756447353520159 ) ) ;
#27870 = CARTESIAN_POINT ( 'NONE',  ( -13.32377113153209791, -5.100909530930220370, -18.19321520033831874 ) ) ;
#27871 = CARTESIAN_POINT ( 'NONE',  ( 126.0703014775786102, -0.1624402480850797581, -16.17319339645315424 ) ) ;
#27872 = EDGE_LOOP ( 'NONE', ( #11039, #13428, #9816, #11158 ) ) ;
#27873 = CARTESIAN_POINT ( 'NONE',  ( 123.6877814775786533, -3.383040157471821630, -19.15922257007629170 ) ) ;
#27874 = CARTESIAN_POINT ( 'NONE',  ( 111.1770983795247787, -0.7896495226426338832, -9.318865927141430916 ) ) ;
#27875 = LINE ( 'NONE', #10770, #30715 ) ;
#27876 = CARTESIAN_POINT ( 'NONE',  ( 122.4965214775786251, -10.30919188438810075, -12.61870101168855918 ) ) ;
#27877 = CARTESIAN_POINT ( 'NONE',  ( 125.0492214775786266, -6.344957434206665248, -7.627207830600338134 ) ) ;
#27878 = PLANE ( 'NONE',  #14101 ) ;
#27879 = CARTESIAN_POINT ( 'NONE',  ( 112.0020881442453344, 0.2603800115204892296, -16.42320221600525088 ) ) ;
#27880 = EDGE_CURVE ( 'NONE', #36176, #36279, #8028, .T. ) ;
#27881 = CARTESIAN_POINT ( 'NONE',  ( 114.9275671295247889, -10.62599879583958540, -13.39321520033831447 ) ) ;
#27882 = CARTESIAN_POINT ( 'NONE',  ( 106.1764733795248219, -8.938348069036489818, -17.46756447353520159 ) ) ;
#27883 = ORIENTED_EDGE ( 'NONE', *, *, #4774, .T. ) ;
#27884 = DIRECTION ( 'NONE',  ( -1.387778780781445478E-15, -1.000000000000000000, 0.000000000000000000 ) ) ;
#27885 = CARTESIAN_POINT ( 'NONE',  ( 113.9307948109119764, -10.15424416112533912, -14.75197769757731336 ) ) ;
#27886 = CIRCLE ( 'NONE', #10437, 2.999999999999999556 ) ;
#27887 = CARTESIAN_POINT ( 'NONE',  ( 126.2972081442452890, -2.084020599724406786, -8.691656652584148546 ) ) ;
#27888 = CARTESIAN_POINT ( 'NONE',  ( 114.5803015045248117, -2.477300249445798297, -7.631215200338321125 ) ) ;
#27889 = CARTESIAN_POINT ( 'NONE',  ( 106.8015515045248378, -6.936859964151250502, -18.39754474579286025 ) ) ;
#27890 = CARTESIAN_POINT ( 'NONE',  ( 121.8725281442453223, -6.222761293078241884, -8.102969835052219238 ) ) ;
#27891 = UNCERTAINTY_MEASURE_WITH_UNIT (LENGTH_MEASURE( 1.000000000000000082E-05 ), #14138, 'distance_accuracy_value', 'NONE');
#27892 = CARTESIAN_POINT ( 'NONE',  ( 118.6391081442452986, -5.574606645277164318, -18.38911715685844683 ) ) ;
#27893 = CARTESIAN_POINT ( 'NONE',  ( 126.1837548109119211, -10.63000616557722466, -14.87417383870573495 ) ) ;
#27894 = EDGE_LOOP ( 'NONE', ( #42934, #28545, #8716, #40255 ) ) ;
#27895 = DIRECTION ( 'NONE',  ( -0.7871354856660202071, 0.6167752151498580027, 0.002461946824133919541 ) ) ;
#27896 = AXIS2_PLACEMENT_3D ( 'NONE', #11974, #25877, #4889 ) ;
#27897 = PLANE ( 'NONE',  #14227 ) ;
#27898 = CARTESIAN_POINT ( 'NONE',  ( 113.4202548109119846, 0.1319031606808879209, -14.10382304977623669 ) ) ;
#27899 = ORIENTED_EDGE ( 'NONE', *, *, #39791, .T. ) ;
#27900 = DIRECTION ( 'NONE',  ( -1.000000000000000000, 0.000000000000000000, -0.000000000000000000 ) ) ;
#27901 = EDGE_CURVE ( 'NONE', #33593, #25225, #45097, .T. ) ;
#27902 = CARTESIAN_POINT ( 'NONE',  ( 111.9410827545248708, -6.936859964151250502, -8.388885654883777576 ) ) ;
#27903 = ORIENTED_EDGE ( 'NONE', *, *, #13435, .F. ) ;
#27904 = CARTESIAN_POINT ( 'NONE',  ( 118.0151148109119816, 0.4262465694468514643, -12.03445270309931736 ) ) ;
#27905 = CARTESIAN_POINT ( 'NONE',  ( 112.7395348109119766, -4.153390946401321671, -8.397313243818183892 ) ) ;
#27906 = EDGE_CURVE ( 'NONE', #15493, #10303, #16588, .T. ) ;
#27907 =( BOUNDED_CURVE ( )  B_SPLINE_CURVE ( 3, ( #6220, #12851, #13072, #30169 ),
 .UNSPECIFIED., .F., .T. ) 
 B_SPLINE_CURVE_WITH_KNOTS ( ( 4, 4 ),
 ( 4.712388980384689674, 5.355890089177970381 ),
 .UNSPECIFIED. ) 
 CURVE ( )  GEOMETRIC_REPRESENTATION_ITEM ( )  RATIONAL_B_SPLINE_CURVE ( ( 1.000000000000000000, 0.9657888653670090306, 0.9657888653670090306, 1.000000000000000000 ) ) 
 REPRESENTATION_ITEM ( '' )  );
#27908 = CARTESIAN_POINT ( 'NONE',  ( 117.4103264091100840, -0.9924539043446216624, -17.29976612834909133 ) ) ;
#27909 = CARTESIAN_POINT ( 'NONE',  ( 124.6051735609119646, -9.645473719204776586, -14.86997237629376656 ) ) ;
#27910 = ORIENTED_EDGE ( 'NONE', *, *, #2319, .T. ) ;
#27911 = VECTOR ( 'NONE', #23922, 1000.000000000000000 ) ;
#27912 = DIRECTION ( 'NONE',  ( -0.000000000000000000, -0.9284778069183718952, -0.3713878862591649677 ) ) ;
#27913 = CARTESIAN_POINT ( 'NONE',  ( 125.3566265649618288, -1.353822015633321829, -7.281778159245134496 ) ) ;
#27914 = CARTESIAN_POINT ( 'NONE',  ( 113.3995983795247895, -0.7896495226426338832, -9.318865927141430916 ) ) ;
#27915 = CIRCLE ( 'NONE', #36637, 2.999999999999999556 ) ;
#27916 = CARTESIAN_POINT ( 'NONE',  ( 118.1329114811013312, -2.280480477428486807, -18.08254604495228435 ) ) ;
#27917 = CARTESIAN_POINT ( 'NONE',  ( 121.8725281442453223, -6.222761293078241884, -8.102969835052219238 ) ) ;
#27918 = CARTESIAN_POINT ( 'NONE',  ( 117.1074881442453233, 0.4262465694468514643, -12.03445270309931736 ) ) ;
#27919 = CARTESIAN_POINT ( 'NONE',  ( 113.6471614775786492, -4.153390946401318118, -8.397313243818187445 ) ) ;
#27920 = EDGE_LOOP ( 'NONE', ( #22595, #27620, #21714, #22502 ) ) ;
#27921 = CARTESIAN_POINT ( 'NONE',  ( 85.15861813568058380, -25.23119213852205789, -15.24166438581092109 ) ) ;
#27922 = CARTESIAN_POINT ( 'NONE',  ( 115.8595014775786609, -7.643976991954077427, -18.09477374809248928 ) ) ;
#27923 = CARTESIAN_POINT ( 'NONE',  ( 119.7434548109119703, -2.254126046650808401, -18.26827295101220017 ) ) ;
#27924 = VECTOR ( 'NONE', #11348, 1000.000000000000000 ) ;
#27925 = CARTESIAN_POINT ( 'NONE',  ( 66.38809756183205479, -36.79083284667497367, -4.893215200338314474 ) ) ;
#27926 = CARTESIAN_POINT ( 'NONE',  ( 72.54180985774836188, -56.01452643456254776, -34.87945145442834871 ) ) ;
#27927 = CARTESIAN_POINT ( 'NONE',  ( 116.0864081442453113, -9.988377603198976828, -10.36322818467138340 ) ) ;
#27928 = ORIENTED_EDGE ( 'NONE', *, *, #18431, .F. ) ;
#27929 = CARTESIAN_POINT ( 'NONE',  ( 114.5547881442453217, -5.638512984488999180, -18.83840828888717311 ) ) ;
#27930 = CARTESIAN_POINT ( 'NONE',  ( 151.2860562277021472, -0.6896191363000483410, -17.70303589939592825 ) ) ;
#27931 = CARTESIAN_POINT ( 'NONE',  ( 110.0658483795247804, -0.7896495226426338832, -9.318865927141430916 ) ) ;
#27932 = CARTESIAN_POINT ( 'NONE',  ( 113.9307948109119906, 0.9020085738987339008, -11.91225656197089222 ) ) ;
#27933 = CARTESIAN_POINT ( 'NONE',  ( 113.8740681442453138, 0.5811942927096154232, -14.16772938898807155 ) ) ;
#27934 = CARTESIAN_POINT ( 'NONE',  ( 125.3328548109119964, -0.8288870151387760510, -10.36305467784173118 ) ) ;
#27935 = CARTESIAN_POINT ( 'NONE',  ( 60.06931813437629586, -14.72076136720887085, -18.18301750815651374 ) ) ;
#27936 = CARTESIAN_POINT ( 'NONE',  ( 108.1906140045248463, 0.1403307496149616695, -15.46607636864997204 ) ) ;
#27937 = CARTESIAN_POINT ( 'NONE',  ( 111.3160046295247838, -4.863998795839590272, -7.631215200338315796 ) ) ;
#27938 = CARTESIAN_POINT ( 'NONE',  ( 109.2294420763164453, -8.136444762514427609, -17.62486350101510624 ) ) ;
#27939 = CARTESIAN_POINT ( 'NONE',  ( 118.2987481442453088, -7.894159318335828068, -9.358103419637847864 ) ) ;
#27940 = DIRECTION ( 'NONE',  ( 0.9970811988817434024, -0.07634843047859724008, 9.125038414728753042E-18 ) ) ;
#27941 = CARTESIAN_POINT ( 'NONE',  ( 117.0806140045248185, 0.1403307496149616695, -15.46607636864997204 ) ) ;
#27942 = CARTESIAN_POINT ( 'NONE',  ( 108.3295202545248657, -10.62599879583958717, -15.77991374673208469 ) ) ;
#27943 = CARTESIAN_POINT ( 'NONE',  ( 126.5561942423915838, -4.825870161346100140, -8.224435640663250169 ) ) ;
#27944 = CARTESIAN_POINT ( 'NONE',  ( 124.9924948109119924, -4.089484607189486809, -7.948022111789456723 ) ) ;
#27945 = DIRECTION ( 'NONE',  ( 0.9908103287288528849, -0.1352586133457776008, 0.000000000000000000 ) ) ;
#27946 = CARTESIAN_POINT ( 'NONE',  ( 121.1350814775786233, 0.5811942927096110934, -14.16772938898807510 ) ) ;
#27947 = CARTESIAN_POINT ( 'NONE',  ( 116.4267681442453153, -3.383040157471821630, -19.15922257007629170 ) ) ;
#27949 = ORIENTED_EDGE ( 'NONE', *, *, #10180, .F. ) ;
#27948 = ADVANCED_FACE ( 'NONE', ( #30958 ), #13854, .T. ) ;
#27950 = VECTOR ( 'NONE', #43249, 1000.000000000000000 ) ;
#27951 = CARTESIAN_POINT ( 'NONE',  ( 115.3489614775786407, -0.8288870151387760510, -10.36305467784173118 ) ) ;
#27952 = AXIS2_PLACEMENT_3D ( 'NONE', #30571, #9838, #44948 ) ;
#27953 = CARTESIAN_POINT ( 'NONE',  ( 124.8790414775786246, -0.4660016031367893996, -10.09054647747474043 ) ) ;
#27954 = CARTESIAN_POINT ( 'NONE',  ( 118.3554748109119998, 0.2603800115204892296, -16.42320221600525088 ) ) ;
#27955 = CARTESIAN_POINT ( 'NONE',  ( 117.3343948109119737, -6.222761293078241884, -8.102969835052219238 ) ) ;
#27956 = ORIENTED_EDGE ( 'NONE', *, *, #41804, .F. ) ;
#27957 = CARTESIAN_POINT ( 'NONE',  ( 122.3830681442452857, -1.833838273342659697, -17.42832698103878286 ) ) ;
#27958 = CIRCLE ( 'NONE', #33760, 2.000000000000000444 ) ;
#27959 = CARTESIAN_POINT ( 'NONE',  ( 115.2922348109119781, -10.63000616557722466, -14.87417383870573495 ) ) ;
#27960 = EDGE_CURVE ( 'NONE', #424, #11479, #15319, .T. ) ;
#27961 = DIRECTION ( 'NONE',  ( -0.2768435750659266059, -0.3568721902840680249, 0.8921882507333128709 ) ) ;
#27962 = CARTESIAN_POINT ( 'NONE',  ( 113.1217858795247935, -0.7896495226426338832, -17.46756447353520159 ) ) ;
#27963 = CARTESIAN_POINT ( 'NONE',  ( 68.27567836778572996, -1.300826558512744535, -10.52192843399248545 ) ) ;
#27964 = DIRECTION ( 'NONE',  ( -0.4461977533474357216, -0.8271203734159378040, -0.3417300876246930907 ) ) ;
#27965 = CARTESIAN_POINT ( 'NONE',  ( 143.3676850761856940, -64.41823023953081417, -19.25521411788945514 ) ) ;
#27966 = CARTESIAN_POINT ( 'NONE',  ( 116.0864081442453113, -9.988377603198976828, -10.36322818467138340 ) ) ;
#27967 =( REPRESENTATION_RELATIONSHIP ('NONE','NONE', #36667, #30918 ) REPRESENTATION_RELATIONSHIP_WITH_TRANSFORMATION ( #22945 )SHAPE_REPRESENTATION_RELATIONSHIP( ) );
#27968 = CARTESIAN_POINT ( 'NONE',  ( 96.46827370896536991, -26.60028948451273223, -14.20056342530837412 ) ) ;
#27969 = CARTESIAN_POINT ( 'NONE',  ( 113.1366214775786432, -7.643976991954077427, -18.09477374809248928 ) ) ;
#27970 = CARTESIAN_POINT ( 'NONE',  ( 123.9584548109119737, -12.48189245497263755, -10.95032834292243074 ) ) ;
#27971 = CARTESIAN_POINT ( 'NONE',  ( 69.36136150295220659, -61.11559914574721120, -34.54422812497841022 ) ) ;
#27972 = CARTESIAN_POINT ( 'NONE',  ( 115.9693640045247776, 0.1403307496149616695, -15.46607636864997204 ) ) ;
#27973 = CARTESIAN_POINT ( 'NONE',  ( 116.6536748109119941, 0.9020085738987339008, -11.91225656197089222 ) ) ;
#27974 = AXIS2_PLACEMENT_3D ( 'NONE', #31038, #38101, #41548 ) ;
#27975 = DIRECTION ( 'NONE',  ( 0.8636456077245088236, -0.5040994586965589219, 0.000000000000000000 ) ) ;
#27976 = DIRECTION ( 'NONE',  ( -0.2768435750659263839, -0.3568721902840679139, 0.8921882507333128709 ) ) ;
#27977 = ADVANCED_FACE ( 'NONE', ( #41241 ), #41016, .T. ) ;
#27978 = CARTESIAN_POINT ( 'NONE',  ( 119.0929214775786278, -5.638512984489023161, -18.83840828888716601 ) ) ;
#27979 = DIRECTION ( 'NONE',  ( 1.000000000000000000, 0.000000000000000000, -0.000000000000000000 ) ) ;
#27980 = CARTESIAN_POINT ( 'NONE',  ( 120.8514481442452961, -2.084020599724406786, -8.691656652584148546 ) ) ;
#27981 = ORIENTED_EDGE ( 'NONE', *, *, #38036, .F. ) ;
#27982 = CARTESIAN_POINT ( 'NONE',  ( 136.0617147589354090, -9.506656963484036993, -9.746956911094994069 ) ) ;
#27983 = CARTESIAN_POINT ( 'NONE',  ( 121.3619881442452879, -4.089484607189486809, -7.948022111789456723 ) ) ;
#27984 = FACE_OUTER_BOUND ( 'NONE', #35074, .T. ) ;
#27985 = CARTESIAN_POINT ( 'NONE',  ( 115.5191414775786569, -6.222761293078241884, -8.102969835052219238 ) ) ;
#27986 = CARTESIAN_POINT ( 'NONE',  ( 114.2711548109119803, -0.1624402480850797581, -16.17319339645315424 ) ) ;
#27987 = DIRECTION ( 'NONE',  ( 0.000000000000000000, -0.3818493186865927203, 0.9242245927363029745 ) ) ;
#27988 = CARTESIAN_POINT ( 'NONE',  ( 111.4549108795247747, -8.938348069036489818, -9.318865927141430916 ) ) ;
#27989 = CARTESIAN_POINT ( 'NONE',  ( 122.0994348109119443, -10.15424416112533912, -14.75197769757731336 ) ) ;
#27990 = CARTESIAN_POINT ( 'NONE',  ( 121.1918081442452859, -10.15424416112533912, -14.75197769757731336 ) ) ;
#27991 = CYLINDRICAL_SURFACE ( 'NONE', #42024, 1.999999999999998890 ) ;
#27992 = CARTESIAN_POINT ( 'NONE',  ( 109.2294421297036280, -3.476265968579914212, -8.054548070311122743 ) ) ;
#27993 = DIRECTION ( 'NONE',  ( 0.000000000000000000, -0.3818493186865927203, 0.9242245927363029745 ) ) ;
#27994 = CARTESIAN_POINT ( 'NONE',  ( 107.0099108795247815, -1.325403438956436419, -16.93181055722141792 ) ) ;
#27995 = CARTESIAN_POINT ( 'NONE',  ( 117.2294421295247844, 1.035107641088057973, -21.72657133228191739 ) ) ;
#27996 = CARTESIAN_POINT ( 'NONE',  ( 113.6471614775786492, -5.638512984488999180, -18.83840828888717311 ) ) ;
#27997 = CARTESIAN_POINT ( 'NONE',  ( 116.3133148109119759, -7.893985811506177619, -18.51759400769804742 ) ) ;
#27998 = CARTESIAN_POINT ( 'NONE',  ( 110.6909265045248247, -7.250697342233347165, -19.15521520033831138 ) ) ;
#27999 = LINE ( 'NONE', #10669, #9723 ) ;
#28000 = ORIENTED_EDGE ( 'NONE', *, *, #28388, .T. ) ;
#28001 = CARTESIAN_POINT ( 'NONE',  ( 70.36267391504962632, -5.685877709920933221, -19.39321520033831447 ) ) ;
#28002 = CARTESIAN_POINT ( 'NONE',  ( 122.2128881442453263, -1.834011780172310813, -8.268836392978581529 ) ) ;
#28003 = CARTESIAN_POINT ( 'NONE',  ( 112.1722681442453222, -0.4660016031367893996, -10.09054647747474043 ) ) ;
#28004 = CARTESIAN_POINT ( 'NONE',  ( 119.6601881442453106, -1.833838273342659253, -17.42832698103878286 ) ) ;
#28005 = CARTESIAN_POINT ( 'NONE',  ( 125.8433948109119456, -1.834011780172310813, -8.268836392978581529 ) ) ;
#28006 = CARTESIAN_POINT ( 'NONE',  ( 117.4478481442453131, 0.2603800115204892296, -16.42320221600525088 ) ) ;
#28007 = AXIS2_PLACEMENT_3D ( 'NONE', #6655, #34444, #17150 ) ;
#28008 = CARTESIAN_POINT ( 'NONE',  ( 108.0517077545248696, -2.791137627527939813, -18.39754474579286025 ) ) ;
#28009 = EDGE_CURVE ( 'NONE', #14596, #36351, #18963, .T. ) ;
#28010 = CARTESIAN_POINT ( 'NONE',  ( 112.3991748109119868, -1.833838273342658809, -17.42832698103878286 ) ) ;
#28011 = CARTESIAN_POINT ( 'NONE',  ( 69.69189222814998175, -41.76310523276723785, -19.39321520033831447 ) ) ;
#28012 = ORIENTED_EDGE ( 'NONE', *, *, #19756, .F. ) ;
#28013 = CARTESIAN_POINT ( 'NONE',  ( 119.7736414775786358, -10.30919188438810075, -12.61870101168855918 ) ) ;
#28014 = CARTESIAN_POINT ( 'NONE',  ( 121.5492360609119800, -6.564341423271550902, -7.887810678476487425 ) ) ;
#28015 = CARTESIAN_POINT ( 'NONE',  ( 114.7249681442453237, 0.2603800115204892296, -16.42320221600525088 ) ) ;
#28016 = VERTEX_POINT ( 'NONE', #20484 ) ;
#28017 = CARTESIAN_POINT ( 'NONE',  ( 114.5108483795247878, -0.7896495226426338832, -9.318865927141430916 ) ) ;
#28018 = LINE ( 'NONE', #3605, #17976 ) ;
#28019 = DIRECTION ( 'NONE',  ( 0.000000000000000000, 0.000000000000000000, -1.000000000000000000 ) ) ;
#28020 = CARTESIAN_POINT ( 'NONE',  ( 124.6340697093320387, -5.999156839134622388, -18.26265215102739248 ) ) ;
#28021 = CARTESIAN_POINT ( 'NONE',  ( 71.99789814782840836, -24.87091310681484657, -18.19321520033831519 ) ) ;
#28022 = CARTESIAN_POINT ( 'NONE',  ( 120.3409081442453044, -8.899110576539710493, -16.42337572283490132 ) ) ;
#28023 = DIRECTION ( 'NONE',  ( 0.000000000000000000, 0.000000000000000000, -1.000000000000000000 ) ) ;
#28024 = CARTESIAN_POINT ( 'NONE',  ( 120.6245414775786458, -0.1624402480850797581, -16.17319339645315424 ) ) ;
#28025 = AXIS2_PLACEMENT_3D ( 'NONE', #10644, #42104, #34565 ) ;
#28026 = DIRECTION ( 'NONE',  ( 0.000000000000000000, 0.6004852223388321697, -0.7996358532186279566 ) ) ;
#28027 = CARTESIAN_POINT ( 'NONE',  ( 119.9438214775786378, -2.084020599724406786, -8.691656652584148546 ) ) ;
#28028 = CARTESIAN_POINT ( 'NONE',  ( 122.5910329359119970, -4.283928203966213211, -7.183505701512925334 ) ) ;
#28029 = CARTESIAN_POINT ( 'NONE',  ( 114.7816948109119863, 0.5811942927096154232, -14.16772938898807155 ) ) ;
#28030 = CARTESIAN_POINT ( 'NONE',  ( 59.44377208703740223, -12.82110557137145967, -9.393546723914594665 ) ) ;
#28031 = CONICAL_SURFACE ( 'NONE', #34551, 2.445500000000004448, 0.9599310885968757034 ) ;
#28032 = CARTESIAN_POINT ( 'NONE',  ( 116.9940348109119839, -0.1624402480850797581, -16.17319339645315424 ) ) ;
#28033 = ORIENTED_EDGE ( 'NONE', *, *, #5958, .F. ) ;
#28034 = CARTESIAN_POINT ( 'NONE',  ( 117.1074881442453233, -10.63000616557722466, -14.87417383870573495 ) ) ;
#28035 = CARTESIAN_POINT ( 'NONE',  ( 109.2324108795247923, -8.938348069036489818, -9.318865927141430916 ) ) ;
#28036 = CARTESIAN_POINT ( 'NONE',  ( 115.5191414775786427, -6.222761293078232114, -8.102969835052212133 ) ) ;
#28037 = CARTESIAN_POINT ( 'NONE',  ( 114.8344297178593507, -0.3595008806742178709, -15.96590799893915857 ) ) ;
#28038 = DIRECTION ( 'NONE',  ( 0.9609149988134837450, -0.1028163501681639419, 0.2570431154366518145 ) ) ;
#28039 = CARTESIAN_POINT ( 'NONE',  ( 121.5888948109119809, -10.30919188438810075, -12.61870101168855918 ) ) ;
#28040 = ORIENTED_EDGE ( 'NONE', *, *, #32038, .T. ) ;
#28041 = CARTESIAN_POINT ( 'NONE',  ( 126.5254139958957040, -8.459460868501995634, -9.701178152251141995 ) ) ;
#28042 = CARTESIAN_POINT ( 'NONE',  ( 118.1852948109119836, -4.153390946401325223, -8.397313243818185668 ) ) ;
#28043 = FACE_OUTER_BOUND ( 'NONE', #13269, .T. ) ;
#28044 = CARTESIAN_POINT ( 'NONE',  ( 64.20801161461099582, -15.17998946340411592, -16.19887345869426198 ) ) ;
#28045 = CARTESIAN_POINT ( 'NONE',  ( 126.2404814775786264, -9.261995988541697145, -16.69588392320189030 ) ) ;
#28046 = CARTESIAN_POINT ( 'NONE',  ( 111.7327233795247849, -1.325403438956436419, -9.854619843455211026 ) ) ;
#28047 = CARTESIAN_POINT ( 'NONE',  ( 88.98550738977573360, -10.74509419609185379, -14.14321520033831625 ) ) ;
#28048 = VERTEX_POINT ( 'NONE', #24128 ) ;
#28049 = CARTESIAN_POINT ( 'NONE',  ( 115.5191414775786569, -3.383040157471821630, -19.15922257007629170 ) ) ;
#28050 = CARTESIAN_POINT ( 'NONE',  ( 125.6732148109119862, -9.859900752359378018, -12.68260735090039759 ) ) ;
#28051 = CARTESIAN_POINT ( 'NONE',  ( 124.0848681442452772, -4.089484607189486809, -7.948022111789456723 ) ) ;
#28052 = CARTESIAN_POINT ( 'NONE',  ( 115.9729548109119861, -3.505236298600246325, -18.68346056562440793 ) ) ;
#28053 = FACE_OUTER_BOUND ( 'NONE', #2728, .T. ) ;
#28054 = CARTESIAN_POINT ( 'NONE',  ( 118.2987481442453088, -1.561330072975668504, -17.79121239304076951 ) ) ;
#28055 = CARTESIAN_POINT ( 'NONE',  ( 70.19189222814998175, -55.40259354030312267, -35.36385344588251911 ) ) ;
#28056 = CARTESIAN_POINT ( 'NONE',  ( 0.04488520489200759078, -6.166763362545027327, -8.593215200338315540 ) ) ;
#28057 = CARTESIAN_POINT ( 'NONE',  ( 124.6521348109119884, -7.894159318335828068, -9.358103419637847864 ) ) ;
#28058 = EDGE_LOOP ( 'NONE', ( #20467, #8556, #11376, #33414, #25964 ) ) ;
#28059 = AXIS2_PLACEMENT_3D ( 'NONE', #36465, #15959, #36906 ) ;
#28060 = CARTESIAN_POINT ( 'NONE',  ( 70.19189222814998175, -100.0979043305785581, -53.24182196210380624 ) ) ;
#28061 = CARTESIAN_POINT ( 'NONE',  ( 115.1787814775786387, -9.988377603198976828, -10.36322818467138340 ) ) ;
#28062 = CARTESIAN_POINT ( 'NONE',  ( 123.8579614775786126, -9.859900752359378018, -12.68260735090039759 ) ) ;
#28063 = ORIENTED_EDGE ( 'NONE', *, *, #39109, .F. ) ;
#28064 = CARTESIAN_POINT ( 'NONE',  ( 121.0807175202278074, -2.239543233855044946, -18.13706010537467606 ) ) ;
#28065 = CARTESIAN_POINT ( 'NONE',  ( 122.2128881442453263, -1.834011780172310813, -8.268836392978581529 ) ) ;
#28066 = CONICAL_SURFACE ( 'NONE', #29518, 5.999999999999997335, 0.4636476090008060935 ) ;
#28067 = CARTESIAN_POINT ( 'NONE',  ( 108.6073327545248048, -2.477300249445798297, -19.15521520033831138 ) ) ;
#28068 = CARTESIAN_POINT ( 'NONE',  ( 121.5321681442453183, -0.1624402480850797581, -16.17319339645315424 ) ) ;
#28069 = EDGE_CURVE ( 'NONE', #19352, #22762, #44882, .T. ) ;
#28070 = VERTEX_POINT ( 'NONE', #34583 ) ;
#28071 = ORIENTED_EDGE ( 'NONE', *, *, #37975, .F. ) ;
#28072 = CARTESIAN_POINT ( 'NONE',  ( 112.7962614775786676, -3.383040157471821630, -19.15922257007629170 ) ) ;
#28073 = CARTESIAN_POINT ( 'NONE',  ( 123.0637881442452937, -8.899110576539710493, -16.42337572283490132 ) ) ;
#28074 = CARTESIAN_POINT ( 'NONE',  ( 79.40190946915554093, 5.047224606967246174, -20.48130549182737425 ) ) ;
#28075 = CARTESIAN_POINT ( 'NONE',  ( 59.77100663911058120, -14.81899367705580595, -18.19321520033832229 ) ) ;
#28076 = ADVANCED_FACE ( 'NONE', ( #13194 ), #34363, .F. ) ;
#28077 = CARTESIAN_POINT ( 'NONE',  ( 123.9146881442452894, 0.9020085738987339008, -11.91225656197089222 ) ) ;
#28078 = DIRECTION ( 'NONE',  ( 0.8636456077245088236, -0.5040994586965589219, 0.000000000000000000 ) ) ;
#28079 = CARTESIAN_POINT ( 'NONE',  ( 88.22708560785949317, -3.622631779710408395, -18.64321520033831803 ) ) ;
#28080 = CARTESIAN_POINT ( 'NONE',  ( 123.7445081442452874, -1.561330072975668948, -17.79121239304076951 ) ) ;
#28082 = CARTESIAN_POINT ( 'NONE',  ( 125.1059481442452750, -1.833838273342660141, -17.42832698103878286 ) ) ;
#28081 = CARTESIAN_POINT ( 'NONE',  ( 120.7379948109119709, -10.63000616557722466, -14.87417383870573495 ) ) ;
#28083 = CARTESIAN_POINT ( 'NONE',  ( 119.1496481442453046, -6.222761293078241884, -8.102969835052219238 ) ) ;
#28084 = LINE ( 'NONE', #41992, #41497 ) ;
#28085 = CARTESIAN_POINT ( 'NONE',  ( 114.3278814775786429, -10.30919188438810075, -12.61870101168855918 ) ) ;
#28086 = ORIENTED_EDGE ( 'NONE', *, *, #17537, .F. ) ;
#28087 = CARTESIAN_POINT ( 'NONE',  ( 85.75809888461174069, -18.45227461768569199, -7.393215200338315363 ) ) ;
#28088 = CIRCLE ( 'NONE', #8426, 3.500000000000003109 ) ;
#28089 = CARTESIAN_POINT ( 'NONE',  ( 113.0523327545247838, -6.936859964151250502, -8.388885654883777576 ) ) ;
#28090 = CARTESIAN_POINT ( 'NONE',  ( 109.9269421295247753, -9.868328341294093420, -13.39321520033831447 ) ) ;
#28091 = CARTESIAN_POINT ( 'NONE',  ( 113.4690515045247992, -6.936859964151250502, -18.39754474579286025 ) ) ;
#28092 = CARTESIAN_POINT ( 'NONE',  ( 125.9568481442452850, -6.344957434206665248, -7.627207830600338134 ) ) ;
#28093 = CARTESIAN_POINT ( 'NONE',  ( 125.3895814775786448, -2.084020599724406786, -8.691656652584148546 ) ) ;
#28094 = EDGE_LOOP ( 'NONE', ( #17961, #1079, #2183, #1405 ) ) ;
#28095 = EDGE_CURVE ( 'NONE', #34215, #1783, #21858, .T. ) ;
#28096 = CARTESIAN_POINT ( 'NONE',  ( 114.6115148109119986, -6.222761293078241884, -8.102969835052219238 ) ) ;
#28097 = CARTESIAN_POINT ( 'NONE',  ( 110.0658483795247804, -0.7896495226426338832, -9.318865927141430916 ) ) ;
#28098 = DIRECTION ( 'NONE',  ( -1.156482317317869950E-15, -1.000000000000000000, 0.000000000000000000 ) ) ;
#28099 = CARTESIAN_POINT ( 'NONE',  ( 124.1983214775786166, -8.166667518702819706, -8.995218007635861213 ) ) ;
#28100 = EDGE_CURVE ( 'NONE', #11967, #8479, #37337, .T. ) ;
#28101 = EDGE_CURVE ( 'NONE', #10336, #22908, #23682, .T. ) ;
#28102 = CARTESIAN_POINT ( 'NONE',  ( 123.9714148109119805, -0.4660016031367893996, -10.09054647747474043 ) ) ;
#28104 = CIRCLE ( 'NONE', #2595, 1.500000000000001332 ) ;
#28103 = CARTESIAN_POINT ( 'NONE',  ( 119.8823610609119754, -6.340755971794695078, -8.611740276972781771 ) ) ;
#28105 = CARTESIAN_POINT ( 'NONE',  ( 126.0135748109119902, -1.833838273342660141, -17.42832698103878286 ) ) ;
#28106 = CARTESIAN_POINT ( 'NONE',  ( 114.1635827545248389, -2.477300249445798297, -19.15521520033831138 ) ) ;
#28107 = CARTESIAN_POINT ( 'NONE',  ( 105.7597546295248350, -4.863998795839590272, -7.631215200338315796 ) ) ;
#28108 = ORIENTED_EDGE ( 'NONE', *, *, #16709, .T. ) ;
#28109 = CARTESIAN_POINT ( 'NONE',  ( 126.4599182912984077, -7.451362815295157205, -8.974203731756436042 ) ) ;
#28110 = CARTESIAN_POINT ( 'NONE',  ( 113.5337081442453240, -0.8288870151387760510, -10.36305467784173118 ) ) ;
#28111 = CARTESIAN_POINT ( 'NONE',  ( 113.8173414775786512, 0.2603800115204892296, -16.42320221600525088 ) ) ;
#28112 = CARTESIAN_POINT ( 'NONE',  ( 114.8581140045248361, -10.62599879583958717, -11.00651665394454604 ) ) ;
#28113 = CARTESIAN_POINT ( 'NONE',  ( 107.0099108795247815, -1.325403438956436419, -16.93181055722141792 ) ) ;
#28114 = CARTESIAN_POINT ( 'NONE',  ( 121.0783548109119749, -9.565557343593413364, -10.61323700422348004 ) ) ;
#28115 = CARTESIAN_POINT ( 'NONE',  ( 119.2063748109119814, -7.894159318335828068, -9.358103419637847864 ) ) ;
#28116 = CARTESIAN_POINT ( 'NONE',  ( 112.4559014775786778, -0.1624402480850797581, -16.17319339645315424 ) ) ;
#28117 = ORIENTED_EDGE ( 'NONE', *, *, #37268, .T. ) ;
#28118 = CARTESIAN_POINT ( 'NONE',  ( 120.9936110609119737, -6.340755971794695078, -8.611740276972781771 ) ) ;
#28119 = DIRECTION ( 'NONE',  ( -0.6049664196031393493, 0.7962509850245452769, 0.000000000000000000 ) ) ;
#28120 = CARTESIAN_POINT ( 'NONE',  ( 114.9518748109119883, -7.643976991954077427, -18.09477374809248928 ) ) ;
#28121 = EDGE_LOOP ( 'NONE', ( #29558, #44552, #28572, #38982 ) ) ;
#28122 = CARTESIAN_POINT ( 'NONE',  ( 126.2758031835854098, -9.050378324229031435, -16.17924689356632584 ) ) ;
#28123 = CARTESIAN_POINT ( 'NONE',  ( 106.8015515045248378, -2.477300249445798297, -7.631215200338321125 ) ) ;
#28124 = CARTESIAN_POINT ( 'NONE',  ( 110.5520202545248054, 0.1403307496149616695, -11.32035403202665336 ) ) ;
#28125 = EDGE_CURVE ( 'NONE', #35850, #23757, #38903, .T. ) ;
#28126 = VERTEX_POINT ( 'NONE', #14523 ) ;
#28127 = CARTESIAN_POINT ( 'NONE',  ( 119.0361948109119652, -2.084020599724406786, -8.691656652584148546 ) ) ;
#28128 = CARTESIAN_POINT ( 'NONE',  ( 112.3424481442453384, -3.505236298600246325, -18.68346056562440793 ) ) ;
#28129 = CARTESIAN_POINT ( 'NONE',  ( 124.5966688623432219, -9.713577380183913590, -14.62808432448665563 ) ) ;
#28130 = AXIS2_PLACEMENT_3D ( 'NONE', #32651, #43602, #5063 ) ;
#28131 = CARTESIAN_POINT ( 'NONE',  ( 123.3550173109119612, 0.2312338769422704887, -16.08380026872395874 ) ) ;
#28132 = ORIENTED_EDGE ( 'NONE', *, *, #9520, .F. ) ;
#28133 = DIRECTION ( 'NONE',  ( -0.9908103287288504424, 0.1352586133457951423, 0.000000000000000000 ) ) ;
#28134 = CARTESIAN_POINT ( 'NONE',  ( 124.7442371152527016, -2.402718219011967360, -6.010812890236988615 ) ) ;
#28135 = EDGE_CURVE ( 'NONE', #3445, #11630, #28436, .T. ) ;
#28136 = CARTESIAN_POINT ( 'NONE',  ( 116.1777233795247781, -8.938348069036489818, -17.46756447353520159 ) ) ;
#28137 = CARTESIAN_POINT ( 'NONE',  ( 113.0798948109119948, -0.4660016031367893996, -10.09054647747474043 ) ) ;
#28138 = CARTESIAN_POINT ( 'NONE',  ( 123.1772414775786189, -5.574606645277164318, -18.38911715685844683 ) ) ;
#28139 = CARTESIAN_POINT ( 'NONE',  ( 118.3554748109119998, -9.565557343593413364, -10.61323700422348004 ) ) ;
#28140 = CARTESIAN_POINT ( 'NONE',  ( 113.3277860444392076, -1.267766418764742387, -16.93314635290707315 ) ) ;
#28141 = ORIENTED_EDGE ( 'NONE', *, *, #36889, .F. ) ;
#28142 = CARTESIAN_POINT ( 'NONE',  ( 116.7104014775786425, -8.899110576539710493, -16.42337572283490132 ) ) ;
#28143 = DIRECTION ( 'NONE',  ( 0.000000000000000000, 0.5905882410490339574, 0.8069730661766899571 ) ) ;
#28144 = CARTESIAN_POINT ( 'NONE',  ( 65.66749702063913219, -36.20550398600038022, -5.467054258871666406 ) ) ;
#28145 = CARTESIAN_POINT ( 'NONE',  ( 116.9582927111058552, -1.267766418764730840, -16.93314635290706605 ) ) ;
#28146 = AXIS2_PLACEMENT_3D ( 'NONE', #11049, #18787, #35418 ) ;
#28147 = CARTESIAN_POINT ( 'NONE',  ( 113.8173414775786512, 0.2603800115204892296, -16.42320221600525088 ) ) ;
#28148 = VERTEX_POINT ( 'NONE', #42798 ) ;
#28149 = CARTESIAN_POINT ( 'NONE',  ( 115.8595014775786609, -1.834011780172310813, -8.268836392978581529 ) ) ;
#28150 = CARTESIAN_POINT ( 'NONE',  ( 115.8759982281897862, 0.3371508018708627152, -21.89321520033831447 ) ) ;
#28151 = CARTESIAN_POINT ( 'NONE',  ( 109.9269421295247753, 0.8980012041604618078, -13.39321520033831447 ) ) ;
#28152 = CARTESIAN_POINT ( 'NONE',  ( 114.1009748109119784, -4.089484607189486809, -7.948022111789456723 ) ) ;
#28153 = EDGE_CURVE ( 'NONE', #19198, #2194, #14568, .T. ) ;
#28154 = CARTESIAN_POINT ( 'NONE',  ( 112.5126281442453120, -10.30919188438810075, -12.61870101168855918 ) ) ;
#28155 = CARTESIAN_POINT ( 'NONE',  ( 124.1983214775786166, -1.833838273342659697, -17.42832698103878286 ) ) ;
#28156 = DIRECTION ( 'NONE',  ( 0.000000000000000000, -0.3818493186865936084, 0.9242245927363024194 ) ) ;
#28157 = CARTESIAN_POINT ( 'NONE',  ( 108.3989733795248753, -1.325403438956436419, -9.854619843455211026 ) ) ;
#28158 = ORIENTED_EDGE ( 'NONE', *, *, #20085, .T. ) ;
#28159 = LINE ( 'NONE', #20201, #40484 ) ;
#28160 = CARTESIAN_POINT ( 'NONE',  ( 109.2295290894191311, -5.098491836473954208, -18.58823644444565204 ) ) ;
#28161 = CARTESIAN_POINT ( 'NONE',  ( 116.7671281442453335, -7.643976991954077427, -18.09477374809248928 ) ) ;
#28162 = CARTESIAN_POINT ( 'NONE',  ( 105.6208483795248299, -0.7896495226426338832, -9.318865927141430916 ) ) ;
#28163 = CARTESIAN_POINT ( 'NONE',  ( 118.2795432127138611, -2.191907684172563986, -18.20049396185734025 ) ) ;
#28164 = CARTESIAN_POINT ( 'NONE',  ( 111.3160046295247838, -4.863998795839590272, -7.631215200338315796 ) ) ;
#28165 = CARTESIAN_POINT ( 'NONE',  ( 127.9806007748884298, -5.559840797202522999, -7.553254777380711715 ) ) ;
#28166 = CARTESIAN_POINT ( 'NONE',  ( 125.7866681442452688, -0.4660016031367893996, -10.09054647747474043 ) ) ;
#28167 = DIRECTION ( 'NONE',  ( -0.000000000000000000, -0.9284778069183718952, -0.3713878862591649677 ) ) ;
#28168 = EDGE_CURVE ( 'NONE', #44499, #14756, #8743, .T. ) ;
#28169 = CARTESIAN_POINT ( 'NONE',  ( 123.8579614775786126, 0.5811942927096110934, -14.16772938898807510 ) ) ;
#28170 = CARTESIAN_POINT ( 'NONE',  ( 115.7460481442453357, 0.9020085738987339008, -11.91225656197089222 ) ) ;
#28171 = EDGE_LOOP ( 'NONE', ( #19204, #16512, #39297, #31299, #20010 ) ) ;
#28172 = AXIS2_PLACEMENT_3D ( 'NONE', #26214, #8213, #36905 ) ;
#28173 = CARTESIAN_POINT ( 'NONE',  ( 114.2144281442453178, -1.833838273342658809, -17.42832698103878286 ) ) ;
#28174 = CARTESIAN_POINT ( 'NONE',  ( 71.02242295334774269, -57.11741039020605371, -39.15458185685995574 ) ) ;
#28175 = CARTESIAN_POINT ( 'NONE',  ( 119.0929214775786278, -5.638512984488999180, -18.83840828888717311 ) ) ;
#28176 = CARTESIAN_POINT ( 'NONE',  ( 117.6747548109119919, -7.643976991954077427, -18.09477374809248928 ) ) ;
#28177 = ORIENTED_EDGE ( 'NONE', *, *, #24554, .F. ) ;
#28178 = CARTESIAN_POINT ( 'NONE',  ( 122.9503348109119827, -9.859900752359378018, -12.68260735090039759 ) ) ;
#28179 =( BOUNDED_CURVE ( )  B_SPLINE_CURVE ( 2, ( #14567, #28037, #20967, #18212, #17544, #11379, #42390, #11155, #39182, #21634, #38493, #7946, #7721, #21857, #31437, #7268, #4293 ),
 .UNSPECIFIED., .F., .T. ) 
 B_SPLINE_CURVE_WITH_KNOTS ( ( 3, 2, 2, 2, 2, 2, 2, 2, 3 ),
 ( 0.1040431156034945931, 0.1125000000000000028, 0.1250000000000000000, 0.1375000000000000111, 0.1499999999999999944, 0.1625000000000000056, 0.1749999999999999889, 0.1875000000000000000, 0.1959568843965054930 ),
 .UNSPECIFIED. ) 
 CURVE ( )  GEOMETRIC_REPRESENTATION_ITEM ( )  RATIONAL_B_SPLINE_CURVE ( ( 0.9666851417651740608, 0.9485006404992000206, 1.000000000000000000, 0.9238795325112869605, 1.000000000000000000, 0.9238795325112869605, 1.000000000000000000, 0.9238795325112869605, 1.000000000000000000, 0.9238795325112869605, 1.000000000000000000, 0.9238795325112869605, 1.000000000000000000, 0.9238795325112869605, 1.000000000000000000, 0.9485006404991980222, 0.9666851417651760592 ) ) 
 REPRESENTATION_ITEM ( '' )  );
#28180 = CARTESIAN_POINT ( 'NONE',  ( 116.1431348109119881, -10.30919188438810075, -12.61870101168855918 ) ) ;
#28181 = CARTESIAN_POINT ( 'NONE',  ( 136.6050546525240463, 0.4234926033938513634, -15.51982212705869735 ) ) ;
#28182 = AXIS2_PLACEMENT_3D ( 'NONE', #35594, #18735, #31732 ) ;
#28183 = CARTESIAN_POINT ( 'NONE',  ( 107.7738952545248310, 0.8980012041604421569, -11.00651665394454071 ) ) ;
#28184 = CARTESIAN_POINT ( 'NONE',  ( 63.12337091419462354, -3.603895683774054781, -9.393215200338314474 ) ) ;
#28185 = CARTESIAN_POINT ( 'NONE',  ( 127.0728412258224580, 0.5536521883242400133, -13.06923365641767276 ) ) ;
#28186 = CONICAL_SURFACE ( 'NONE', #2689, 2.000000000000000444, 0.9599310885968830309 ) ;
#28187 = CARTESIAN_POINT ( 'NONE',  ( 87.80477198183443477, -25.99489077589524300, -13.39321520033831625 ) ) ;
#28188 = CARTESIAN_POINT ( 'NONE',  ( 115.8027748109119841, -0.4660016031367893996, -10.09054647747474043 ) ) ;
#28189 = CARTESIAN_POINT ( 'NONE',  ( 137.2528433483957997, -10.12362414824511347, -13.50737840558690017 ) ) ;
#28190 = CARTESIAN_POINT ( 'NONE',  ( 124.6894688159050872, -8.253847584685239269, -17.09290432062678278 ) ) ;
#28191 = DIRECTION ( 'NONE',  ( 1.000000000000000000, 0.000000000000000000, -0.000000000000000000 ) ) ;
#28192 = ADVANCED_FACE ( 'NONE', ( #38676 ), #24784, .T. ) ;
#28193 = FACE_OUTER_BOUND ( 'NONE', #20759, .T. ) ;
#28194 = CARTESIAN_POINT ( 'NONE',  ( 116.3860827545247787, -6.936859964151250502, -8.388885654883777576 ) ) ;
#28195 = CARTESIAN_POINT ( 'NONE',  ( 121.9491998309151057, -2.215723800389698184, -18.16877924232191788 ) ) ;
#28196 = LINE ( 'NONE', #42102, #28231 ) ;
#28197 = CARTESIAN_POINT ( 'NONE',  ( 67.37136766119182596, -67.53150897494617766, -41.09057840265009531 ) ) ;
#28200 = CARTESIAN_POINT ( 'NONE',  ( 116.2565881442452991, -9.261995988541697145, -16.69588392320189030 ) ) ;
#28199 = B_SPLINE_CURVE_WITH_KNOTS ( 'NONE', 3,
 ( #31268, #30832, #41, #13954, #16937, #35116, #17379, #21239, #17597, #34677 ),
 .UNSPECIFIED., .F., .F.,
 ( 4, 3, 3, 4 ),
 ( 0.000000000000000000, 1.415135068341309975E-06, 2.830270136676894854E-06, 5.507324299894169413E-06 ),
 .UNSPECIFIED. ) ;
#28198 = CARTESIAN_POINT ( 'NONE',  ( 61.63318325272354770, -19.46990085680238636, -19.39321520033831447 ) ) ;
#28201 = CYLINDRICAL_SURFACE ( 'NONE', #36572, 1.999999999999999778 ) ;
#28202 = CARTESIAN_POINT ( 'NONE',  ( 119.1496481442453046, -6.222761293078241884, -8.102969835052219238 ) ) ;
#28203 = EDGE_LOOP ( 'NONE', ( #25340, #33710, #8535, #36453 ) ) ;
#28204 = CARTESIAN_POINT ( 'NONE',  ( 122.0226922641554523, -8.548534124195553474, -17.65096007659764510 ) ) ;
#28205 = CARTESIAN_POINT ( 'NONE',  ( 121.3052614775786111, -1.834011780172310813, -8.268836392978581529 ) ) ;
#28206 = CARTESIAN_POINT ( 'NONE',  ( 114.4413952545248350, -9.868328341294098749, -15.46607636864997204 ) ) ;
#28207 = CARTESIAN_POINT ( 'NONE',  ( 114.7249681442453237, -9.565557343593413364, -10.61323700422348004 ) ) ;
#28208 = CARTESIAN_POINT ( 'NONE',  ( 113.1933481442453058, -5.574606645277164318, -18.38911715685844683 ) ) ;
#28209 = CARTESIAN_POINT ( 'NONE',  ( 70.19189222814998175, -59.47700027789979060, -36.99360193826534271 ) ) ;
#28210 = CARTESIAN_POINT ( 'NONE',  ( 114.5108483795247878, -0.7896495226426338832, -9.318865927141430916 ) ) ;
#28211 = CARTESIAN_POINT ( 'NONE',  ( 121.2485348109119769, -8.899110576539710493, -16.42337572283490132 ) ) ;
#28212 = CARTESIAN_POINT ( 'NONE',  ( 121.1350814775786233, -9.859900752359378018, -12.68260735090039759 ) ) ;
#28213 = CARTESIAN_POINT ( 'NONE',  ( 114.4980614775786734, -2.084020599724388578, -8.691656652584157428 ) ) ;
#28214 = DIRECTION ( 'NONE',  ( 0.2768435750659264949, 0.3568721902840676363, -0.8921882507333129819 ) ) ;
#28215 = LINE ( 'NONE', #35010, #37164 ) ;
#28216 = CIRCLE ( 'NONE', #1962, 2.999999999999999556 ) ;
#28217 = CARTESIAN_POINT ( 'NONE',  ( 111.3160046295247838, -4.863998795839590272, -18.39754474579285315 ) ) ;
#28218 = DIRECTION ( 'NONE',  ( 0.000000000000000000, 0.000000000000000000, 1.000000000000000000 ) ) ;
#28219 = CARTESIAN_POINT ( 'NONE',  ( 116.1431348109119881, -10.30919188438810075, -12.61870101168855918 ) ) ;
#28220 = CARTESIAN_POINT ( 'NONE',  ( 115.7460481442453357, 0.9020085738987339008, -11.91225656197089222 ) ) ;
#28221 = CARTESIAN_POINT ( 'NONE',  ( 111.4549108795247747, -8.938348069036489818, -9.318865927141430916 ) ) ;
#28222 = CARTESIAN_POINT ( 'NONE',  ( 114.3846081442453197, -10.63000616557722466, -14.87417383870573495 ) ) ;
#28223 = VERTEX_POINT ( 'NONE', #18401 ) ;
#28224 = UNCERTAINTY_MEASURE_WITH_UNIT (LENGTH_MEASURE( 1.000000000000000082E-05 ), #35773, 'distance_accuracy_value', 'NONE');
#28225 = LINE ( 'NONE', #32070, #40742 ) ;
#28226 = CARTESIAN_POINT ( 'NONE',  ( 121.5888948109119809, -10.30919188438810075, -12.61870101168855918 ) ) ;
#28227 = CARTESIAN_POINT ( 'NONE',  ( 114.9518748109119883, -1.834011780172310813, -8.268836392978581529 ) ) ;
#28228 = CARTESIAN_POINT ( 'NONE',  ( 121.0783548109119749, -9.565557343593413364, -10.61323700422348004 ) ) ;
#28229 = CARTESIAN_POINT ( 'NONE',  ( 111.5482748109120053, -0.1624402480850797581, -16.17319339645315424 ) ) ;
#28230 = CARTESIAN_POINT ( 'NONE',  ( 120.5678148109119832, -8.166667518702819706, -8.995218007635861213 ) ) ;
#28231 = VECTOR ( 'NONE', #31372, 1000.000000000000000 ) ;
#28232 = CARTESIAN_POINT ( 'NONE',  ( 113.6774108795247997, -8.938348069036489818, -9.318865927141430916 ) ) ;
#28233 = CARTESIAN_POINT ( 'NONE',  ( 115.9729548109119861, -3.505236298600246325, -18.68346056562440793 ) ) ;
#28234 = DIRECTION ( 'NONE',  ( 0.000000000000000000, -0.9242245927363028635, -0.3818493186865930533 ) ) ;
#28235 = EDGE_LOOP ( 'NONE', ( #34754, #18973 ) ) ;
#28236 = CARTESIAN_POINT ( 'NONE',  ( 122.6099748109119929, -9.261995988541697145, -16.69588392320189030 ) ) ;
#28237 = CARTESIAN_POINT ( 'NONE',  ( 119.2631014775786298, 0.2603800115204892296, -16.42320221600525088 ) ) ;
#28238 = ORIENTED_EDGE ( 'NONE', *, *, #41477, .F. ) ;
#28239 = CARTESIAN_POINT ( 'NONE',  ( 114.7886608795247696, -8.938348069036489818, -9.318865927141430916 ) ) ;
#28240 = CARTESIAN_POINT ( 'NONE',  ( 124.6521348109119884, -1.561330072975668948, -17.79121239304076951 ) ) ;
#28242 = CARTESIAN_POINT ( 'NONE',  ( 70.19189222814998175, -51.68868231262963775, -33.87830190084585524 ) ) ;
#28241 = CONICAL_SURFACE ( 'NONE', #40615, 1.610000000000000986, 0.9599310885968765916 ) ;
#28243 = CARTESIAN_POINT ( 'NONE',  ( 116.7104014775786425, -8.899110576539710493, -16.42337572283490132 ) ) ;
#28244 = CYLINDRICAL_SURFACE ( 'NONE', #6970, 5.132259260909266985 ) ;
#28245 = CARTESIAN_POINT ( 'NONE',  ( 121.4754414775786131, -1.833838273342659697, -17.42832698103878286 ) ) ;
#28246 = CARTESIAN_POINT ( 'NONE',  ( 121.1350814775786233, 0.5811942927096136469, -14.16772938898805378 ) ) ;
#28247 = CARTESIAN_POINT ( 'NONE',  ( 122.9503348109119827, -9.859900752359378018, -12.68260735090039759 ) ) ;
#28248 = CARTESIAN_POINT ( 'NONE',  ( 117.0049627575976814, 0.4002175711165650851, -14.64321520033831447 ) ) ;
#28249 = CARTESIAN_POINT ( 'NONE',  ( 120.2274548109119934, -9.859900752359378018, -12.68260735090039759 ) ) ;
#28250 = FACE_OUTER_BOUND ( 'NONE', #14930, .T. ) ;
#28251 = CARTESIAN_POINT ( 'NONE',  ( 116.1431348109119881, -10.30919188438810075, -12.61870101168855918 ) ) ;
#28252 = LINE ( 'NONE', #18662, #41666 ) ;
#28253 = CARTESIAN_POINT ( 'NONE',  ( 119.5467348109119712, -5.574606645277164318, -18.38911715685844683 ) ) ;
#28254 = ORIENTED_EDGE ( 'NONE', *, *, #8425, .T. ) ;
#28255 = CARTESIAN_POINT ( 'NONE',  ( 118.4122014775786340, 0.5811942927096110934, -14.16772938898807510 ) ) ;
#28256 = CARTESIAN_POINT ( 'NONE',  ( 114.3024890045248156, -9.868328341294098749, -11.32035403202665869 ) ) ;
#28257 = DIRECTION ( 'NONE',  ( 0.000000000000000000, 0.000000000000000000, 1.000000000000000000 ) ) ;
#28258 = DIRECTION ( 'NONE',  ( 1.000000000000000000, 0.000000000000000000, -0.000000000000000000 ) ) ;
#28259 = EDGE_CURVE ( 'NONE', #40326, #39449, #7442, .T. ) ;
#28260 = DIRECTION ( 'NONE',  ( 0.9609149988134837450, -0.1028163501681639419, 0.2570431154366518145 ) ) ;
#28261 = CARTESIAN_POINT ( 'NONE',  ( 124.0848681442452772, -4.089484607189486809, -7.948022111789456723 ) ) ;
#28262 = VERTEX_POINT ( 'NONE', #14077 ) ;
#28263 = CARTESIAN_POINT ( 'NONE',  ( 126.2184548109108420, -7.957993755341922437, -9.463799409162998444 ) ) ;
#28264 = CARTESIAN_POINT ( 'NONE',  ( 120.3976348109119812, -7.643976991954077427, -18.09477374809248928 ) ) ;
#28265 = CARTESIAN_POINT ( 'NONE',  ( 87.68939540009954214, -25.23119213852205789, -15.24166438581092109 ) ) ;
#28266 = CARTESIAN_POINT ( 'NONE',  ( 64.60369908702583075, -13.80855579193262805, -17.86746305170717619 ) ) ;
#28267 = CARTESIAN_POINT ( 'NONE',  ( 126.1270281442452870, -10.30919188438810075, -12.61870101168855918 ) ) ;
#28268 = CARTESIAN_POINT ( 'NONE',  ( 112.0105358795248804, -8.402594152722688392, -9.854619843455216355 ) ) ;
#28269 = CARTESIAN_POINT ( 'NONE',  ( 123.2184548109119788, -2.211393927326563702, -15.67656524173425758 ) ) ;
#28270 = ORIENTED_EDGE ( 'NONE', *, *, #44062, .T. ) ;
#28271 = CARTESIAN_POINT ( 'NONE',  ( 113.7606148109119886, -1.561330072975668060, -17.79121239304076596 ) ) ;
#28272 = CARTESIAN_POINT ( 'NONE',  ( 124.9357681442453014, -7.643976991954077427, -18.09477374809248928 ) ) ;
#28273 = CARTESIAN_POINT ( 'NONE',  ( 121.9859814775786333, 0.2603800115204892296, -16.42320221600525088 ) ) ;
#28274 = CARTESIAN_POINT ( 'NONE',  ( 117.7882081442453170, -3.505236298600246325, -18.68346056562440793 ) ) ;
#28275 = CIRCLE ( 'NONE', #43655, 1.199999999999999512 ) ;
#28276 = CARTESIAN_POINT ( 'NONE',  ( 126.5621572004008755, -3.449551328269489403, -8.418040804988667247 ) ) ;
#28277 = CARTESIAN_POINT ( 'NONE',  ( 123.6310548109119765, -5.638512984488999180, -18.83840828888717311 ) ) ;
#28278 = CARTESIAN_POINT ( 'NONE',  ( 111.7857214775786474, -4.159894987975828684, -8.443039665293898821 ) ) ;
#28279 = DIRECTION ( 'NONE',  ( 0.000000000000000000, 0.000000000000000000, 1.000000000000000000 ) ) ;
#28280 = DIRECTION ( 'NONE',  ( 0.000000000000000000, 0.000000000000000000, 1.000000000000000000 ) ) ;
#28281 = CARTESIAN_POINT ( 'NONE',  ( 125.7299414775786346, -10.15424416112533912, -14.75197769757731336 ) ) ;
#28282 = ORIENTED_EDGE ( 'NONE', *, *, #27007, .T. ) ;
#28283 = CARTESIAN_POINT ( 'NONE',  ( 116.5976908158778826, -9.866790291921139655, -13.46630915925490690 ) ) ;
#28284 = CARTESIAN_POINT ( 'NONE',  ( 121.2485348109119769, -0.4660016031367893996, -10.09054647747474043 ) ) ;
#28285 = CARTESIAN_POINT ( 'NONE',  ( 135.9690293846555278, -8.515994457645518878, -18.06058892513630099 ) ) ;
#28286 = ORIENTED_EDGE ( 'NONE', *, *, #22760, .F. ) ;
#28287 = DIRECTION ( 'NONE',  ( -0.7871354856660162103, -0.4483307682966942709, -0.4235767337848251879 ) ) ;
#28288 = CARTESIAN_POINT ( 'NONE',  ( 122.3263414775786373, -6.344957434206665248, -7.627207830600338134 ) ) ;
#28289 = CARTESIAN_POINT ( 'NONE',  ( 109.5796765045248122, -7.250697342233347165, -19.15521520033831138 ) ) ;
#28290 = CARTESIAN_POINT ( 'NONE',  ( 120.7379948109119709, 0.4262465694468514643, -12.03445270309931736 ) ) ;
#28291 = ORIENTED_EDGE ( 'NONE', *, *, #35301, .F. ) ;
#28292 = CARTESIAN_POINT ( 'NONE',  ( 116.1431348109119881, -10.30919188438810075, -12.61870101168855918 ) ) ;
#28293 = DIRECTION ( 'NONE',  ( -1.000000000000000000, 0.000000000000000000, 0.000000000000000000 ) ) ;
#28294 = CARTESIAN_POINT ( 'NONE',  ( 112.5649393026123022, -1.179503403430478770, -17.05068175419387799 ) ) ;
#28295 = CARTESIAN_POINT ( 'NONE',  ( 59.41811746136757222, -12.82955349636864639, -17.39310469171629947 ) ) ;
#28296 = CARTESIAN_POINT ( 'NONE',  ( 125.9001214775786224, -4.089484607189486809, -7.948022111789456723 ) ) ;
#28297 = DIRECTION ( 'NONE',  ( -1.000000000000000000, 0.000000000000000000, 0.000000000000000000 ) ) ;
#28298 = LINE ( 'NONE', #41987, #3347 ) ;
#28299 = CARTESIAN_POINT ( 'NONE',  ( 124.5954081442453116, -3.383040157471821630, -19.15922257007629170 ) ) ;
#28301 = CARTESIAN_POINT ( 'NONE',  ( 121.8725281442453223, -6.222761293078241884, -8.102969835052219238 ) ) ;
#28300 = CARTESIAN_POINT ( 'NONE',  ( 123.6877814775786533, -3.383040157471821630, -19.15922257007629170 ) ) ;
#28302 = CARTESIAN_POINT ( 'NONE',  ( 118.5256548109119876, -8.899110576539710493, -16.42337572283490132 ) ) ;
#28303 = DIRECTION ( 'NONE',  ( -0.000000000000000000, -0.9284778069183721172, -0.3713878862591650232 ) ) ;
#28304 = CARTESIAN_POINT ( 'NONE',  ( 117.1642148109119859, -9.261995988541697145, -16.69588392320189030 ) ) ;
#28305 = ORIENTED_EDGE ( 'NONE', *, *, #14186, .T. ) ;
#28306 = CARTESIAN_POINT ( 'NONE',  ( 122.8176765460471813, -2.191907684172563986, -18.20049396185734025 ) ) ;
#28307 = CARTESIAN_POINT ( 'NONE',  ( 125.5492214775786550, -6.210324830719740064, -8.151390318758597431 ) ) ;
#28308 = CARTESIAN_POINT ( 'NONE',  ( 112.7050671295247923, 0.1403307496149613920, -13.39321520033831447 ) ) ;
#28309 = CARTESIAN_POINT ( 'NONE',  ( 106.8015515045248378, -6.936859964151250502, -18.39754474579286025 ) ) ;
#28310 = CARTESIAN_POINT ( 'NONE',  ( 113.5385046295247804, -4.863998795839590272, -18.39754474579285315 ) ) ;
#28311 = CARTESIAN_POINT ( 'NONE',  ( 124.4819548109119722, -7.893985811506177619, -18.51759400769804742 ) ) ;
#28312 = CARTESIAN_POINT ( 'NONE',  ( 112.7395348109119766, -5.638512984488999180, -18.83840828888717311 ) ) ;
#28313 = EDGE_LOOP ( 'NONE', ( #45103, #37526, #1306, #44290, #11685, #545 ) ) ;
#28314 = CARTESIAN_POINT ( 'NONE',  ( 112.0588148109119828, -9.859900752359374465, -12.68260735090039404 ) ) ;
#28315 = CARTESIAN_POINT ( 'NONE',  ( 111.5938171295247940, -10.62599879583958540, -13.39321520033831447 ) ) ;
#28316 = FACE_BOUND ( 'NONE', #30306, .T. ) ;
#28317 = CARTESIAN_POINT ( 'NONE',  ( 122.2128881442453263, -1.834011780172310813, -8.268836392978581529 ) ) ;
#28318 = CARTESIAN_POINT ( 'NONE',  ( 123.1772414775786189, -4.089484607189486809, -7.948022111789456723 ) ) ;
#28319 = CARTESIAN_POINT ( 'NONE',  ( 79.14411413026581954, 4.892312988188566081, -5.897268129732760045 ) ) ;
#28320 = CARTESIAN_POINT ( 'NONE',  ( 117.6747548109119919, -1.834011780172310813, -8.268836392978581529 ) ) ;
#28321 = FACE_OUTER_BOUND ( 'NONE', #1572, .T. ) ;
#28322 = CARTESIAN_POINT ( 'NONE',  ( 111.8021765045248372, -2.791137627527939813, -8.388885654883777576 ) ) ;
#28323 = ORIENTED_EDGE ( 'NONE', *, *, #42975, .T. ) ;
#28324 = CARTESIAN_POINT ( 'NONE',  ( 126.4852516627942265, -7.433467366253567299, -8.949158261980540985 ) ) ;
#28325 = CARTESIAN_POINT ( 'NONE',  ( 113.9875214775786532, -8.899110576539710493, -16.42337572283490132 ) ) ;
#28326 = CARTESIAN_POINT ( 'NONE',  ( 112.0588148109119828, 0.5811942927096154232, -14.16772938898807155 ) ) ;
#28327 = CARTESIAN_POINT ( 'NONE',  ( 113.9552233795247815, -8.938348069036489818, -17.46756447353520159 ) ) ;
#28328 = DIRECTION ( 'NONE',  ( 0.000000000000000000, 0.000000000000000000, 1.000000000000000000 ) ) ;
#28329 = CARTESIAN_POINT ( 'NONE',  ( 123.8579614775786126, -9.859900752359378018, -12.68260735090039759 ) ) ;
#28330 = CARTESIAN_POINT ( 'NONE',  ( 121.1918081442452859, -10.15424416112533912, -14.75197769757731336 ) ) ;
#28331 = CARTESIAN_POINT ( 'NONE',  ( 125.6732148109119862, 0.5811942927096110934, -14.16772938898807510 ) ) ;
#28332 = EDGE_LOOP ( 'NONE', ( #10490, #8158 ) ) ;
#28333 = LINE ( 'NONE', #34915, #9620 ) ;
#28334 = CIRCLE ( 'NONE', #14493, 2.000000000000001776 ) ;
#28335 = DIRECTION ( 'NONE',  ( -0.000000000000000000, -0.9284778069183718952, -0.3713878862591649677 ) ) ;
#28336 = CARTESIAN_POINT ( 'NONE',  ( 115.1787814775786387, -0.1624402480850797581, -16.17319339645315424 ) ) ;
#28337 = VERTEX_POINT ( 'NONE', #4250 ) ;
#28338 = CARTESIAN_POINT ( 'NONE',  ( 126.4915402333597854, -9.314160179844931164, -15.95839630942495724 ) ) ;
#28339 = DIRECTION ( 'NONE',  ( 0.000000000000000000, -0.3818493186865927203, 0.9242245927363029745 ) ) ;
#28340 = CARTESIAN_POINT ( 'NONE',  ( 111.3160046295247838, -4.863998795839590272, -18.39754474579285315 ) ) ;
#28341 = CARTESIAN_POINT ( 'NONE',  ( 125.1059481442452750, -1.833838273342660141, -17.42832698103878286 ) ) ;
#28342 = ORIENTED_EDGE ( 'NONE', *, *, #19486, .T. ) ;
#28343 = CARTESIAN_POINT ( 'NONE',  ( 117.9016614775786280, -0.1624402480850797581, -16.17319339645315424 ) ) ;
#28344 = CARTESIAN_POINT ( 'NONE',  ( 112.4559014775786778, -0.1624402480850797581, -16.17319339645315424 ) ) ;
#28345 = DIRECTION ( 'NONE',  ( -0.000000000000000000, -0.9284778069183720062, -0.3713878862591650232 ) ) ;
#28346 = EDGE_CURVE ( 'NONE', #25605, #20709, #35705, .T. ) ;
#28347 = CARTESIAN_POINT ( 'NONE',  ( 122.5215798109119874, -2.173413727453600508, -8.297982527556802879 ) ) ;
#28348 = ORIENTED_EDGE ( 'NONE', *, *, #11927, .F. ) ;
#28349 = CARTESIAN_POINT ( 'NONE',  ( 61.63318325272354770, -19.46990085680238636, -10.89321520033831447 ) ) ;
#28350 = CARTESIAN_POINT ( 'NONE',  ( 119.7434548109119703, -2.530624428477246113, -8.966368849971939170 ) ) ;
#28351 = CARTESIAN_POINT ( 'NONE',  ( 109.3018640045248304, -10.62599879583958717, -11.00651665394454604 ) ) ;
#28352 = CARTESIAN_POINT ( 'NONE',  ( 113.2500748109119968, -6.344957434206662583, -7.627207830600332805 ) ) ;
#28353 = CARTESIAN_POINT ( 'NONE',  ( 112.0020881442453344, 0.2603800115204892296, -16.42320221600525088 ) ) ;
#28354 = CARTESIAN_POINT ( 'NONE',  ( 119.3198281442452924, -9.859900752359374465, -12.68260735090039404 ) ) ;
#28355 = DIRECTION ( 'NONE',  ( 0.000000000000000000, -0.6004852223388319477, 0.7996358532186282897 ) ) ;
#28356 = ORIENTED_EDGE ( 'NONE', *, *, #5258, .F. ) ;
#28357 = CARTESIAN_POINT ( 'NONE',  ( 117.6180281442453150, -8.899110576539710493, -16.42337572283490132 ) ) ;
#28358 = DIRECTION ( 'NONE',  ( 0.7871354856660198740, 0.4483307682966886643, 0.4235767337848242442 ) ) ;
#28359 = CARTESIAN_POINT ( 'NONE',  ( 71.36400868967236022, -24.42718413923373788, -4.893215200338314474 ) ) ;
#28360 = CARTESIAN_POINT ( 'NONE',  ( 115.8999108795247821, -8.938348069036489818, -9.318865927141430916 ) ) ;
#28361 = CIRCLE ( 'NONE', #29111, 2.999999999999999556 ) ;
#28362 = CARTESIAN_POINT ( 'NONE',  ( 113.2500748109119968, -6.344957434206662583, -7.627207830600332805 ) ) ;
#28363 = ORIENTED_EDGE ( 'NONE', *, *, #36724, .F. ) ;
#28364 = CARTESIAN_POINT ( 'NONE',  ( 116.5402214775786405, 0.2603800115204892296, -16.42320221600525088 ) ) ;
#28365 = VECTOR ( 'NONE', #33734, 1000.000000000000000 ) ;
#28366 = CARTESIAN_POINT ( 'NONE',  ( 87.44708369096657918, -21.99489077589588604, -7.893215200338315363 ) ) ;
#28367 = CARTESIAN_POINT ( 'NONE',  ( 112.1494421295248003, 0.8980012041604618078, -13.39321520033831447 ) ) ;
#28368 = CARTESIAN_POINT ( 'NONE',  ( 112.1722681442453222, -0.4660016031367893996, -10.09054647747474043 ) ) ;
#28369 = CARTESIAN_POINT ( 'NONE',  ( 114.7249681442453237, 0.2603800115204892296, -16.42320221600525088 ) ) ;
#28370 = CARTESIAN_POINT ( 'NONE',  ( 127.0553483106841810, -10.27339372193082312, -13.70636429400185285 ) ) ;
#28371 = DIRECTION ( 'NONE',  ( -0.5735764363510450492, -0.3127926500124816878, 0.7570804645221038687 ) ) ;
#28372 = CARTESIAN_POINT ( 'NONE',  ( 109.3713171295247832, 0.1403307496149613920, -13.39321520033831447 ) ) ;
#28373 = ADVANCED_FACE ( 'NONE', ( #28886 ), #21589, .T. ) ;
#28374 = ORIENTED_EDGE ( 'NONE', *, *, #13019, .F. ) ;
#28375 = CARTESIAN_POINT ( 'NONE',  ( 116.2471765045247594, -7.250697342233347165, -19.15521520033830427 ) ) ;
#28376 = CARTESIAN_POINT ( 'NONE',  ( 109.2294861558825119, -6.900259341933140611, -18.27081374760126664 ) ) ;
#28377 = CARTESIAN_POINT ( 'NONE',  ( 115.7460481442453357, -10.15424416112533912, -14.75197769757731336 ) ) ;
#28378 = CARTESIAN_POINT ( 'NONE',  ( 64.57113367631538381, -13.11585569015068664, -11.30697229492609068 ) ) ;
#28379 = CARTESIAN_POINT ( 'NONE',  ( 115.4831921295247952, -9.868328341294093420, -13.39321520033831447 ) ) ;
#28380 = CARTESIAN_POINT ( 'NONE',  ( 110.7603796295247918, -4.863998795839590272, -19.15521520033831493 ) ) ;
#28381 = CARTESIAN_POINT ( 'NONE',  ( 126.9115046738381096, -5.096111321019845875, -8.051413078099821874 ) ) ;
#28382 = CARTESIAN_POINT ( 'NONE',  ( 125.1626748109119802, -9.988377603198980381, -10.36322818467138518 ) ) ;
#28383 = CARTESIAN_POINT ( 'NONE',  ( 70.19189222814998175, -60.04498257489500190, -37.22079287717834717 ) ) ;
#28384 = EDGE_CURVE ( 'NONE', #20709, #39064, #3227, .T. ) ;
#28385 = CARTESIAN_POINT ( 'NONE',  ( 125.6164881442453094, 0.2603800115204892296, -16.42320221600525088 ) ) ;
#28386 = CARTESIAN_POINT ( 'NONE',  ( 117.5045748109119756, 0.5811942927096110934, -14.16772938898807510 ) ) ;
#28387 = ORIENTED_EDGE ( 'NONE', *, *, #7278, .F. ) ;
#28388 = EDGE_CURVE ( 'NONE', #37757, #41378, #41542, .T. ) ;
#28389 = CARTESIAN_POINT ( 'NONE',  ( 115.2355081442453155, 0.1319031606808879209, -14.10382304977623669 ) ) ;
#28390 = CARTESIAN_POINT ( 'NONE',  ( 111.7751814775786556, -7.893985811506177619, -18.51759400769804742 ) ) ;
#28391 = CARTESIAN_POINT ( 'NONE',  ( 116.3133148109119759, -7.893985811506177619, -18.51759400769804742 ) ) ;
#28392 = CARTESIAN_POINT ( 'NONE',  ( 115.1787814775786387, -0.1624402480850797581, -16.17319339645315424 ) ) ;
#28393 = ORIENTED_EDGE ( 'NONE', *, *, #41493, .F. ) ;
#28394 = CARTESIAN_POINT ( 'NONE',  ( 122.0427081442452817, -9.859900752359378018, -12.68260735090039759 ) ) ;
#28395 = ADVANCED_FACE ( 'NONE', ( #15647 ), #18213, .T. ) ;
#28396 = CARTESIAN_POINT ( 'NONE',  ( 115.6325948109119821, 0.2603800115204892296, -16.42320221600525088 ) ) ;
#28397 = AXIS2_PLACEMENT_3D ( 'NONE', #26006, #29419, #15742 ) ;
#28398 = CARTESIAN_POINT ( 'NONE',  ( 137.4531891128992811, 0.2004337171367315540, -13.63196781300515781 ) ) ;
#28399 = CARTESIAN_POINT ( 'NONE',  ( 109.1629577545248395, -7.250697342233347165, -7.631215200338321125 ) ) ;
#28400 = EDGE_CURVE ( 'NONE', #25805, #19894, #25688, .T. ) ;
#28401 = EDGE_CURVE ( 'NONE', #16340, #14378, #32776, .T. ) ;
#28402 = ADVANCED_FACE ( 'NONE', ( #36155 ), #21234, .T. ) ;
#28403 = CARTESIAN_POINT ( 'NONE',  ( 62.74499803204670911, -14.59121584192012655, -9.399563555836040862 ) ) ;
#28404 = CARTESIAN_POINT ( 'NONE',  ( 126.4552522132384667, 0.2524518362947308914, -13.53592757502032917 ) ) ;
#28405 = DIRECTION ( 'NONE',  ( -0.000000000000000000, -0.9284778069183718952, -0.3713878862591649677 ) ) ;
#28406 = AXIS2_PLACEMENT_3D ( 'NONE', #22147, #28771, #15302 ) ;
#28407 = CARTESIAN_POINT ( 'NONE',  ( 114.4413348109119823, -9.261995988541697145, -16.69588392320189030 ) ) ;
#28408 = DIRECTION ( 'NONE',  ( -0.5735764363510446051, 0.3127926500124816878, -0.7570804645221042017 ) ) ;
#28409 = CARTESIAN_POINT ( 'NONE',  ( 114.2144281442453178, -1.833838273342658809, -17.42832698103878286 ) ) ;
#28410 = CARTESIAN_POINT ( 'NONE',  ( 69.69189222814998175, -41.76310523276723785, -4.893215200338314474 ) ) ;
#28411 = CARTESIAN_POINT ( 'NONE',  ( 112.2841521944299785, 0.6269505268395592079, -12.14321520033829849 ) ) ;
#28412 = CARTESIAN_POINT ( 'NONE',  ( 115.8304577545247582, -2.791137627527939813, -18.39754474579286025 ) ) ;
#28413 = CARTESIAN_POINT ( 'NONE',  ( 112.1722681442453222, -8.899110576539710493, -16.42337572283490132 ) ) ;
#28414 = CARTESIAN_POINT ( 'NONE',  ( 70.19189222814998175, -54.83461124330791847, -35.13666250696951465 ) ) ;
#28415 = LINE ( 'NONE', #14059, #15838 ) ;
#28417 = CARTESIAN_POINT ( 'NONE',  ( 118.0151148109119816, -10.63000616557722466, -14.87417383870573495 ) ) ;
#28416 = CARTESIAN_POINT ( 'NONE',  ( 124.7440798109119697, -7.200787124940195127, -17.81845355600763625 ) ) ;
#28418 = CARTESIAN_POINT ( 'NONE',  ( 124.8223148109119762, -10.15424416112533912, -14.75197769757731336 ) ) ;
#28419 = CARTESIAN_POINT ( 'NONE',  ( 119.2631014775786298, -9.565557343593413364, -10.61323700422348004 ) ) ;
#28420 = CARTESIAN_POINT ( 'NONE',  ( 113.0798948109119948, -8.899110576539710493, -16.42337572283490132 ) ) ;
#28421 = ORIENTED_EDGE ( 'NONE', *, *, #24251, .T. ) ;
#28422 = CARTESIAN_POINT ( 'NONE',  ( 86.34560043013698305, -9.320000780048239619, -8.143215200338314474 ) ) ;
#28423 = CARTESIAN_POINT ( 'NONE',  ( 124.7088614775786226, 0.2603800115204892296, -16.42320221600525088 ) ) ;
#28424 = CARTESIAN_POINT ( 'NONE',  ( 113.5385046295247804, -4.863998795839590272, -18.39754474579285315 ) ) ;
#28425 = CARTESIAN_POINT ( 'NONE',  ( 117.7882081442453170, -3.505236298600246325, -18.68346056562440793 ) ) ;
#28426 = CARTESIAN_POINT ( 'NONE',  ( 115.3489614775786407, -0.8288870151387760510, -10.36305467784173118 ) ) ;
#28427 = CARTESIAN_POINT ( 'NONE',  ( 85.92326454629504440, -27.42010911645014204, -8.655686125604109549 ) ) ;
#28428 = CARTESIAN_POINT ( 'NONE',  ( 114.7886608795247696, -8.938348069036489818, -9.318865927141430916 ) ) ;
#28429 = CARTESIAN_POINT ( 'NONE',  ( 121.1918081442452859, -10.15424416112533912, -14.75197769757731336 ) ) ;
#28430 = CARTESIAN_POINT ( 'NONE',  ( 124.1415948109119540, -3.505236298600246325, -18.68346056562440793 ) ) ;
#28431 = CARTESIAN_POINT ( 'NONE',  ( 114.6682414775786469, -7.894159318335810305, -9.358103419637833653 ) ) ;
#28432 = VECTOR ( 'NONE', #28358, 1000.000000000000227 ) ;
#28433 = CARTESIAN_POINT ( 'NONE',  ( 109.2294400832953301, -1.120989073033315409, -9.512730530502590653 ) ) ;
#28434 = CARTESIAN_POINT ( 'NONE',  ( 121.8270485609119760, -10.36940331770106916, -15.09355782777062061 ) ) ;
#28435 = CARTESIAN_POINT ( 'NONE',  ( 113.6774108795247997, -8.938348069036489818, -9.318865927141430916 ) ) ;
#28436 = LINE ( 'NONE', #11108, #22567 ) ;
#28437 = CARTESIAN_POINT ( 'NONE',  ( 115.9729548109119861, -6.344957434206662583, -7.627207830600332805 ) ) ;
#28438 = CARTESIAN_POINT ( 'NONE',  ( 113.4769814775786330, -10.63000616557722466, -14.87417383870573495 ) ) ;
#28439 = CARTESIAN_POINT ( 'NONE',  ( 113.2606921295247702, 0.8980012041604618078, -13.39321520033831447 ) ) ;
#28440 =( BOUNDED_CURVE ( )  B_SPLINE_CURVE ( 3, ( #37020, #16069, #5116, #12889 ),
 .UNSPECIFIED., .F., .F. ) 
 B_SPLINE_CURVE_WITH_KNOTS ( ( 4, 4 ),
 ( 4.712388980384689674, 5.608053774242550027 ),
 .UNSPECIFIED. ) 
 CURVE ( )  GEOMETRIC_REPRESENTATION_ITEM ( )  RATIONAL_B_SPLINE_CURVE ( ( 1.000000000000000000, 0.9342585459106650392, 0.9342585459106650392, 1.000000000000000000 ) ) 
 REPRESENTATION_ITEM ( '' )  );
#28441 = CARTESIAN_POINT ( 'NONE',  ( 112.1722681442453222, -0.4660016031367893996, -10.09054647747474043 ) ) ;
#28442 = VERTEX_POINT ( 'NONE', #4923 ) ;
#28443 = CARTESIAN_POINT ( 'NONE',  ( 113.0188248073892794, -1.081026697600518283, -17.18181821144401766 ) ) ;
#28444 = CARTESIAN_POINT ( 'NONE',  ( 123.9714148109119805, -0.4660016031367893996, -10.09054647747474043 ) ) ;
#28445 = AXIS2_PLACEMENT_3D ( 'NONE', #34963, #6966, #27945 ) ;
#28446 = CARTESIAN_POINT ( 'NONE',  ( 114.8384214775786489, 0.9020085738987339008, -11.91225656197089222 ) ) ;
#28447 = CARTESIAN_POINT ( 'NONE',  ( 122.6667014775786413, -2.084020599724406786, -8.691656652584148546 ) ) ;
#28448 = FILL_AREA_STYLE ('',( #38244 ) ) ;
#28449 = AXIS2_PLACEMENT_3D ( 'NONE', #22852, #36743, #5511 ) ;
#28450 = CARTESIAN_POINT ( 'NONE',  ( 124.3117748109119844, -10.30919188438810075, -12.61870101168855918 ) ) ;
#28451 = CARTESIAN_POINT ( 'NONE',  ( 120.7379948109119709, -10.63000616557722466, -14.87417383870573495 ) ) ;
#28452 = ADVANCED_FACE ( 'NONE', ( #40498 ), #7338, .T. ) ;
#28453 = CARTESIAN_POINT ( 'NONE',  ( 112.9828796295247884, -4.863998795839590272, -19.15521520033831493 ) ) ;
#28454 = CARTESIAN_POINT ( 'NONE',  ( 116.0864081442453113, -0.1624402480850797581, -16.17319339645315424 ) ) ;
#28455 = B_SPLINE_CURVE_WITH_KNOTS ( 'NONE', 3,
 ( #42131, #14757, #25248, #38459, #10891, #14529, #4028, #28443, #24790, #28893 ),
 .UNSPECIFIED., .F., .F.,
 ( 4, 3, 3, 4 ),
 ( 4.336808689942019662E-19, 0.0001671877548681264863, 0.0003343755096277690043, 0.0006463528481650629171 ),
 .UNSPECIFIED. ) ;
#28456 = CARTESIAN_POINT ( 'NONE',  ( 143.3676850761856940, -49.76310523276723785, -40.89321520033831092 ) ) ;
#28457 = ORIENTED_EDGE ( 'NONE', *, *, #38798, .F. ) ;
#28458 = CARTESIAN_POINT ( 'NONE',  ( 123.3474214775786209, -9.988377603198976828, -10.36322818467138340 ) ) ;
#28459 = ADVANCED_FACE ( 'NONE', ( #32729 ), #1503, .T. ) ;
#28460 = CARTESIAN_POINT ( 'NONE',  ( 123.0772048109119652, -7.554583864224885481, -18.48844787311982785 ) ) ;
#28461 = CARTESIAN_POINT ( 'NONE',  ( 118.1285681442453068, -7.893985811506177619, -18.51759400769804742 ) ) ;
#28462 = ORIENTED_EDGE ( 'NONE', *, *, #43997, .T. ) ;
#28463 = CARTESIAN_POINT ( 'NONE',  ( 107.6349890045248401, -9.868328341294098749, -11.32035403202665869 ) ) ;
#28464 = DIRECTION ( 'NONE',  ( 1.000000000000000000, 0.000000000000000000, -0.000000000000000000 ) ) ;
#28465 = CONICAL_SURFACE ( 'NONE', #37931, 2.000000000000000444, 0.9599310885968830309 ) ;
#28466 = CARTESIAN_POINT ( 'NONE',  ( 122.7694671478583501, -3.807985514183312326, -19.09877912889401941 ) ) ;
#28467 = CARTESIAN_POINT ( 'NONE',  ( 114.3278814775786429, 0.1319031606808879209, -14.10382304977623669 ) ) ;
#28468 = CARTESIAN_POINT ( 'NONE',  ( 64.61935771200890599, -37.86087448816891765, -4.893215200338314474 ) ) ;
#28469 = EDGE_CURVE ( 'NONE', #10826, #32004, #44496, .T. ) ;
#28470 = CARTESIAN_POINT ( 'NONE',  ( 118.8092881442453290, -0.1624402480850797581, -16.17319339645315424 ) ) ;
#28471 = DIRECTION ( 'NONE',  ( -1.000000000000000000, 0.000000000000000000, 0.000000000000000000 ) ) ;
#28472 = CARTESIAN_POINT ( 'NONE',  ( 120.9081748109119872, -4.153390946401325223, -8.397313243818185668 ) ) ;
#28473 = VECTOR ( 'NONE', #42748, 1000.000000000000114 ) ;
#28474 = CARTESIAN_POINT ( 'NONE',  ( 125.1375072647520881, -10.92929117853784682, -9.105846273144043934 ) ) ;
#28475 = CARTESIAN_POINT ( 'NONE',  ( 118.3554748109119998, -9.565557343593413364, -10.61323700422348004 ) ) ;
#28476 = AXIS2_PLACEMENT_3D ( 'NONE', #19375, #33719, #33483 ) ;
#28477 = CARTESIAN_POINT ( 'NONE',  ( 113.3635281442453504, -9.988377603198976828, -10.36322818467138340 ) ) ;
#28478 = CARTESIAN_POINT ( 'NONE',  ( 119.2063748109119814, -1.561330072975668504, -17.79121239304076951 ) ) ;
#28479 = CARTESIAN_POINT ( 'NONE',  ( 113.0231681442453322, 0.9020085738987339008, -11.91225656197089222 ) ) ;
#28480 = CARTESIAN_POINT ( 'NONE',  ( 69.36136150295220659, -62.76506797251190051, -35.20400990592987966 ) ) ;
#28481 = CARTESIAN_POINT ( 'NONE',  ( 120.7379948109119709, 0.4262465694468514643, -12.03445270309931736 ) ) ;
#28482 = VERTEX_POINT ( 'NONE', #3308 ) ;
#28483 = CARTESIAN_POINT ( 'NONE',  ( 117.7882081442453170, -6.344957434206665248, -7.627207830600338134 ) ) ;
#28484 = CARTESIAN_POINT ( 'NONE',  ( 114.6497546295247929, -4.863998795839590272, -18.39754474579285315 ) ) ;
#28485 = CARTESIAN_POINT ( 'NONE',  ( 151.2860562277021472, -2.495269033102075262, -17.79652296963211455 ) ) ;
#28486 = CARTESIAN_POINT ( 'NONE',  ( 94.20708369096698220, -25.56540164683820393, -12.65854514648976981 ) ) ;
#28487 = CARTESIAN_POINT ( 'NONE',  ( 70.19189222814998175, -51.48119552555760947, -33.79530790927901052 ) ) ;
#28488 = CARTESIAN_POINT ( 'NONE',  ( 122.0994348109119443, 0.9020085738987339008, -11.91225656197089222 ) ) ;
#28489 = EDGE_LOOP ( 'NONE', ( #12624, #28462, #17244, #4942, #24462 ) ) ;
#28490 = DIRECTION ( 'NONE',  ( 0.9908103287288504424, -0.1352586133457951423, 0.000000000000000000 ) ) ;
#28491 = CARTESIAN_POINT ( 'NONE',  ( 122.0994348109119443, -10.15424416112533912, -14.75197769757731336 ) ) ;
#28492 = CARTESIAN_POINT ( 'NONE',  ( 120.7157985609119635, -10.36940331770106916, -15.09355782777062061 ) ) ;
#28493 = CARTESIAN_POINT ( 'NONE',  ( 61.96957081968723458, -13.30635274022726300, -19.04364310209689393 ) ) ;
#28494 = CARTESIAN_POINT ( 'NONE',  ( 120.5435347346423072, -8.435056900666539903, -17.43606523319152757 ) ) ;
#28495 = CARTESIAN_POINT ( 'NONE',  ( 114.0941296295247867, -4.863998795839590272, -8.388885654883775800 ) ) ;
#28496 = ORIENTED_EDGE ( 'NONE', *, *, #5477, .F. ) ;
#28497 = CARTESIAN_POINT ( 'NONE',  ( 114.6115148109119986, -3.383040157471821630, -19.15922257007629170 ) ) ;
#28498 = CARTESIAN_POINT ( 'NONE',  ( 125.1059481442452750, -1.833838273342660141, -17.42832698103878286 ) ) ;
#28499 = CARTESIAN_POINT ( 'NONE',  ( 123.9584548109119737, -2.421111938423274879, -5.775321541204940345 ) ) ;
#28500 = AXIS2_PLACEMENT_3D ( 'NONE', #16302, #9451, #22676 ) ;
#28501 = CARTESIAN_POINT ( 'NONE',  ( 120.9081748109119872, -4.153390946401325223, -8.397313243818185668 ) ) ;
#28502 = CARTESIAN_POINT ( 'NONE',  ( 75.95778847736481509, -3.256761025687722189, -7.993215200338315007 ) ) ;
#28503 =( NAMED_UNIT ( * ) SI_UNIT ( $, .STERADIAN. ) SOLID_ANGLE_UNIT ( ) );
#28504 = CARTESIAN_POINT ( 'NONE',  ( 121.0216281442452981, -1.561330072975668948, -17.79121239304076951 ) ) ;
#28505 = CYLINDRICAL_SURFACE ( 'NONE', #20595, 3.000000000000001776 ) ;
#28506 = DIRECTION ( 'NONE',  ( -0.8636456077245089347, 0.5040994586965589219, 0.000000000000000000 ) ) ;
#28507 = DIRECTION ( 'NONE',  ( 0.000000000000000000, -0.3818493186865936084, 0.9242245927363024194 ) ) ;
#28508 = CARTESIAN_POINT ( 'NONE',  ( 112.4559014775786494, -9.988377603198976828, -10.36322818467138340 ) ) ;
#28509 = ORIENTED_EDGE ( 'NONE', *, *, #34790, .T. ) ;
#28510 = EDGE_CURVE ( 'NONE', #6998, #30513, #40419, .T. ) ;
#28511 = CARTESIAN_POINT ( 'NONE',  ( 115.7610046295247912, -4.863998795839590272, -18.39754474579285315 ) ) ;
#28512 = AXIS2_PLACEMENT_3D ( 'NONE', #29486, #43177, #25841 ) ;
#28513 = CARTESIAN_POINT ( 'NONE',  ( 121.9859814775786333, 0.2603800115204892296, -16.42320221600525088 ) ) ;
#28514 = CARTESIAN_POINT ( 'NONE',  ( 137.4945747550012811, -9.029089147476250687, -16.19493358130536365 ) ) ;
#28515 = ORIENTED_EDGE ( 'NONE', *, *, #42306, .T. ) ;
#28516 = PRODUCT_DEFINITION_SHAPE ( 'NONE', 'NONE',  #24145 ) ;
#28517 = CARTESIAN_POINT ( 'NONE',  ( 112.1722681442453222, -0.4660016031367893996, -10.09054647747474043 ) ) ;
#28518 = CARTESIAN_POINT ( 'NONE',  ( 112.3991748109119868, -1.833838273342658809, -17.42832698103878286 ) ) ;
#28519 = CARTESIAN_POINT ( 'NONE',  ( 94.20708369096698220, -25.99489077589524300, -13.39321520033831447 ) ) ;
#28520 = CARTESIAN_POINT ( 'NONE',  ( 122.3263414775786373, -3.505236298600246325, -18.68346056562440793 ) ) ;
#28521 = ORIENTED_EDGE ( 'NONE', *, *, #16124, .F. ) ;
#28522 = CARTESIAN_POINT ( 'NONE',  ( 114.7249681442453237, 0.2603800115204892296, -16.42320221600525088 ) ) ;
#28523 = EDGE_CURVE ( 'NONE', #25112, #33401, #9531, .T. ) ;
#28524 = DIRECTION ( 'NONE',  ( -1.000000000000000000, 0.000000000000000000, 0.000000000000000000 ) ) ;
#28525 = CARTESIAN_POINT ( 'NONE',  ( 64.73784058450603140, -41.08681216603740438, -16.39321520033831447 ) ) ;
#28526 = CARTESIAN_POINT ( 'NONE',  ( 111.4241771286805260, -2.495269033102075262, -17.79652296963211455 ) ) ;
#28527 = CARTESIAN_POINT ( 'NONE',  ( 125.3895814775786448, -7.893985811506177619, -18.51759400769804742 ) ) ;
#28528 = CARTESIAN_POINT ( 'NONE',  ( 70.19189222814998175, -56.12358456014947450, -35.65224734057483857 ) ) ;
#28529 = CARTESIAN_POINT ( 'NONE',  ( 124.4252281442452812, -9.261995988541697145, -16.69588392320189030 ) ) ;
#28531 = CARTESIAN_POINT ( 'NONE',  ( 124.4819548109119722, -2.084020599724406786, -8.691656652584148546 ) ) ;
#28530 = CARTESIAN_POINT ( 'NONE',  ( 123.5743281442453139, -7.893985811506177619, -18.51759400769804742 ) ) ;
#28532 = CARTESIAN_POINT ( 'NONE',  ( 119.8870948109119752, -0.8288870151387760510, -10.36305467784173118 ) ) ;
#28533 = CARTESIAN_POINT ( 'NONE',  ( 69.16666358353634791, -25.68530218154914024, -5.871463680831265464 ) ) ;
#28534 = CARTESIAN_POINT ( 'NONE',  ( 118.9227414775786400, -10.63000616557722466, -14.87417383870573495 ) ) ;
#28535 = EDGE_LOOP ( 'NONE', ( #3108, #26849, #1701, #15931, #26024, #9879 ) ) ;
#28536 = ORIENTED_EDGE ( 'NONE', *, *, #1621, .T. ) ;
#28537 = CARTESIAN_POINT ( 'NONE',  ( 71.02242295334774269, -56.18893258328766649, -38.78319397060078444 ) ) ;
#28538 = CARTESIAN_POINT ( 'NONE',  ( 115.2748327545248657, -2.477300249445798297, -19.15521520033831138 ) ) ;
#28539 = CARTESIAN_POINT ( 'NONE',  ( 113.1912390045248031, -9.868328341294098749, -11.32035403202665869 ) ) ;
#28540 = AXIS2_PLACEMENT_3D ( 'NONE', #42621, #11384, #32114 ) ;
#28541 = CARTESIAN_POINT ( 'NONE',  ( 113.6774108795247997, -1.325403438956436419, -16.93181055722141792 ) ) ;
#28542 = ADVANCED_FACE ( 'NONE', ( #44602 ), #30904, .T. ) ;
#28543 = CARTESIAN_POINT ( 'NONE',  ( 125.6164881442453094, 0.2603800115204892296, -16.42320221600525088 ) ) ;
#28544 = CARTESIAN_POINT ( 'NONE',  ( 125.8433948109119456, -7.643976991954077427, -18.09477374809248928 ) ) ;
#28545 = ORIENTED_EDGE ( 'NONE', *, *, #7813, .T. ) ;
#28546 = CARTESIAN_POINT ( 'NONE',  ( 111.4348214775786801, -3.505236298600246325, -18.68346056562440793 ) ) ;
#28547 = CARTESIAN_POINT ( 'NONE',  ( 109.3713171295247832, -10.62599879583958540, -13.39321520033831447 ) ) ;
#28548 = DIRECTION ( 'NONE',  ( 1.000000000000000000, 0.000000000000000000, -0.000000000000000000 ) ) ;
#28549 = CARTESIAN_POINT ( 'NONE',  ( 125.5030348109119558, -3.383040157471821630, -19.15922257007629170 ) ) ;
#28550 = CARTESIAN_POINT ( 'NONE',  ( 125.5597614775786326, -1.561330072975669392, -17.79121239304076951 ) ) ;
#28551 = CARTESIAN_POINT ( 'NONE',  ( 79.26207964172509435, 4.977544347528738200, -6.087841491724327980 ) ) ;
#28552 = CARTESIAN_POINT ( 'NONE',  ( 114.7249681442453237, 0.2603800115204892296, -16.42320221600525088 ) ) ;
#28553 = CARTESIAN_POINT ( 'NONE',  ( 115.4137390045248566, 0.8980012041604421569, -15.77991374673208469 ) ) ;
#28554 = CARTESIAN_POINT ( 'NONE',  ( 112.9828796295247884, -4.863998795839590272, -8.388885654883775800 ) ) ;
#28555 = ORIENTED_EDGE ( 'NONE', *, *, #19062, .T. ) ;
#28556 = DIRECTION ( 'NONE',  ( 1.000000000000000000, 0.000000000000000000, -0.000000000000000000 ) ) ;
#28557 = CARTESIAN_POINT ( 'NONE',  ( 116.6536748109119941, -10.15424416112533912, -14.75197769757731336 ) ) ;
#28558 = CARTESIAN_POINT ( 'NONE',  ( 113.1933481442453058, -4.089484607189486809, -7.948022111789456723 ) ) ;
#28559 = CARTESIAN_POINT ( 'NONE',  ( 61.69189222814998175, -60.26310523276723785, -29.64311716074571379 ) ) ;
#28560 = CARTESIAN_POINT ( 'NONE',  ( 123.5743281442453139, -2.084020599724406786, -8.691656652584148546 ) ) ;
#28561 = CARTESIAN_POINT ( 'NONE',  ( 120.8514481442452961, -2.084020599724406786, -8.691656652584148546 ) ) ;
#28562 = CARTESIAN_POINT ( 'NONE',  ( 115.6893214775786447, -9.859900752359374465, -12.68260735090039404 ) ) ;
#28563 = ORIENTED_EDGE ( 'NONE', *, *, #7465, .T. ) ;
#28564 = CARTESIAN_POINT ( 'NONE',  ( 122.0354079359119908, -4.360204210389833968, -8.000047426360245240 ) ) ;
#28565 = DIRECTION ( 'NONE',  ( -0.8636456077245080465, 0.5040994586965603652, 0.000000000000000000 ) ) ;
#28566 = CARTESIAN_POINT ( 'NONE',  ( 116.0296814775786345, -1.833838273342658809, -17.42832698103878286 ) ) ;
#28567 = ORIENTED_EDGE ( 'NONE', *, *, #24189, .F. ) ;
#28568 = DIRECTION ( 'NONE',  ( 0.000000000000000000, 0.000000000000000000, -1.000000000000000000 ) ) ;
#28569 = CARTESIAN_POINT ( 'NONE',  ( 112.1155414775786454, 0.9020085738987339008, -11.91225656197089222 ) ) ;
#28570 = CARTESIAN_POINT ( 'NONE',  ( 110.1353015045248469, -6.936859964151250502, -18.39754474579286025 ) ) ;
#28571 = LINE ( 'NONE', #11242, #9886 ) ;
#28572 = ORIENTED_EDGE ( 'NONE', *, *, #34004, .T. ) ;
#28573 = VECTOR ( 'NONE', #42145, 1000.000000000000000 ) ;
#28574 = ORIENTED_EDGE ( 'NONE', *, *, #33669, .T. ) ;
#28575 = CARTESIAN_POINT ( 'NONE',  ( 116.9373081442452929, -1.833838273342659253, -17.42832698103878286 ) ) ;
#28576 = EDGE_CURVE ( 'NONE', #15833, #24095, #41184, .T. ) ;
#28577 = CARTESIAN_POINT ( 'NONE',  ( 118.5256548109119876, -8.899110576539710493, -16.42337572283490132 ) ) ;
#28578 = CARTESIAN_POINT ( 'NONE',  ( 124.5847809835702691, -9.789958397730165629, -14.26986282893143532 ) ) ;
#28579 = CARTESIAN_POINT ( 'NONE',  ( 122.3826735609119680, 0.6414057260225851653, -11.69287257290600657 ) ) ;
#28580 = ORIENTED_EDGE ( 'NONE', *, *, #3550, .T. ) ;
#28581 = DIRECTION ( 'NONE',  ( 0.000000000000000000, 0.000000000000000000, 1.000000000000000000 ) ) ;
#28582 = CARTESIAN_POINT ( 'NONE',  ( 125.2183010572584010, -0.7431075297091613852, -7.348064569251269162 ) ) ;
#28583 = CARTESIAN_POINT ( 'NONE',  ( 111.1770983795247787, -0.7896495226426338832, -9.318865927141430916 ) ) ;
#28584 = CARTESIAN_POINT ( 'NONE',  ( 111.7751814775786556, -7.893985811506177619, -18.51759400769804742 ) ) ;
#28585 = CARTESIAN_POINT ( 'NONE',  ( 111.9453614775786434, -1.561330072975668060, -17.79121239304076596 ) ) ;
#28586 = CARTESIAN_POINT ( 'NONE',  ( 116.2565881442453133, -0.8288870151387760510, -10.36305467784173118 ) ) ;
#28587 = DIRECTION ( 'NONE',  ( 1.000000000000000000, 0.000000000000000000, 0.000000000000000000 ) ) ;
#28588 = VERTEX_POINT ( 'NONE', #24298 ) ;
#28589 = CARTESIAN_POINT ( 'NONE',  ( 114.6682414775786469, -7.894159318335828068, -9.358103419637847864 ) ) ;
#28590 = CARTESIAN_POINT ( 'NONE',  ( 115.5526452545247622, 0.8980012041604421569, -11.00651665394454071 ) ) ;
#28591 = FACE_OUTER_BOUND ( 'NONE', #707, .T. ) ;
#28592 = CARTESIAN_POINT ( 'NONE',  ( 73.07463722459043254, -58.49647601156275556, -35.70688775835006368 ) ) ;
#28593 = CARTESIAN_POINT ( 'NONE',  ( 115.6325948109119821, 0.2603800115204892296, -16.42320221600525088 ) ) ;
#28594 = EDGE_LOOP ( 'NONE', ( #34590, #26541, #23800, #25195, #39496 ) ) ;
#28595 = CARTESIAN_POINT ( 'NONE',  ( 116.6536748109119941, 0.9020085738987339008, -11.91225656197089222 ) ) ;
#28596 = CARTESIAN_POINT ( 'NONE',  ( 114.3846081442453197, -10.63000616557721756, -14.87417383870574206 ) ) ;
#28597 = CARTESIAN_POINT ( 'NONE',  ( 110.4825671295247815, -10.62599879583958540, -13.39321520033831447 ) ) ;
#28598 = CARTESIAN_POINT ( 'NONE',  ( 116.2565881442452991, -9.261995988541697145, -16.69588392320189030 ) ) ;
#28599 = CARTESIAN_POINT ( 'NONE',  ( 112.6260814775786514, -9.261995988541697145, -16.69588392320189030 ) ) ;
#28600 = PRODUCT_DEFINITION_FORMATION_WITH_SPECIFIED_SOURCE ( 'ANY', '', #28885, .NOT_KNOWN. ) ;
#28601 = CARTESIAN_POINT ( 'NONE',  ( 127.9806007748621255, -10.70395921878446011, -14.08905720169468978 ) ) ;
#28602 = CARTESIAN_POINT ( 'NONE',  ( 77.44400397045842510, -3.459648945705700473, -16.39321520033831447 ) ) ;
#28603 = CARTESIAN_POINT ( 'NONE',  ( 67.08264006073221708, -20.21382323020432992, -15.89321520033831447 ) ) ;
#28604 = ORIENTED_EDGE ( 'NONE', *, *, #6417, .T. ) ;
#28605 = VECTOR ( 'NONE', #14338, 1000.000000000000000 ) ;
#28606 = DIRECTION ( 'NONE',  ( 0.000000000000000000, -0.3818493186865927203, 0.9242245927363029745 ) ) ;
#28607 = CARTESIAN_POINT ( 'NONE',  ( 109.2294398423855739, -8.045347437686777070, -17.68788261941902107 ) ) ;
#28608 = CARTESIAN_POINT ( 'NONE',  ( 115.4056881442453459, -2.084020599724406786, -8.691656652584148546 ) ) ;
#28609 = LINE ( 'NONE', #38615, #18288 ) ;
#28610 = CARTESIAN_POINT ( 'NONE',  ( 116.4555358795247884, -8.402594152722688392, -9.854619843455216355 ) ) ;
#28611 = CARTESIAN_POINT ( 'NONE',  ( 114.7192077545248594, -2.791137627527939813, -18.39754474579286025 ) ) ;
#28612 = CARTESIAN_POINT ( 'NONE',  ( 121.9093097909088215, -1.016270020561755860, -17.26805140881366896 ) ) ;
#28613 = CARTESIAN_POINT ( 'NONE',  ( 113.8740681442453138, -9.859900752359374465, -12.68260735090039404 ) ) ;
#28614 = DIRECTION ( 'NONE',  ( -0.000000000000000000, -0.9284778069183721172, -0.3713878862591650232 ) ) ;
#28615 = CARTESIAN_POINT ( 'NONE',  ( 122.8936081442453059, 0.2603800115204892296, -16.42320221600525088 ) ) ;
#28616 = CARTESIAN_POINT ( 'NONE',  ( 119.2063748109119814, -1.561330072975668504, -17.79121239304076951 ) ) ;
#28617 = VERTEX_POINT ( 'NONE', #23625 ) ;
#28618 = CARTESIAN_POINT ( 'NONE',  ( 116.7104014775786425, -8.899110576539710493, -16.42337572283490132 ) ) ;
#28619 = CARTESIAN_POINT ( 'NONE',  ( 112.7395348109119766, -5.638512984488999180, -18.83840828888717311 ) ) ;
#28620 = CARTESIAN_POINT ( 'NONE',  ( 117.8449348109119938, -8.166667518702817929, -8.995218007635861213 ) ) ;
#28621 = CARTESIAN_POINT ( 'NONE',  ( 120.1140014775786398, -7.894159318335828068, -9.358103419637847864 ) ) ;
#28622 = ORIENTED_EDGE ( 'NONE', *, *, #38409, .T. ) ;
#28623 = CARTESIAN_POINT ( 'NONE',  ( 120.3409081442453044, -8.899110576539710493, -16.42337572283490132 ) ) ;
#28624 = AXIS2_PLACEMENT_3D ( 'NONE', #26921, #9368, #26023 ) ;
#28625 = CARTESIAN_POINT ( 'NONE',  ( 120.6812681442452941, -10.30919188438810075, -12.61870101168855918 ) ) ;
#28626 = CARTESIAN_POINT ( 'NONE',  ( 136.4689272580744444, 0.8652765085456386451, -12.77968882490968561 ) ) ;
#28627 = CARTESIAN_POINT ( 'NONE',  ( 109.5102233795247884, -8.938348069036489818, -17.46756447353520159 ) ) ;
#28628 = CARTESIAN_POINT ( 'NONE',  ( 86.48169505875749508, -25.23119213852205789, -15.24166438581092109 ) ) ;
#28629 = CARTESIAN_POINT ( 'NONE',  ( 116.8209981608379877, 0.3867979994853637526, -14.64321520033831447 ) ) ;
#28630 = EDGE_CURVE ( 'NONE', #37481, #12500, #6744, .T. ) ;
#28631 = CARTESIAN_POINT ( 'NONE',  ( 112.8439733795247832, -1.325403438956436419, -9.854619843455211026 ) ) ;
#28632 = CIRCLE ( 'NONE', #35869, 2.999999999999999556 ) ;
#28633 = CARTESIAN_POINT ( 'NONE',  ( 115.5191414775786569, -3.383040157471821630, -19.15922257007629170 ) ) ;
#28634 = CARTESIAN_POINT ( 'NONE',  ( 137.0105207745574774, -10.31073456892766593, -13.75249372251127689 ) ) ;
#28635 = CARTESIAN_POINT ( 'NONE',  ( 115.5191414775786569, -6.222761293078241884, -8.102969835052219238 ) ) ;
#28636 = CARTESIAN_POINT ( 'NONE',  ( 70.19189222814998175, -58.18802696105826300, -36.47801710466001879 ) ) ;
#28637 = DIRECTION ( 'NONE',  ( 0.9609149988134837450, -0.1028163501681639419, 0.2570431154366518145 ) ) ;
#28638 = CARTESIAN_POINT ( 'NONE',  ( 112.1494421295248003, -9.868328341294093420, -13.39321520033831447 ) ) ;
#28639 = CARTESIAN_POINT ( 'NONE',  ( 113.0798948109119948, -8.899110576539710493, -16.42337572283490132 ) ) ;
#28640 = CYLINDRICAL_SURFACE ( 'NONE', #34738, 0.4999999999999996669 ) ;
#28641 = EDGE_CURVE ( 'NONE', #24842, #38956, #22606, .T. ) ;
#28642 = DIRECTION ( 'NONE',  ( -0.000000000000000000, -0.9284778069183721172, -0.3713878862591650232 ) ) ;
#28644 = CARTESIAN_POINT ( 'NONE',  ( 120.1140014775786398, -1.561330072975668504, -17.79121239304076951 ) ) ;
#28643 = CARTESIAN_POINT ( 'NONE',  ( 62.52450766521648262, -14.54539169785276442, -9.275848827766759896 ) ) ;
#28645 = CARTESIAN_POINT ( 'NONE',  ( 119.4900081442453086, -7.643976991954077427, -18.09477374809248928 ) ) ;
#28646 = CARTESIAN_POINT ( 'NONE',  ( 125.7299414775786346, 0.9020085738987339008, -11.91225656197089222 ) ) ;
#28647 = ORIENTED_EDGE ( 'NONE', *, *, #20953, .F. ) ;
#28648 = CARTESIAN_POINT ( 'NONE',  ( 136.3568202015625275, -7.080281580350018089, -8.023828915629925618 ) ) ;
#28649 = CARTESIAN_POINT ( 'NONE',  ( 124.3117748109119844, -10.30919188438810075, -12.61870101168855918 ) ) ;
#28650 = CARTESIAN_POINT ( 'NONE',  ( 116.3166296295247832, -4.863998795839590272, -8.388885654883775800 ) ) ;
#28651 = CARTESIAN_POINT ( 'NONE',  ( 117.6747548109119919, -7.643976991954077427, -18.09477374809248928 ) ) ;
#28653 = CARTESIAN_POINT ( 'NONE',  ( 117.9583881442453048, 0.1319031606808879209, -14.10382304977623669 ) ) ;
#28652 = COLOUR_RGB ( '',0.7921568627450980005, 0.8196078431372548767, 0.9333333333333333481 ) ;
#28654 = CARTESIAN_POINT ( 'NONE',  ( 85.94313020268559455, -27.37200725933698564, -8.637542561674017350 ) ) ;
#28655 = CARTESIAN_POINT ( 'NONE',  ( 113.1217858795247935, -0.7896495226426338832, -17.46756447353520159 ) ) ;
#28656 = CARTESIAN_POINT ( 'NONE',  ( 119.9438214775786378, -2.084020599724406786, -8.691656652584148546 ) ) ;
#28657 = VECTOR ( 'NONE', #165, 1000.000000000000227 ) ;
#28658 = CARTESIAN_POINT ( 'NONE',  ( 124.1983214775786166, -1.833838273342659697, -17.42832698103878286 ) ) ;
#28659 = CARTESIAN_POINT ( 'NONE',  ( 115.7573452706806876, 0.3193521225029610777, -14.64321520033831447 ) ) ;
#28660 = CARTESIAN_POINT ( 'NONE',  ( 109.2294408980514930, -1.069172662007336960, -9.568136978171825291 ) ) ;
#28661 = CARTESIAN_POINT ( 'NONE',  ( 119.9518141859119851, -8.321307733199551748, -9.223433127585318303 ) ) ;
#28662 = CARTESIAN_POINT ( 'NONE',  ( 115.1359265045248605, -7.250697342233347165, -19.15521520033831138 ) ) ;
#28663 = EDGE_CURVE ( 'NONE', #12393, #3515, #21728, .T. ) ;
#28664 = CARTESIAN_POINT ( 'NONE',  ( 117.2294421295247986, 1.129870453897466431, -21.68537999533008076 ) ) ;
#28665 = CARTESIAN_POINT ( 'NONE',  ( 118.9227414775786400, -10.63000616557722466, -14.87417383870573495 ) ) ;
#28666 = CARTESIAN_POINT ( 'NONE',  ( 119.3765548109119834, 0.9020085738987339008, -11.91225656197089222 ) ) ;
#28667 = CARTESIAN_POINT ( 'NONE',  ( 109.8574890045247940, 0.8980012041604421569, -15.77991374673208469 ) ) ;
#28668 = CARTESIAN_POINT ( 'NONE',  ( 112.3991748109119868, -8.166667518702817929, -8.995218007635859436 ) ) ;
#28669 = ADVANCED_FACE ( 'NONE', ( #2399 ), #27010, .T. ) ;
#28670 = EDGE_CURVE ( 'NONE', #26479, #31784, #16068, .T. ) ;
#28671 = ORIENTED_EDGE ( 'NONE', *, *, #15081, .T. ) ;
#28672 = DIRECTION ( 'NONE',  ( 1.000000000000000000, 0.000000000000000000, 0.000000000000000000 ) ) ;
#28673 = AXIS2_PLACEMENT_3D ( 'NONE', #32747, #19537, #26605 ) ;
#28674 = CARTESIAN_POINT ( 'NONE',  ( 116.8805814775786445, -6.344957434206662583, -7.627207830600332805 ) ) ;
#28675 = CARTESIAN_POINT ( 'NONE',  ( 122.2696148109119889, -5.574606645277164318, -18.38911715685844683 ) ) ;
#28676 = CARTESIAN_POINT ( 'NONE',  ( 0.000000000000000000, 0.000000000000000000, 0.000000000000000000 ) ) ;
#28677 = CARTESIAN_POINT ( 'NONE',  ( 126.0135748109119902, -8.166667518702819706, -8.995218007635861213 ) ) ;
#28678 = CARTESIAN_POINT ( 'NONE',  ( 121.3619881442452879, -4.089484607189486809, -7.948022111789456723 ) ) ;
#28679 = CARTESIAN_POINT ( 'NONE',  ( 114.5108483795247878, -0.7896495226426338832, -9.318865927141430916 ) ) ;
#28680 = B_SPLINE_CURVE_WITH_KNOTS ( 'NONE', 3,
 ( #40029, #1493, #39808, #12227, #8574, #39587, #40492, #25680, #15415, #8793 ),
 .UNSPECIFIED., .F., .F.,
 ( 4, 3, 3, 4 ),
 ( 0.000000000000000000, 0.0001671877560958085049, 0.0003343755126086549959, 0.0006438490228505480001 ),
 .UNSPECIFIED. ) ;
#28681 = CARTESIAN_POINT ( 'NONE',  ( 116.4267681442453153, -6.222761293078241884, -8.102969835052219238 ) ) ;
#28682 = CARTESIAN_POINT ( 'NONE',  ( 123.2161110609119561, -3.163656168406935087, -18.89861972220014508 ) ) ;
#28683 = CARTESIAN_POINT ( 'NONE',  ( 61.76986277844709861, -39.32091226840162079, -19.39321520033831447 ) ) ;
#28684 = ORIENTED_EDGE ( 'NONE', *, *, #11741, .T. ) ;
#28685 = CLOSED_SHELL ( 'NONE', ( #9157, #29468, #30926, #40077, #5849, #30615, #5283, #44746, #44936, #17153, #18869, #38709, #12811, #44004, #14687, #37594, #11085, #44520, #33422, #37985, #13870, #8589, #42033, #27786, #20118, #28373, #44569, #7918, #26046, #32050, #1057, #19871, #740, #35961, #27589, #45130, #34117, #21958, #17099, #18360, #27977, #6108, #28192, #36121, #27286, #25171, #1906, #39580, #26874, #43120, #20833, #22691, #28918, #16676, #5583, #26155, #30711, #7350, #38479, #27702, #21390, #42839, #14742, #17277, #29763, #31176, #15584, #33416, #3587, #21776, #38738, #4961, #34374, #44952, #14327, #36513, #5507, #29782, #1424, #28972, #2417, #31209, #37396, #38405, #24463, #32607, #23660, #236, #22884, #11913, #42610, #17353, #42023, #18483, #14393, #21992, #12483, #14713, #13694, #16155, #8312, #12870, #26548, #40343, #25603, #15333, #30423, #24480, #32268, #2242, #42582, #37930, #2813, #33464, #33108, #3824, #43747, #30860, #16160, #29733, #42904, #40401, #6374, #19929, #12882, #11531, #31728, #25629, #5031, #42361, #42284, #27081, #19247, #25032, #20464 ) ) ;
#28686 = CARTESIAN_POINT ( 'NONE',  ( 119.6045485609119794, -0.08252387247370887580, -11.91645802438286417 ) ) ;
#28687 = CARTESIAN_POINT ( 'NONE',  ( 119.3765548109119834, 0.9020085738987339008, -11.91225656197089222 ) ) ;
#28688 = ORIENTED_EDGE ( 'NONE', *, *, #38650, .F. ) ;
#28689 = CARTESIAN_POINT ( 'NONE',  ( 122.5182407289968154, -6.032552146994431652, -18.32589373581284775 ) ) ;
#28690 = DIRECTION ( 'NONE',  ( 0.9609149988134837450, -0.1028163501681639419, 0.2570431154366518145 ) ) ;
#28691 = CARTESIAN_POINT ( 'NONE',  ( 122.3263414775786373, -6.344957434206689229, -7.627207830600343463 ) ) ;
#28692 = CARTESIAN_POINT ( 'NONE',  ( 115.4624148109119943, -4.153390946401321671, -8.397313243818183892 ) ) ;
#28693 = DIRECTION ( 'NONE',  ( 0.8636456077245090457, -0.5040994586965586999, 0.000000000000000000 ) ) ;
#28694 = CARTESIAN_POINT ( 'NONE',  ( 124.5074358514838906, -9.686381406722462728, -12.07228238157437694 ) ) ;
#28695 = CARTESIAN_POINT ( 'NONE',  ( 118.6958348109119754, -3.505236298600246325, -18.68346056562440793 ) ) ;
#28696 = CARTESIAN_POINT ( 'NONE',  ( 121.8158014775786171, -5.638512984488987634, -18.83840828888717311 ) ) ;
#28697 = CARTESIAN_POINT ( 'NONE',  ( 120.0005481442453146, -4.153390946401325223, -8.397313243818185668 ) ) ;
#28698 = EDGE_CURVE ( 'NONE', #1665, #44682, #19969, .T. ) ;
#28699 = DIRECTION ( 'NONE',  ( 0.000000000000000000, 0.000000000000000000, -1.000000000000000000 ) ) ;
#28700 = CARTESIAN_POINT ( 'NONE',  ( 119.3198281442452924, -9.859900752359374465, -12.68260735090039404 ) ) ;
#28701 = CARTESIAN_POINT ( 'NONE',  ( 113.2500748109119968, -6.344957434206662583, -7.627207830600332805 ) ) ;
#28702 = CARTESIAN_POINT ( 'NONE',  ( 120.3976348109119812, -1.834011780172310813, -8.268836392978581529 ) ) ;
#28703 = CARTESIAN_POINT ( 'NONE',  ( 111.7751814775786556, -7.893985811506177619, -18.51759400769804742 ) ) ;
#28704 = DIRECTION ( 'NONE',  ( -0.000000000000000000, -0.9284778069183718952, -0.3713878862591649677 ) ) ;
#28705 = CARTESIAN_POINT ( 'NONE',  ( 119.7736414775786358, 0.1319031606808879209, -14.10382304977623669 ) ) ;
#28706 = ORIENTED_EDGE ( 'NONE', *, *, #11278, .F. ) ;
#28707 = CARTESIAN_POINT ( 'NONE',  ( 119.7169148109119874, -9.988377603198976828, -10.36322818467138340 ) ) ;
#28708 = CARTESIAN_POINT ( 'NONE',  ( 114.0941296295247867, -4.863998795839590272, -8.388885654883775800 ) ) ;
#28709 = CARTESIAN_POINT ( 'NONE',  ( 78.69189222814998175, -46.76310523276723785, -6.893215200338315363 ) ) ;
#28710 = FACE_OUTER_BOUND ( 'NONE', #44738, .T. ) ;
#28711 = CARTESIAN_POINT ( 'NONE',  ( 70.19189222814998175, -54.47411573338475677, -34.99246555962335492 ) ) ;
#28712 = CARTESIAN_POINT ( 'NONE',  ( 91.77400275106518279, -25.23119213852205789, -15.24166438581092109 ) ) ;
#28713 = ORIENTED_EDGE ( 'NONE', *, *, #16105, .T. ) ;
#28714 = CARTESIAN_POINT ( 'NONE',  ( 67.84197459855160162, -62.01099631431865333, -38.73636453584316541 ) ) ;
#28715 = CARTESIAN_POINT ( 'NONE',  ( 123.4041481442452834, 0.1319031606808879209, -14.10382304977623669 ) ) ;
#28716 = DIRECTION ( 'NONE',  ( 0.000000000000000000, -0.9242245927363027524, -0.3818493186865928868 ) ) ;
#28717 = CARTESIAN_POINT ( 'NONE',  ( 66.40642813730079297, -14.77805237463982024, -16.29520547388278118 ) ) ;
#28718 = EDGE_CURVE ( 'NONE', #408, #21278, #40957, .T. ) ;
#28719 = CARTESIAN_POINT ( 'NONE',  ( 111.5138235035216780, -0.1451374939625849625, -15.72356508888860738 ) ) ;
#28720 = CARTESIAN_POINT ( 'NONE',  ( 113.5385046295247804, -4.863998795839590272, -18.39754474579285315 ) ) ;
#28721 = EDGE_LOOP ( 'NONE', ( #13971, #15852, #656, #8641, #598, #35817, #43148, #16074, #23540 ) ) ;
#28722 = CARTESIAN_POINT ( 'NONE',  ( 115.1787814775786387, -9.988377603198976828, -10.36322818467138340 ) ) ;
#28723 = CARTESIAN_POINT ( 'NONE',  ( 114.3278814775786429, -10.30919188438810075, -12.61870101168855918 ) ) ;
#28724 = CARTESIAN_POINT ( 'NONE',  ( 69.69189222814998175, -41.76310523276723785, -7.393215200338315363 ) ) ;
#28725 = CARTESIAN_POINT ( 'NONE',  ( 119.6034614775786196, -3.505236298600246325, -18.68346056562440793 ) ) ;
#28726 = CARTESIAN_POINT ( 'NONE',  ( 126.3999550322235308, -3.647810012370235722, -8.449820221509870777 ) ) ;
#28727 = CARTESIAN_POINT ( 'NONE',  ( 122.3830681442452857, -8.166667518702819706, -8.995218007635861213 ) ) ;
#28728 = CARTESIAN_POINT ( 'NONE',  ( 123.9714148109119805, -8.899110576539726480, -16.42337572283488001 ) ) ;
#28729 = EDGE_CURVE ( 'NONE', #2441, #28337, #43021, .T. ) ;
#28730 = FACE_OUTER_BOUND ( 'NONE', #556, .T. ) ;
#28731 = DIRECTION ( 'NONE',  ( 0.5735764363510499342, 0.3127926500124801890, -0.7570804645221008711 ) ) ;
#28732 = CARTESIAN_POINT ( 'NONE',  ( 112.6260814775786514, -9.261995988541697145, -16.69588392320189030 ) ) ;
#28733 = ORIENTED_EDGE ( 'NONE', *, *, #38422, .T. ) ;
#28734 = CARTESIAN_POINT ( 'NONE',  ( 116.1082702545247827, 0.1403307496149616695, -11.32035403202665336 ) ) ;
#28735 = CARTESIAN_POINT ( 'NONE',  ( 121.4187148109119789, -6.344957434206665248, -7.627207830600338134 ) ) ;
#28736 = CARTESIAN_POINT ( 'NONE',  ( 62.78977304965946615, -1.552730279056773410, -19.34404429361859457 ) ) ;
#28737 = ORIENTED_EDGE ( 'NONE', *, *, #10023, .T. ) ;
#28738 = FACE_OUTER_BOUND ( 'NONE', #28594, .T. ) ;
#28739 = CARTESIAN_POINT ( 'NONE',  ( 126.2404814775786264, -9.261995988541697145, -16.69588392320189030 ) ) ;
#28740 = CARTESIAN_POINT ( 'NONE',  ( 60.06931813437629586, -14.72076136720887085, -8.603412892520118760 ) ) ;
#28741 = CARTESIAN_POINT ( 'NONE',  ( 122.1561614775786353, -8.899110576539710493, -16.42337572283490132 ) ) ;
#28742 = VECTOR ( 'NONE', #10867, 1000.000000000000114 ) ;
#28743 = ORIENTED_EDGE ( 'NONE', *, *, #40151, .T. ) ;
#28744 = CARTESIAN_POINT ( 'NONE',  ( 119.0929214775786278, -5.638512984488999180, -18.83840828888717311 ) ) ;
#28745 = CARTESIAN_POINT ( 'NONE',  ( 110.4384831777918805, -0.01829820670803256055, -14.64321520033831447 ) ) ;
#28746 = DIRECTION ( 'NONE',  ( 0.000000000000000000, 0.000000000000000000, 1.000000000000000000 ) ) ;
#28747 = CARTESIAN_POINT ( 'NONE',  ( 137.1799701741848025, -5.066786549864910505, -8.072398738317787092 ) ) ;
#28748 = CARTESIAN_POINT ( 'NONE',  ( 124.0281414775786146, -1.834011780172310813, -8.268836392978581529 ) ) ;
#28749 = DIRECTION ( 'NONE',  ( 0.000000000000000000, 0.000000000000000000, -1.000000000000000000 ) ) ;
#28750 = CARTESIAN_POINT ( 'NONE',  ( 90.48265143217095385, -25.66130191030491758, -14.20063063452593255 ) ) ;
#28751 = CARTESIAN_POINT ( 'NONE',  ( 123.5176014775786228, -9.261995988541697145, -16.69588392320189030 ) ) ;
#28753 = CARTESIAN_POINT ( 'NONE',  ( 123.1772414775786189, -5.574606645277164318, -18.38911715685844683 ) ) ;
#28752 = CARTESIAN_POINT ( 'NONE',  ( 124.2550481442452792, -9.988377603198980381, -10.36322818467138518 ) ) ;
#28754 = CARTESIAN_POINT ( 'NONE',  ( 120.7157985609119635, -0.08252387247370887580, -11.91645802438286417 ) ) ;
#28755 = CARTESIAN_POINT ( 'NONE',  ( 123.1772414775786189, -5.574606645277164318, -18.38911715685844683 ) ) ;
#28756 = CARTESIAN_POINT ( 'NONE',  ( 92.04708369096698561, -25.99489077589524300, -13.39321520033831625 ) ) ;
#28757 = CARTESIAN_POINT ( 'NONE',  ( 120.2841814775786276, 0.9020085738987339008, -11.91225656197089222 ) ) ;
#28758 = ORIENTED_EDGE ( 'NONE', *, *, #13075, .F. ) ;
#28759 = EDGE_CURVE ( 'NONE', #10189, #38611, #44151, .T. ) ;
#28760 = DIRECTION ( 'NONE',  ( 0.000000000000000000, -0.3818493186865927203, 0.9242245927363029745 ) ) ;
#28761 = CARTESIAN_POINT ( 'NONE',  ( 115.4831921295247952, 0.8980012041604618078, -13.39321520033831447 ) ) ;
#28762 = CARTESIAN_POINT ( 'NONE',  ( 113.6079577545248043, -2.791137627527939813, -18.39754474579286025 ) ) ;
#28763 = CARTESIAN_POINT ( 'NONE',  ( 115.7610046295247912, -4.863998795839590272, -18.39754474579285315 ) ) ;
#28764 = CARTESIAN_POINT ( 'NONE',  ( 125.3328548109119964, -0.8288870151393684660, -10.36305467784094247 ) ) ;
#28765 = CARTESIAN_POINT ( 'NONE',  ( 116.9373081442452929, -8.166667518702817929, -8.995218007635861213 ) ) ;
#28766 = ORIENTED_EDGE ( 'NONE', *, *, #10913, .T. ) ;
#28767 = CARTESIAN_POINT ( 'NONE',  ( 112.0020881442453344, -9.565557343593413364, -10.61323700422348004 ) ) ;
#28768 = CARTESIAN_POINT ( 'NONE',  ( 105.5513952545248060, 0.8980012041604421569, -11.00651665394454071 ) ) ;
#28769 = CARTESIAN_POINT ( 'NONE',  ( 122.0994348109119585, -10.15424416112534978, -14.75197769757730093 ) ) ;
#28770 = CARTESIAN_POINT ( 'NONE',  ( 94.20708369096698220, -26.09538666226425363, -14.49867541642786861 ) ) ;
#28771 = DIRECTION ( 'NONE',  ( -1.000000000000000000, 0.000000000000000000, -0.000000000000000000 ) ) ;
#28772 = CARTESIAN_POINT ( 'NONE',  ( 60.37068618338318515, -13.41750073646542596, -19.35316885160253264 ) ) ;
#28773 = CARTESIAN_POINT ( 'NONE',  ( 116.1998614775786507, -10.63000616557722466, -14.87417383870573495 ) ) ;
#28774 = CARTESIAN_POINT ( 'NONE',  ( 115.8999108795247821, -8.938348069036489818, -9.318865927141430916 ) ) ;
#28775 = CARTESIAN_POINT ( 'NONE',  ( 110.7603796295247918, -4.863998795839590272, -8.388885654883775800 ) ) ;
#28776 = CONICAL_SURFACE ( 'NONE', #2555, 2.999999999999999556, 0.9599310885968830309 ) ;
#28777 = EDGE_LOOP ( 'NONE', ( #42942, #17410, #29674, #31720 ) ) ;
#28778 = CARTESIAN_POINT ( 'NONE',  ( 126.2940345447956503, -7.620160344469310232, -9.176220693874684642 ) ) ;
#28779 = CARTESIAN_POINT ( 'NONE',  ( 117.4478481442453131, -9.565557343593413364, -10.61323700422348004 ) ) ;
#28780 = CARTESIAN_POINT ( 'NONE',  ( 114.5547881442453217, -5.638512984488999180, -18.83840828888717311 ) ) ;
#28781 = EDGE_CURVE ( 'NONE', #40512, #32536, #29358, .T. ) ;
#28782 = DIRECTION ( 'NONE',  ( -0.000000000000000000, -0.9284778069183721172, -0.3713878862591650232 ) ) ;
#28783 = CARTESIAN_POINT ( 'NONE',  ( 124.9924948109119924, -5.574606645277164318, -18.38911715685844683 ) ) ;
#28784 = UNCERTAINTY_MEASURE_WITH_UNIT (LENGTH_MEASURE( 1.000000000000000082E-05 ), #24795, 'distance_accuracy_value', 'NONE');
#28785 = CARTESIAN_POINT ( 'NONE',  ( 120.3976348109119812, -7.643976991954077427, -18.09477374809248928 ) ) ;
#28786 = CARTESIAN_POINT ( 'NONE',  ( 117.5045748109119756, -9.859900752359374465, -12.68260735090039404 ) ) ;
#28787 = ORIENTED_EDGE ( 'NONE', *, *, #26685, .F. ) ;
#28788 = VECTOR ( 'NONE', #10788, 1000.000000000000000 ) ;
#28789 = CARTESIAN_POINT ( 'NONE',  ( 124.3968141859119783, -8.321307733199551748, -9.223433127585318303 ) ) ;
#28790 = DIRECTION ( 'NONE',  ( 0.000000000000000000, -0.3818493186865927203, 0.9242245927363029745 ) ) ;
#28791 = CARTESIAN_POINT ( 'NONE',  ( 118.4122014775786340, -9.859900752359374465, -12.68260735090039404 ) ) ;
#28792 = VERTEX_POINT ( 'NONE', #17669 ) ;
#28793 = CARTESIAN_POINT ( 'NONE',  ( 110.9878884760652795, 0.6362173239733635022, -12.14321520033831625 ) ) ;
#28794 = CARTESIAN_POINT ( 'NONE',  ( 114.3278814775786429, -10.30919188438810075, -12.61870101168855918 ) ) ;
#28795 = CARTESIAN_POINT ( 'NONE',  ( 116.3166296295247832, -4.863998795839590272, -19.15521520033831493 ) ) ;
#28796 = CARTESIAN_POINT ( 'NONE',  ( 125.7866681442452688, -8.899110576539710493, -16.42337572283490132 ) ) ;
#28797 = ORIENTED_EDGE ( 'NONE', *, *, #34504, .F. ) ;
#28798 = ORIENTED_EDGE ( 'NONE', *, *, #25617, .F. ) ;
#28799 = CARTESIAN_POINT ( 'NONE',  ( 124.0281414775786146, -7.643976991954077427, -18.09477374809248928 ) ) ;
#28800 = CARTESIAN_POINT ( 'NONE',  ( 117.9016614775786280, -0.1624402480850797581, -16.17319339645315424 ) ) ;
#28801 = CARTESIAN_POINT ( 'NONE',  ( 124.5644539102826513, -9.858463830682730134, -13.67056496101630181 ) ) ;
#28802 = CARTESIAN_POINT ( 'NONE',  ( 92.04708369096698561, -25.38011337280982715, -14.88121679464376257 ) ) ;
#28803 = EDGE_LOOP ( 'NONE', ( #26643, #40866, #18292, #27054, #14773 ) ) ;
#28804 = CARTESIAN_POINT ( 'NONE',  ( 151.2860562277021472, -4.863998795839242995, -13.39321520033831447 ) ) ;
#28805 = CARTESIAN_POINT ( 'NONE',  ( 124.9009360172553897, -2.375710885519020099, -6.139922134414775634 ) ) ;
#28806 = VECTOR ( 'NONE', #31260, 1000.000000000000114 ) ;
#28807 = CARTESIAN_POINT ( 'NONE',  ( 111.5938171295247940, -10.62599879583958540, -13.39321520033831447 ) ) ;
#28808 = CARTESIAN_POINT ( 'NONE',  ( 117.2294421295247844, -10.76310523276723785, -21.89255013987451548 ) ) ;
#28809 = CARTESIAN_POINT ( 'NONE',  ( 125.6732148109119862, -9.859900752359378018, -12.68260735090039759 ) ) ;
#28810 = CARTESIAN_POINT ( 'NONE',  ( 122.8368814775786291, -7.894159318335828068, -9.358103419637847864 ) ) ;
#28811 = FACE_OUTER_BOUND ( 'NONE', #42402, .T. ) ;
#28812 = EDGE_LOOP ( 'NONE', ( #9823, #42592, #4116, #1525, #18552 ) ) ;
#28813 = VECTOR ( 'NONE', #21267, 1000.000000000000114 ) ;
#28814 = CARTESIAN_POINT ( 'NONE',  ( 121.1350814775786233, -9.859900752359378018, -12.68260735090039759 ) ) ;
#28815 = CARTESIAN_POINT ( 'NONE',  ( 119.7434548109119703, -2.527210466738042172, -8.967976844669124148 ) ) ;
#28816 = CARTESIAN_POINT ( 'NONE',  ( 117.0806140045248185, 0.1403307496149616695, -15.46607636864997204 ) ) ;
#28817 = CARTESIAN_POINT ( 'NONE',  ( 116.1777233795247781, -8.938348069036489818, -17.46756447353520159 ) ) ;
#28818 = CARTESIAN_POINT ( 'NONE',  ( 115.4056881442453459, -7.893985811506177619, -18.51759400769804742 ) ) ;
#28819 = EDGE_LOOP ( 'NONE', ( #42620, #7692, #37798, #28040, #26907, #44676 ) ) ;
#28820 = CARTESIAN_POINT ( 'NONE',  ( 117.1074881442453233, -10.63000616557722466, -14.87417383870573495 ) ) ;
#28821 = DIRECTION ( 'NONE',  ( -0.4461977533474357771, 0.3417300876246960328, -0.8271203734159368048 ) ) ;
#28822 = CARTESIAN_POINT ( 'NONE',  ( 112.3578015045248861, -2.477300249445798297, -7.631215200338321125 ) ) ;
#28823 = CARTESIAN_POINT ( 'NONE',  ( 116.4267681442453153, -3.383040157471821630, -19.15922257007629170 ) ) ;
#28824 = CARTESIAN_POINT ( 'NONE',  ( 118.0151148109119816, -10.63000616557722466, -14.87417383870573495 ) ) ;
#28825 = CARTESIAN_POINT ( 'NONE',  ( 125.4463081442452932, -4.153390946401325223, -8.397313243818185668 ) ) ;
#28826 = CARTESIAN_POINT ( 'NONE',  ( 60.91427317013496889, -14.50360402731953968, -18.09323085839352530 ) ) ;
#28827 = CARTESIAN_POINT ( 'NONE',  ( 69.36136150295220659, -56.47321011115533196, -32.68728869368257506 ) ) ;
#28828 = ORIENTED_EDGE ( 'NONE', *, *, #32901, .T. ) ;
#28829 = CARTESIAN_POINT ( 'NONE',  ( 115.8304577545247582, -7.250697342233347165, -7.631215200338321125 ) ) ;
#28830 = CARTESIAN_POINT ( 'NONE',  ( 109.2294432855482000, -5.177919973337370863, -18.58740422179702989 ) ) ;
#28831 = CARTESIAN_POINT ( 'NONE',  ( 120.6812681442452941, 0.1319031606808879209, -14.10382304977623669 ) ) ;
#28832 = EDGE_CURVE ( 'NONE', #35171, #5517, #29905, .T. ) ;
#28833 = DIRECTION ( 'NONE',  ( -1.000000000000000000, 0.000000000000000000, -0.000000000000000000 ) ) ;
#28834 = CARTESIAN_POINT ( 'NONE',  ( 114.8581140045248361, 0.1403307496149616695, -15.46607636864997204 ) ) ;
#28835 = CARTESIAN_POINT ( 'NONE',  ( 114.8581140045248361, 0.1403307496149616695, -15.46607636864997204 ) ) ;
#28836 = CYLINDRICAL_SURFACE ( 'NONE', #1433, 1.999999999999998890 ) ;
#28837 = CARTESIAN_POINT ( 'NONE',  ( 113.9875214775786532, -8.899110576539710493, -16.42337572283490132 ) ) ;
#28838 = CARTESIAN_POINT ( 'NONE',  ( 110.2184548109119788, -4.863998795839242995, -13.39321520033831447 ) ) ;
#28839 = CARTESIAN_POINT ( 'NONE',  ( 122.6667014775786413, -7.893985811506177619, -18.51759400769804742 ) ) ;
#28840 = CARTESIAN_POINT ( 'NONE',  ( 120.5110881442453206, -6.344957434206665248, -7.627207830600338134 ) ) ;
#28841 = ORIENTED_EDGE ( 'NONE', *, *, #13370, .F. ) ;
#28842 = CARTESIAN_POINT ( 'NONE',  ( 119.7736414775786358, 0.1319031606808879209, -14.10382304977623669 ) ) ;
#28843 = CARTESIAN_POINT ( 'NONE',  ( 111.7184548109119788, -9.261995988541697145, -16.69588392320189030 ) ) ;
#28844 = CARTESIAN_POINT ( 'NONE',  ( 116.7671281442453335, -1.834011780172310813, -8.268836392978581529 ) ) ;
#28845 = CARTESIAN_POINT ( 'NONE',  ( 120.6812681442452941, 0.1319031606808879209, -14.10382304977623669 ) ) ;
#28846 = EDGE_LOOP ( 'NONE', ( #10575, #8911, #4075, #1825 ) ) ;
#28847 = CARTESIAN_POINT ( 'NONE',  ( 116.4635497909088429, -1.016270020561755860, -17.26805140881366896 ) ) ;
#28848 = AXIS2_PLACEMENT_3D ( 'NONE', #35899, #3990, #31587 ) ;
#28849 = CARTESIAN_POINT ( 'NONE',  ( 119.7736414775786358, -10.30919188438810075, -12.61870101168855918 ) ) ;
#28850 = CARTESIAN_POINT ( 'NONE',  ( 136.8967026949522676, 0.6524655654276926287, -12.96421432964295128 ) ) ;
#28851 = CARTESIAN_POINT ( 'NONE',  ( 109.7185827545247889, -2.477300249445798297, -19.15521520033831138 ) ) ;
#28852 = DIRECTION ( 'NONE',  ( -0.2768435750659113959, -0.3568721902840756854, 0.8921882507333144252 ) ) ;
#28853 = CARTESIAN_POINT ( 'NONE',  ( -12.61278219666105649, -4.053125158562569830, -8.893215200338314474 ) ) ;
#28854 = CARTESIAN_POINT ( 'NONE',  ( 114.5108483795247878, -8.402594152722688392, -16.93181055722141792 ) ) ;
#28855 = CARTESIAN_POINT ( 'NONE',  ( 117.9583881442453048, -10.30919188438810075, -12.61870101168855918 ) ) ;
#28856 = AXIS2_PLACEMENT_3D ( 'NONE', #12859, #16502, #29948 ) ;
#28857 = CARTESIAN_POINT ( 'NONE',  ( 112.3781902440515665, -2.467220198592768199, -17.83387418641523325 ) ) ;
#28858 = CARTESIAN_POINT ( 'NONE',  ( 115.6325948109119821, -9.565557343593413364, -10.61323700422348004 ) ) ;
#28859 = CARTESIAN_POINT ( 'NONE',  ( 126.2471382750653390, -0.7355600668381890861, -10.54709472444621099 ) ) ;
#28860 = CARTESIAN_POINT ( 'NONE',  ( 117.6180281442453150, -8.899110576539721151, -16.42337572283488711 ) ) ;
#28861 = CARTESIAN_POINT ( 'NONE',  ( 112.7745202545247878, 0.1403307496149616695, -11.32035403202665336 ) ) ;
#28862 = CARTESIAN_POINT ( 'NONE',  ( 113.6471614775786492, -4.153390946401321671, -8.397313243818183892 ) ) ;
#28863 = CARTESIAN_POINT ( 'NONE',  ( 93.44708369096697709, -25.99489077589524300, -13.39321520033831447 ) ) ;
#28864 = AXIS2_PLACEMENT_3D ( 'NONE', #30716, #16359, #26845 ) ;
#28865 = CARTESIAN_POINT ( 'NONE',  ( 78.69189222814998175, -71.37806158163368764, -41.02281774838951378 ) ) ;
#28867 = CARTESIAN_POINT ( 'NONE',  ( 118.0718414775786300, -9.261995988541697145, -16.69588392320189030 ) ) ;
#28866 = CARTESIAN_POINT ( 'NONE',  ( 63.98210704970577467, -13.60563849168869943, -8.547981236546295492 ) ) ;
#28868 = CARTESIAN_POINT ( 'NONE',  ( 119.7736414775786358, 0.1319031606808879209, -14.10382304977623669 ) ) ;
#28869 = CARTESIAN_POINT ( 'NONE',  ( 114.3278814775786429, 0.1319031606808879209, -14.10382304977623669 ) ) ;
#28870 = EDGE_LOOP ( 'NONE', ( #44813, #10243, #35417, #36080 ) ) ;
#28871 = CARTESIAN_POINT ( 'NONE',  ( 135.5886503745772984, -7.067465569328434505, -7.812523301970706768 ) ) ;
#28872 = CARTESIAN_POINT ( 'NONE',  ( 122.3830681442452857, -8.166667518702819706, -8.995218007635861213 ) ) ;
#28873 = CARTESIAN_POINT ( 'NONE',  ( 113.0523327545247838, -6.936859964151250502, -8.388885654883777576 ) ) ;
#28874 = CARTESIAN_POINT ( 'NONE',  ( 118.6391081442452986, -5.574606645277164318, -18.38911715685844683 ) ) ;
#28875 = AXIS2_PLACEMENT_3D ( 'NONE', #42041, #11480, #13995 ) ;
#28876 = CARTESIAN_POINT ( 'NONE',  ( 117.5613014775786525, -10.15424416112533912, -14.75197769757731336 ) ) ;
#28877 = CARTESIAN_POINT ( 'NONE',  ( 84.98581999809579202, -29.69064069796288052, -10.86172087519381435 ) ) ;
#28878 = CARTESIAN_POINT ( 'NONE',  ( 107.8433483795247838, -0.7896495226426338832, -9.318865927141430916 ) ) ;
#28879 = CARTESIAN_POINT ( 'NONE',  ( 123.4608748109119745, 0.4262465694468514643, -12.03445270309931736 ) ) ;
#28880 = CARTESIAN_POINT ( 'NONE',  ( 122.6099748109119929, -0.8288870151387760510, -10.36305467784173118 ) ) ;
#28881 = CARTESIAN_POINT ( 'NONE',  ( 115.0086014775786509, -5.574606645277172312, -18.38911715685844683 ) ) ;
#28882 = CARTESIAN_POINT ( 'NONE',  ( 109.2294668361295749, -3.968295118983554026, -7.926221972760173706 ) ) ;
#28883 = CARTESIAN_POINT ( 'NONE',  ( 120.0907204359119760, -10.25716656981731489, -12.88942061488890545 ) ) ;
#28884 = CARTESIAN_POINT ( 'NONE',  ( 116.5944421295247793, 0.8980012041604618078, -13.39321520033831447 ) ) ;
#28885 = PRODUCT ( 'Clamp Bolt', 'Clamp Bolt', '', ( #39149 ) ) ;
#28886 = FACE_OUTER_BOUND ( 'NONE', #959, .T. ) ;
#28887 = FACE_OUTER_BOUND ( 'NONE', #18695, .T. ) ;
#28888 = CARTESIAN_POINT ( 'NONE',  ( 116.8805814775786445, -6.344957434206662583, -7.627207830600332805 ) ) ;
#28889 = CARTESIAN_POINT ( 'NONE',  ( 120.0572748109119772, -3.383040157471821630, -19.15922257007629170 ) ) ;
#28890 = CARTESIAN_POINT ( 'NONE',  ( 110.7603796295247918, -4.863998795839590272, -19.15521520033831493 ) ) ;
#28891 = CARTESIAN_POINT ( 'NONE',  ( 111.8319081442453182, -5.638512984488999180, -18.83840828888717311 ) ) ;
#28892 = ORIENTED_EDGE ( 'NONE', *, *, #37975, .T. ) ;
#28893 = CARTESIAN_POINT ( 'NONE',  ( 112.8721930757767495, -0.9924539043446216624, -17.29976612834909133 ) ) ;
#28894 = CARTESIAN_POINT ( 'NONE',  ( 117.4478481442453131, 0.2603800115204892296, -16.42320221600525088 ) ) ;
#28895 = CARTESIAN_POINT ( 'NONE',  ( 123.6877814775786533, -6.222761293078241884, -8.102969835052219238 ) ) ;
#28896 = AXIS2_PLACEMENT_3D ( 'NONE', #2129, #19932, #33818 ) ;
#28897 = CARTESIAN_POINT ( 'NONE',  ( 0.000000000000000000, 0.000000000000000000, 0.000000000000000000 ) ) ;
#28898 = CARTESIAN_POINT ( 'NONE',  ( 123.8579614775786126, 0.5811942927096110934, -14.16772938898807510 ) ) ;
#28899 = CARTESIAN_POINT ( 'NONE',  ( 122.0994348109119443, 0.9020085738987339008, -11.91225656197089222 ) ) ;
#28900 = VECTOR ( 'NONE', #20083, 1000.000000000000000 ) ;
#28901 = CARTESIAN_POINT ( 'NONE',  ( 114.5803015045248117, -2.477300249445798297, -7.631215200338321125 ) ) ;
#28902 = CARTESIAN_POINT ( 'NONE',  ( 117.7314814775786260, -5.574606645277164318, -18.38911715685844683 ) ) ;
#28903 = CARTESIAN_POINT ( 'NONE',  ( 122.1048610609119720, -3.163656168406935087, -18.89861972220014508 ) ) ;
#28904 = CARTESIAN_POINT ( 'NONE',  ( 94.20708369096698220, -26.84634622004463012, -12.68105978249595189 ) ) ;
#28905 = ORIENTED_EDGE ( 'NONE', *, *, #11962, .T. ) ;
#28906 = AXIS2_PLACEMENT_3D ( 'NONE', #39674, #5231, #19145 ) ;
#28907 = CARTESIAN_POINT ( 'NONE',  ( 120.6463454359119822, 0.5291689781388270175, -13.89700978578772705 ) ) ;
#28908 = CARTESIAN_POINT ( 'NONE',  ( 120.7947214775786193, -9.261995988541697145, -16.69588392320189030 ) ) ;
#28909 = ORIENTED_EDGE ( 'NONE', *, *, #798, .T. ) ;
#28910 = CARTESIAN_POINT ( 'NONE',  ( 124.9252281442453096, -8.862178061932084461, -16.39564131203287545 ) ) ;
#28911 = CARTESIAN_POINT ( 'NONE',  ( -13.61798799253326564, -4.713664127232092937, -7.789724229335226902 ) ) ;
#28912 = CARTESIAN_POINT ( 'NONE',  ( 115.5212212410415873, 0.7607806665037644134, -12.14321520033829493 ) ) ;
#28913 = CARTESIAN_POINT ( 'NONE',  ( 115.0653281442453277, -3.505236298600246325, -18.68346056562440793 ) ) ;
#28914 = CARTESIAN_POINT ( 'NONE',  ( 66.08999561209553519, -0.1327762451593314241, -16.39321520033831447 ) ) ;
#28915 = CARTESIAN_POINT ( 'NONE',  ( 64.12920981708656143, -35.11750645889024014, -5.893215200338315363 ) ) ;
#28916 = CARTESIAN_POINT ( 'NONE',  ( 123.0637881442452937, -8.899110576539710493, -16.42337572283490132 ) ) ;
#28917 = EDGE_CURVE ( 'NONE', #2648, #28126, #1039, .T. ) ;
#28918 = ADVANCED_FACE ( 'NONE', ( #3970 ), #45085, .T. ) ;
#28919 = DIRECTION ( 'NONE',  ( -0.000000000000000000, -0.9284778069183721172, -0.3713878862591650232 ) ) ;
#28920 = CARTESIAN_POINT ( 'NONE',  ( 123.0637881442452937, -8.899110576539710493, -16.42337572283490132 ) ) ;
#28921 = CARTESIAN_POINT ( 'NONE',  ( 125.0302870206147787, -11.97677892521326903, -10.86299592855657359 ) ) ;
#28922 = AXIS2_PLACEMENT_3D ( 'NONE', #43487, #39837, #26604 ) ;
#28923 = CARTESIAN_POINT ( 'NONE',  ( 124.4252281442452812, -0.8288870151387760510, -10.36305467784173118 ) ) ;
#28924 = CARTESIAN_POINT ( 'NONE',  ( 112.9097148109120070, 0.2603800115204892296, -16.42320221600525088 ) ) ;
#28925 = CARTESIAN_POINT ( 'NONE',  ( 120.0005481442453146, -5.638512984488999180, -18.83840828888717311 ) ) ;
#28926 = CARTESIAN_POINT ( 'NONE',  ( 113.4769814775786330, -10.63000616557722466, -14.87417383870573495 ) ) ;
#28927 = CARTESIAN_POINT ( 'NONE',  ( 83.75466360696344736, -7.807702403958562520, -18.64321520033831803 ) ) ;
#28928 = CARTESIAN_POINT ( 'NONE',  ( 121.1350814775786233, -9.859900752359378018, -12.68260735090039759 ) ) ;
#28929 = ORIENTED_EDGE ( 'NONE', *, *, #38276, .F. ) ;
#28930 = CARTESIAN_POINT ( 'NONE',  ( 121.2485348109119769, -0.4660016031367893996, -10.09054647747474043 ) ) ;
#28931 = CARTESIAN_POINT ( 'NONE',  ( 113.3301452545248083, -9.868328341294098749, -15.46607636864997204 ) ) ;
#28932 = CARTESIAN_POINT ( 'NONE',  ( 82.42994493343583429, -31.76310523276723430, -22.89321520033831803 ) ) ;
#28933 = CYLINDRICAL_SURFACE ( 'NONE', #31903, 2.000000000000001776 ) ;
#28934 = CARTESIAN_POINT ( 'NONE',  ( 138.2184548109120499, -3.542396227776595019, -16.40211655196756979 ) ) ;
#28935 = CARTESIAN_POINT ( 'NONE',  ( 116.9417077545247992, -2.791137627527939813, -18.39754474579286025 ) ) ;
#28936 = VERTEX_POINT ( 'NONE', #8360 ) ;
#28937 = CARTESIAN_POINT ( 'NONE',  ( 122.7234281442452755, -4.153390946401325223, -8.397313243818185668 ) ) ;
#28938 = CARTESIAN_POINT ( 'NONE',  ( -13.56828337869051104, -4.779084862086333985, -17.89321520033831447 ) ) ;
#28939 = CARTESIAN_POINT ( 'NONE',  ( 109.2324108795247923, -1.325403438956436419, -16.93181055722137174 ) ) ;
#28940 = AXIS2_PLACEMENT_3D ( 'NONE', #2204, #8835, #36191 ) ;
#28941 = CARTESIAN_POINT ( 'NONE',  ( 120.8160396737536928, -8.611453504372539314, -17.77011218421760574 ) ) ;
#28942 = CARTESIAN_POINT ( 'NONE',  ( 108.6073327545248048, -6.936859964151250502, -8.388885654883777576 ) ) ;
#28943 = ADVANCED_FACE ( 'NONE', ( #22709 ), #10253, .T. ) ;
#28944 = ORIENTED_EDGE ( 'NONE', *, *, #12244, .F. ) ;
#28945 = CARTESIAN_POINT ( 'NONE',  ( 115.9729548109119861, -6.344957434206662583, -7.627207830600332805 ) ) ;
#28946 = CARTESIAN_POINT ( 'NONE',  ( 88.82299970795220645, -11.01275678708395489, -14.13803923971916632 ) ) ;
#28947 = CARTESIAN_POINT ( 'NONE',  ( 120.2274548109119934, -9.859900752359374465, -12.68260735090039404 ) ) ;
#28948 = FACE_OUTER_BOUND ( 'NONE', #13649, .T. ) ;
#28949 = CARTESIAN_POINT ( 'NONE',  ( 70.19189222814998175, -100.0979043305785581, -53.24182196210380624 ) ) ;
#28950 = CARTESIAN_POINT ( 'NONE',  ( 67.84197459855160162, -52.72621824513493038, -35.02248567325151640 ) ) ;
#28951 = CARTESIAN_POINT ( 'NONE',  ( 110.4361338361194811, 0.1075849324168598464, -12.14321520033833046 ) ) ;
#28952 = EDGE_CURVE ( 'NONE', #36034, #5046, #24817, .T. ) ;
#28953 = SURFACE_SIDE_STYLE ('',( #29165 ) ) ;
#28954 = ORIENTED_EDGE ( 'NONE', *, *, #32524, .F. ) ;
#28955 = EDGE_CURVE ( 'NONE', #19203, #29206, #26589, .T. ) ;
#28956 = DIRECTION ( 'NONE',  ( 0.8636456077245092677, -0.5040994586965584778, 0.000000000000000000 ) ) ;
#28957 = AXIS2_PLACEMENT_3D ( 'NONE', #13566, #44809, #33606 ) ;
#28958 = CARTESIAN_POINT ( 'NONE',  ( 122.0427081442452817, 0.5811942927096110934, -14.16772938898807510 ) ) ;
#28959 = CARTESIAN_POINT ( 'NONE',  ( 136.9394333025971093, -9.868690179724596945, -15.68633195852948248 ) ) ;
#28960 = ORIENTED_EDGE ( 'NONE', *, *, #1177, .F. ) ;
#28961 = CARTESIAN_POINT ( 'NONE',  ( 112.2857214775786474, -4.089484607189486809, -7.948022111789456723 ) ) ;
#28962 = CARTESIAN_POINT ( 'NONE',  ( 111.4915481442453142, -1.833838273342658365, -17.42832698103878286 ) ) ;
#28963 = EDGE_CURVE ( 'NONE', #9582, #42332, #1954, .T. ) ;
#28964 = CARTESIAN_POINT ( 'NONE',  ( 110.5266510812576826, -0.01829820670803256055, -12.14321520033831625 ) ) ;
#28965 = CARTESIAN_POINT ( 'NONE',  ( 121.9292548109119849, -7.894159318335828068, -9.358103419637847864 ) ) ;
#28966 = EDGE_LOOP ( 'NONE', ( #12401, #11243, #39081, #30132, #21686 ) ) ;
#28967 = CARTESIAN_POINT ( 'NONE',  ( 119.2631014775786298, 0.2603800115204892296, -16.42320221600525088 ) ) ;
#28968 = CARTESIAN_POINT ( 'NONE',  ( 87.02785693856107230, -25.99489077589524300, -13.39321520033831447 ) ) ;
#28969 = ADVANCED_FACE ( 'NONE', ( #40271 ), #11708, .F. ) ;
#28970 = CARTESIAN_POINT ( 'NONE',  ( 79.41838382432698040, 5.053604680061214438, -20.45601830029449530 ) ) ;
#28971 = EDGE_CURVE ( 'NONE', #26936, #26522, #44378, .T. ) ;
#28972 = ADVANCED_FACE ( 'NONE', ( #13369 ), #13140, .F. ) ;
#28973 = CARTESIAN_POINT ( 'NONE',  ( 137.4945747550012811, -3.899949230086460883, -8.466937502284467953 ) ) ;
#28974 = CARTESIAN_POINT ( 'NONE',  ( 112.1722681442453222, -8.899110576539710493, -16.42337572283490132 ) ) ;
#28975 = DIRECTION ( 'NONE',  ( 1.156482317317869950E-15, 1.000000000000000000, 0.000000000000000000 ) ) ;
#28976 = FACE_OUTER_BOUND ( 'NONE', #12986, .T. ) ;
#28977 = CARTESIAN_POINT ( 'NONE',  ( 112.6828081442453282, -2.084020599724406786, -8.691656652584148546 ) ) ;
#28978 = CARTESIAN_POINT ( 'NONE',  ( 112.1722681442453222, -0.4660016031367893996, -10.09054647747474043 ) ) ;
#28979 = CARTESIAN_POINT ( 'NONE',  ( 116.6714741698188504, -8.633658976779720717, -16.79467234361142047 ) ) ;
#28980 = CARTESIAN_POINT ( 'NONE',  ( 125.1059481442452750, -1.833838273342660141, -17.42832698103878286 ) ) ;
#28981 = CARTESIAN_POINT ( 'NONE',  ( 121.4187148109119789, -6.344957434206665248, -7.627207830600338134 ) ) ;
#28982 = ORIENTED_EDGE ( 'NONE', *, *, #13331, .F. ) ;
#28983 = CARTESIAN_POINT ( 'NONE',  ( 126.5561942423968844, -8.545838888952497214, -17.02113326143807726 ) ) ;
#28984 = CARTESIAN_POINT ( 'NONE',  ( 115.3442858795247759, -0.7896495226426338832, -17.46756447353520159 ) ) ;
#28985 = CARTESIAN_POINT ( 'NONE',  ( 113.8163171295247764, 0.1403307496149613920, -13.39321520033831447 ) ) ;
#28986 = CARTESIAN_POINT ( 'NONE',  ( 114.7192077545248594, -2.791137627527939813, -18.39754474579286025 ) ) ;
#28987 = CARTESIAN_POINT ( 'NONE',  ( 126.9932531981154966, -9.953270824051303478, -11.62590261691779858 ) ) ;
#28988 = CARTESIAN_POINT ( 'NONE',  ( 115.5758681442453053, -1.561330072975668060, -17.79121239304076951 ) ) ;
#28989 = ORIENTED_EDGE ( 'NONE', *, *, #34052, .F. ) ;
#28990 = CARTESIAN_POINT ( 'NONE',  ( 113.0798948109119948, -8.899110576539710493, -16.42337572283490132 ) ) ;
#28991 = CARTESIAN_POINT ( 'NONE',  ( 70.19189222814998175, -56.69156685714467159, -35.87943827948784303 ) ) ;
#28992 = CARTESIAN_POINT ( 'NONE',  ( 72.54180985774836188, -53.22909301380743585, -33.76528779565084903 ) ) ;
#28993 = CARTESIAN_POINT ( 'NONE',  ( 120.3439060953690642, -6.001247023715329476, -18.26661038929047720 ) ) ;
#28994 = CARTESIAN_POINT ( 'NONE',  ( 109.2295025952882526, -0.04762797407389267323, -15.11742090230669611 ) ) ;
#28995 = CARTESIAN_POINT ( 'NONE',  ( -12.55641747516330575, -4.307035652475513565, -19.39321520033831447 ) ) ;
#28996 = CARTESIAN_POINT ( 'NONE',  ( 114.9518748109119883, -1.834011780172310813, -8.268836392978581529 ) ) ;
#28997 = CARTESIAN_POINT ( 'NONE',  ( 110.8992858795247827, -0.7896495226426338832, -17.46756447353520159 ) ) ;
#28998 = CARTESIAN_POINT ( 'NONE',  ( 113.6774108795247997, -1.325403438956436419, -16.93181055722141792 ) ) ;
#28999 = VERTEX_POINT ( 'NONE', #24079 ) ;
#29000 = DIRECTION ( 'NONE',  ( -0.000000000000000000, -0.9284778069183721172, -0.3713878862591650232 ) ) ;
#29001 = CARTESIAN_POINT ( 'NONE',  ( 120.6812681442452941, 0.1319031606808879209, -14.10382304977623669 ) ) ;
#29002 = CARTESIAN_POINT ( 'NONE',  ( 117.2209414775786485, -7.893985811506177619, -18.51759400769804742 ) ) ;
#29003 = CARTESIAN_POINT ( 'NONE',  ( 111.8886348109120092, -3.383040157471821630, -19.15922257007629170 ) ) ;
#29004 = CARTESIAN_POINT ( 'NONE',  ( 123.5176014775786228, -0.8288870151387760510, -10.36305467784173118 ) ) ;
#29005 = CARTESIAN_POINT ( 'NONE',  ( 124.7088614775786226, -9.565557343593413364, -10.61323700422348004 ) ) ;
#29006 = CARTESIAN_POINT ( 'NONE',  ( 114.6682414775786469, -7.894159318335828068, -9.358103419637847864 ) ) ;
#29007 = ORIENTED_EDGE ( 'NONE', *, *, #11389, .F. ) ;
#29008 = CARTESIAN_POINT ( 'NONE',  ( 121.1325173109119788, 0.2312338769422704887, -16.08380026872395874 ) ) ;
#29009 = DIRECTION ( 'NONE',  ( -0.7871354856660202071, 0.6167752151498580027, 0.002461946824133919541 ) ) ;
#29010 = CARTESIAN_POINT ( 'NONE',  ( 118.5823814775786360, -7.643976991954077427, -18.09477374809248928 ) ) ;
#29011 = ORIENTED_EDGE ( 'NONE', *, *, #32345, .T. ) ;
#29012 = FACE_OUTER_BOUND ( 'NONE', #37926, .T. ) ;
#29013 = EDGE_CURVE ( 'NONE', #21529, #15102, #13811, .T. ) ;
#29014 = CARTESIAN_POINT ( 'NONE',  ( 116.4267681442453153, -3.383040157471821630, -19.15922257007629170 ) ) ;
#29015 = CARTESIAN_POINT ( 'NONE',  ( 114.6497546295247929, -4.863998795839590272, -7.631215200338315796 ) ) ;
#29016 = CARTESIAN_POINT ( 'NONE',  ( 125.5030348109119558, -6.222761293078241884, -8.102969835052219238 ) ) ;
#29017 = ORIENTED_EDGE ( 'NONE', *, *, #30672, .T. ) ;
#29018 = EDGE_LOOP ( 'NONE', ( #21869, #18153, #39538, #44138 ) ) ;
#29019 = CARTESIAN_POINT ( 'NONE',  ( 122.9503348109119827, -9.859900752359378018, -12.68260735090039759 ) ) ;
#29020 = CARTESIAN_POINT ( 'NONE',  ( 115.8595014775786609, -7.643976991954077427, -18.09477374809248928 ) ) ;
#29021 = CARTESIAN_POINT ( 'NONE',  ( 124.5685810787103662, -9.850217616288844624, -13.79100485233420770 ) ) ;
#29022 = CARTESIAN_POINT ( 'NONE',  ( 122.0354079359119908, -5.444069387712269226, -19.60292469916370450 ) ) ;
#29023 = ORIENTED_EDGE ( 'NONE', *, *, #10840, .T. ) ;
#29024 = CARTESIAN_POINT ( 'NONE',  ( 112.1719155697224295, -8.904739562214000870, -16.41571553851813547 ) ) ;
#29025 = CARTESIAN_POINT ( 'NONE',  ( 3.060777270043529619, -5.064559853354640317, -17.89321520033831447 ) ) ;
#29026 = CARTESIAN_POINT ( 'NONE',  ( 110.6909265045248247, -7.250697342233347165, -19.15521520033831138 ) ) ;
#29027 = CARTESIAN_POINT ( 'NONE',  ( 112.2857214775786474, -4.089484607189486809, -7.948022111789456723 ) ) ;
#29028 = CARTESIAN_POINT ( 'NONE',  ( 126.5808414775786446, -9.859900752359378018, -12.68260735090039759 ) ) ;
#29029 = EDGE_CURVE ( 'NONE', #42684, #17900, #4582, .T. ) ;
#29030 = CARTESIAN_POINT ( 'NONE',  ( 121.8158014775786171, -4.153390946401325223, -8.397313243818185668 ) ) ;
#29031 = CARTESIAN_POINT ( 'NONE',  ( 109.2294421295247844, -49.76310523276723785, -19.39321520033831447 ) ) ;
#29032 = VERTEX_POINT ( 'NONE', #13588 ) ;
#29033 = CARTESIAN_POINT ( 'NONE',  ( 119.6034614775786196, -3.505236298600246325, -18.68346056562440793 ) ) ;
#29034 = CARTESIAN_POINT ( 'NONE',  ( 116.0388171295248014, -10.62599879583958540, -13.39321520033831447 ) ) ;
#29035 = CARTESIAN_POINT ( 'NONE',  ( 114.2354127111058659, -1.267766418764742165, -16.93314635290707315 ) ) ;
#29036 = CARTESIAN_POINT ( 'NONE',  ( 114.4413952545248350, 0.8980012041604421569, -11.00651665394454071 ) ) ;
#29037 = CARTESIAN_POINT ( 'NONE',  ( 117.3343948109119737, -3.383040157471821630, -19.15922257007629170 ) ) ;
#29038 = ORIENTED_EDGE ( 'NONE', *, *, #7431, .F. ) ;
#29039 = CARTESIAN_POINT ( 'NONE',  ( 116.4267681442453153, -3.383040157471821630, -19.15922257007629170 ) ) ;
#29040 = CARTESIAN_POINT ( 'NONE',  ( 96.46827370896536991, -26.13949388144357755, -14.39191870720298994 ) ) ;
#29041 = CARTESIAN_POINT ( 'NONE',  ( 105.6208483795248299, -0.7896495226426338832, -9.318865927141430916 ) ) ;
#29042 = CARTESIAN_POINT ( 'NONE',  ( 117.2209414775786485, -7.893985811506177619, -18.51759400769804742 ) ) ;
#29043 = CARTESIAN_POINT ( 'NONE',  ( 118.6391081442452986, -4.089484607189486809, -7.948022111789456723 ) ) ;
#29044 = CARTESIAN_POINT ( 'NONE',  ( 125.6164881442453094, -9.565557343593413364, -10.61323700422348004 ) ) ;
#29045 = CARTESIAN_POINT ( 'NONE',  ( 120.7979673576684831, -6.302457937304708935, -18.83702152638930372 ) ) ;
#29046 = DIRECTION ( 'NONE',  ( 0.000000000000000000, -0.3818493186865936084, 0.9242245927363024194 ) ) ;
#29047 = ORIENTED_EDGE ( 'NONE', *, *, #6360, .T. ) ;
#29048 = CARTESIAN_POINT ( 'NONE',  ( 112.2334103192116999, -2.378957183258581853, -17.95140958770220152 ) ) ;
#29049 = CARTESIAN_POINT ( 'NONE',  ( 109.2294421416092689, -10.38236770277540622, -13.95981693459670048 ) ) ;
#29050 = CARTESIAN_POINT ( 'NONE',  ( 119.8870948109119752, -0.8288870151387760510, -10.36305467784173118 ) ) ;
#29051 = AXIS2_PLACEMENT_3D ( 'NONE', #25016, #28672, #3590 ) ;
#29052 = CARTESIAN_POINT ( 'NONE',  ( 111.8021765045248372, -2.791137627527939813, -8.388885654883777576 ) ) ;
#29053 = CARTESIAN_POINT ( 'NONE',  ( 106.5931921295248372, 0.8980012041604618078, -13.39321520033831447 ) ) ;
#29054 = CARTESIAN_POINT ( 'NONE',  ( 113.0231681442453180, -10.15424416112533912, -14.75197769757731336 ) ) ;
#29055 = CARTESIAN_POINT ( 'NONE',  ( 70.19189222814998175, -62.44811955051406471, -34.95094429002801206 ) ) ;
#29056 = CARTESIAN_POINT ( 'NONE',  ( 124.4252281442452812, -9.261995988541697145, -16.69588392320189030 ) ) ;
#29057 = CARTESIAN_POINT ( 'NONE',  ( 121.2485348109119769, -0.4660016031367893996, -10.09054647747474043 ) ) ;
#29058 = ORIENTED_EDGE ( 'NONE', *, *, #8324, .T. ) ;
#29059 = CARTESIAN_POINT ( 'NONE',  ( 119.2063748109119814, -7.894159318335828068, -9.358103419637847864 ) ) ;
#29060 = CARTESIAN_POINT ( 'NONE',  ( 111.9453614775786434, -1.561330072975668060, -17.79121239304076596 ) ) ;
#29061 = CARTESIAN_POINT ( 'NONE',  ( 122.7234281442452755, -5.638512984488999180, -18.83840828888717311 ) ) ;
#29062 = CARTESIAN_POINT ( 'NONE',  ( 119.6601881442453106, -1.833838273342659253, -17.42832698103878286 ) ) ;
#29063 = ORIENTED_EDGE ( 'NONE', *, *, #212, .F. ) ;
#29064 = CARTESIAN_POINT ( 'NONE',  ( 124.8223148109119762, -10.15424416112533912, -14.75197769757731336 ) ) ;
#29065 = CARTESIAN_POINT ( 'NONE',  ( 119.4900081442453086, -1.834011780172310813, -8.268836392978581529 ) ) ;
#29066 = CARTESIAN_POINT ( 'NONE',  ( 125.3296504289713766, -7.415504751769019798, -6.746157367331738541 ) ) ;
#29067 = DIRECTION ( 'NONE',  ( 0.000000000000000000, -0.9242245927363029745, -0.3818493186865929978 ) ) ;
#29068 = CARTESIAN_POINT ( 'NONE',  ( 126.2184548109119504, 0.09929810886256085212, -14.00506970868240231 ) ) ;
#29069 = CARTESIAN_POINT ( 'NONE',  ( 114.2330358795247776, -8.402594152722688392, -9.854619843455216355 ) ) ;
#29070 = CARTESIAN_POINT ( 'NONE',  ( 117.1074881442453233, -10.63000616557722466, -14.87417383870573495 ) ) ;
#29071 = EDGE_CURVE ( 'NONE', #38280, #28936, #6748, .T. ) ;
#29072 = AXIS2_PLACEMENT_3D ( 'NONE', #23611, #3071, #10595 ) ;
#29073 = CARTESIAN_POINT ( 'NONE',  ( 137.3527759848280141, -9.837515720139910158, -11.99256683774707177 ) ) ;
#29074 = CARTESIAN_POINT ( 'NONE',  ( 116.0864081442453113, -0.1624402480850797581, -16.17319339645315424 ) ) ;
#29075 = CARTESIAN_POINT ( 'NONE',  ( 111.6617281442453304, 0.4262465694468514643, -12.03445270309931736 ) ) ;
#29076 = CARTESIAN_POINT ( 'NONE',  ( 126.3230600034097364, -0.6023121577465754273, -10.67916527035535168 ) ) ;
#29077 = CARTESIAN_POINT ( 'NONE',  ( 109.7880358795247986, -8.402594152722688392, -9.854619843455216355 ) ) ;
#29078 = CARTESIAN_POINT ( 'NONE',  ( 113.4202548109119846, 0.1319031606808879209, -14.10382304977623669 ) ) ;
#29079 = CARTESIAN_POINT ( 'NONE',  ( 114.9466624678160969, -1.149058757900091265, -17.09122335155388939 ) ) ;
#29080 = DIRECTION ( 'NONE',  ( -1.000000000000000000, 0.000000000000000000, -0.000000000000000000 ) ) ;
#29082 = CARTESIAN_POINT ( 'NONE',  ( 119.1496481442453046, -3.383040157471821630, -19.15922257007629170 ) ) ;
#29081 = CARTESIAN_POINT ( 'NONE',  ( 61.00844462485471098, -13.32659074696883117, -7.515841235333575732 ) ) ;
#29083 = CARTESIAN_POINT ( 'NONE',  ( 124.3685014775786328, 0.4262465694468514643, -12.03445270309931736 ) ) ;
#29084 = ORIENTED_EDGE ( 'NONE', *, *, #35301, .T. ) ;
#29085 = CARTESIAN_POINT ( 'NONE',  ( 137.0596819398186028, -7.194705560345089346, -8.499707714596844710 ) ) ;
#29086 = CARTESIAN_POINT ( 'NONE',  ( 75.95778847736514194, -3.256761025687008537, -12.39321520033831447 ) ) ;
#29087 = CARTESIAN_POINT ( 'NONE',  ( 112.9134265045247645, -2.791137627527939813, -8.388885654883777576 ) ) ;
#29088 = CARTESIAN_POINT ( 'NONE',  ( 120.7947214775786193, -0.8288870151387760510, -10.36305467784173118 ) ) ;
#29089 =( BOUNDED_CURVE ( )  B_SPLINE_CURVE ( 2, ( #9791, #34814, #31195, #403, #2932 ),
 .UNSPECIFIED., .F., .T. ) 
 B_SPLINE_CURVE_WITH_KNOTS ( ( 3, 2, 3 ),
 ( 0.8750000000000000000, 0.8828125000000000000, 0.8891217583431300087 ),
 .UNSPECIFIED. ) 
 CURVE ( )  GEOMETRIC_REPRESENTATION_ITEM ( )  RATIONAL_B_SPLINE_CURVE ( ( 0.9999999999999800160, 0.9238795325113059453, 1.000000000000000000, 0.9385262470929799372, 0.9763430640194590282 ) ) 
 REPRESENTATION_ITEM ( '' )  );
#29090 = CARTESIAN_POINT ( 'NONE',  ( 121.1918081442452859, -10.15424416112533912, -14.75197769757731336 ) ) ;
#29091 = CARTESIAN_POINT ( 'NONE',  ( 115.9162281442453093, -5.574606645277164318, -18.38911715685844683 ) ) ;
#29092 = CARTESIAN_POINT ( 'NONE',  ( 86.15278414645355554, -26.86419576995684722, -8.486169908812993157 ) ) ;
#29093 = CARTESIAN_POINT ( 'NONE',  ( 110.0658483795247804, -0.7896495226426338832, -9.318865927141430916 ) ) ;
#29094 = CARTESIAN_POINT ( 'NONE',  ( 124.1983214775786166, -1.833838273342659697, -17.42832698103878286 ) ) ;
#29095 = CARTESIAN_POINT ( 'NONE',  ( 123.8012348109119642, -9.565557343593413364, -10.61323700422348004 ) ) ;
#29096 = DIRECTION ( 'NONE',  ( 0.000000000000000000, -0.3818493186865936084, 0.9242245927363024194 ) ) ;
#29097 = DIRECTION ( 'NONE',  ( 0.9609149988134837450, -0.1028163501681639419, 0.2570431154366518145 ) ) ;
#29098 = EDGE_CURVE ( 'NONE', #18562, #39160, #34317, .T. ) ;
#29099 = CARTESIAN_POINT ( 'NONE',  ( 124.0495485609119584, -10.36940331770106916, -15.09355782777062061 ) ) ;
#29100 = CARTESIAN_POINT ( 'NONE',  ( 114.0246765045248196, -7.250697342233347165, -19.15521520033831138 ) ) ;
#29101 = CARTESIAN_POINT ( 'NONE',  ( -13.37968822036932615, -5.027311996218202239, -18.18770968788854603 ) ) ;
#29102 = CARTESIAN_POINT ( 'NONE',  ( 71.67504600870660170, -26.72445618319088823, -4.893215200338314474 ) ) ;
#29103 = CARTESIAN_POINT ( 'NONE',  ( 117.9583881442453048, -10.30919188438810075, -12.61870101168855918 ) ) ;
#29104 = CARTESIAN_POINT ( 'NONE',  ( 119.8870948109119752, -9.261995988541697145, -16.69588392320189030 ) ) ;
#29105 = CARTESIAN_POINT ( 'NONE',  ( 107.2877233795247776, -8.938348069036489818, -17.46756447353520159 ) ) ;
#29106 = CARTESIAN_POINT ( 'NONE',  ( 113.7038881442453402, -3.383040157471821630, -19.15922257007629170 ) ) ;
#29107 = CARTESIAN_POINT ( 'NONE',  ( 87.44708369096657918, -21.99489077589588604, -20.89321520033831447 ) ) ;
#29108 = ORIENTED_EDGE ( 'NONE', *, *, #38421, .T. ) ;
#29109 = DIRECTION ( 'NONE',  ( -0.3445294493088589816, -0.9387755102040820088, 0.000000000000000000 ) ) ;
#29110 = CARTESIAN_POINT ( 'NONE',  ( 116.7671281442453335, -1.834011780172310813, -8.268836392978581529 ) ) ;
#29111 = AXIS2_PLACEMENT_3D ( 'NONE', #12243, #5602, #22713 ) ;
#29112 = CARTESIAN_POINT ( 'NONE',  ( 124.5954081442453116, -6.222761293078241884, -8.102969835052219238 ) ) ;
#29113 = APPLICATION_PROTOCOL_DEFINITION ( 'draft international standard', 'automotive_design', 1998, #18372 ) ;
#29114 = CARTESIAN_POINT ( 'NONE',  ( 113.8173414775786512, -9.565557343593413364, -10.61323700422348004 ) ) ;
#29115 = CARTESIAN_POINT ( 'NONE',  ( 120.9081748109119872, -5.638512984488999180, -18.83840828888717311 ) ) ;
#29116 = CARTESIAN_POINT ( 'NONE',  ( 112.2188952545247531, 0.8980012041604421569, -11.00651665394454071 ) ) ;
#29117 = CIRCLE ( 'NONE', #35743, 1.499999999999998002 ) ;
#29118 = CARTESIAN_POINT ( 'NONE',  ( 115.7460481442453357, -10.15424416112533912, -14.75197769757731336 ) ) ;
#29119 = CARTESIAN_POINT ( 'NONE',  ( 116.7606190177645402, -4.646879210594899945, -18.55939208857811451 ) ) ;
#29120 = DIRECTION ( 'NONE',  ( 0.000000000000000000, 0.000000000000000000, -1.000000000000000000 ) ) ;
#29121 = ORIENTED_EDGE ( 'NONE', *, *, #19491, .F. ) ;
#29122 = AXIS2_PLACEMENT_3D ( 'NONE', #2427, #37309, #23422 ) ;
#29123 = CARTESIAN_POINT ( 'NONE',  ( 122.6604860609119640, -6.564341423271550902, -7.887810678476487425 ) ) ;
#29124 = CARTESIAN_POINT ( 'NONE',  ( 118.4122014775786340, 0.5811942927096110934, -14.16772938898807510 ) ) ;
#29125 = VERTEX_POINT ( 'NONE', #16563 ) ;
#29126 = DIRECTION ( 'NONE',  ( 0.5040994586965589219, 0.8636456077245089347, 0.000000000000000000 ) ) ;
#29127 = CARTESIAN_POINT ( 'NONE',  ( 63.10250807381770244, -31.76310523276723430, -23.89321520033831803 ) ) ;
#29128 = CARTESIAN_POINT ( 'NONE',  ( 75.95778847736481509, -3.256761025687722189, -7.993215200338315007 ) ) ;
#29129 = CARTESIAN_POINT ( 'NONE',  ( 115.0086014775786509, -5.574606645277164318, -18.38911715685844683 ) ) ;
#29130 = CARTESIAN_POINT ( 'NONE',  ( 67.94976195724866841, -0.5658009588791762523, -16.39321520033831447 ) ) ;
#29131 = CARTESIAN_POINT ( 'NONE',  ( 64.01282776924010420, -34.86145050234441811, -5.893215200338315363 ) ) ;
#29132 = CARTESIAN_POINT ( 'NONE',  ( 123.9714148109119805, -8.899110576539710493, -16.42337572283490132 ) ) ;
#29133 = DIRECTION ( 'NONE',  ( -1.000000000000000000, 0.000000000000000000, 0.000000000000000000 ) ) ;
#29134 = CARTESIAN_POINT ( 'NONE',  ( 124.7655881442452852, -9.859900752359378018, -12.68260735090039759 ) ) ;
#29135 = CIRCLE ( 'NONE', #27691, 2.445500000000004448 ) ;
#29136 = CARTESIAN_POINT ( 'NONE',  ( 125.0526156892421454, -11.67076936788440022, -16.62222883760368930 ) ) ;
#29137 = CARTESIAN_POINT ( 'NONE',  ( 119.0929214775786278, -4.153390946401325223, -8.397313243818185668 ) ) ;
#29138 = CARTESIAN_POINT ( 'NONE',  ( 121.9292548109119849, -7.894159318335828068, -9.358103419637847864 ) ) ;
#29139 = CARTESIAN_POINT ( 'NONE',  ( 113.7606148109119886, -1.561330072975668060, -17.79121239304076596 ) ) ;
#29140 = CARTESIAN_POINT ( 'NONE',  ( 118.9794681442453026, -9.261995988541697145, -16.69588392320189030 ) ) ;
#29141 = CARTESIAN_POINT ( 'NONE',  ( 112.9664414775786412, 0.5811942927096154232, -14.16772938898807155 ) ) ;
#29142 = CARTESIAN_POINT ( 'NONE',  ( 69.69189222815028018, -41.76310523276638520, -14.39321520033831625 ) ) ;
#29143 = CARTESIAN_POINT ( 'NONE',  ( 122.9503348109119827, -9.859900752359378018, -12.68260735090039759 ) ) ;
#29144 = VERTEX_POINT ( 'NONE', #17017 ) ;
#29145 = CARTESIAN_POINT ( 'NONE',  ( 119.6601881442453106, -8.166667518702819706, -8.995218007635861213 ) ) ;
#29146 = CARTESIAN_POINT ( 'NONE',  ( 109.0935046295247872, -4.863998795839590272, -18.39754474579285315 ) ) ;
#29147 = CARTESIAN_POINT ( 'NONE',  ( 112.4967077545247633, -2.791137627527939813, -18.39754474579286025 ) ) ;
#29148 = CARTESIAN_POINT ( 'NONE',  ( 83.47559691244318003, -32.81415873735240041, -23.89321520033831803 ) ) ;
#29149 = CARTESIAN_POINT ( 'NONE',  ( 66.69189222814998175, -41.76310523276723785, -24.39321520033831447 ) ) ;
#29150 = AXIS2_PLACEMENT_3D ( 'NONE', #45126, #6373, #7040 ) ;
#29151 = CARTESIAN_POINT ( 'NONE',  ( 116.2471765045247594, -2.791137627527939813, -8.388885654883777576 ) ) ;
#29152 = ORIENTED_EDGE ( 'NONE', *, *, #1593, .T. ) ;
#29153 = AXIS2_PLACEMENT_3D ( 'NONE', #38318, #14160, #41333 ) ;
#29154 = CARTESIAN_POINT ( 'NONE',  ( 122.5532481442453019, 0.4262465694468514643, -12.03445270309931736 ) ) ;
#29155 = CARTESIAN_POINT ( 'NONE',  ( 120.8547048109119686, -7.554583864224885481, -18.48844787311982785 ) ) ;
#29156 = FACE_OUTER_BOUND ( 'NONE', #36218, .T. ) ;
#29157 = CARTESIAN_POINT ( 'NONE',  ( 106.6626452545248611, -9.868328341294098749, -15.46607636864997204 ) ) ;
#29158 = VERTEX_POINT ( 'NONE', #37515 ) ;
#29159 = CARTESIAN_POINT ( 'NONE',  ( 116.3133148109119759, -7.893985811506177619, -18.51759400769804742 ) ) ;
#29160 = CARTESIAN_POINT ( 'NONE',  ( 96.21525317080913453, -27.63241331390002031, -14.62699200570882851 ) ) ;
#29161 = CARTESIAN_POINT ( 'NONE',  ( 119.0929214775786278, -4.153390946401325223, -8.397313243818185668 ) ) ;
#29162 = DIRECTION ( 'NONE',  ( 0.000000000000000000, 0.000000000000000000, -1.000000000000000000 ) ) ;
#29163 = CARTESIAN_POINT ( 'NONE',  ( 111.2184548109119788, -8.862178061932382889, -16.39564131203247399 ) ) ;
#29164 = CARTESIAN_POINT ( 'NONE',  ( 71.50489436060276205, -24.57757939319463958, -4.893215200338314474 ) ) ;
#29165 = SURFACE_STYLE_FILL_AREA ( #15042 ) ;
#29166 = ORIENTED_EDGE ( 'NONE', *, *, #11363, .T. ) ;
#29167 = EDGE_CURVE ( 'NONE', #34887, #26514, #30655, .T. ) ;
#29168 = CARTESIAN_POINT ( 'NONE',  ( 116.7333483795247844, -8.402594152722688392, -16.93181055722141792 ) ) ;
#29169 = AXIS2_PLACEMENT_3D ( 'NONE', #315, #35631, #22188 ) ;
#29170 = CARTESIAN_POINT ( 'NONE',  ( 120.9081748109119872, -5.638512984488999180, -18.83840828888717311 ) ) ;
#29171 = B_SPLINE_CURVE_WITH_KNOTS ( 'NONE', 3,
 ( #36480, #1819, #1154, #8229, #5021, #25782, #18937, #11651, #1595, #12106 ),
 .UNSPECIFIED., .F., .F.,
 ( 4, 3, 3, 4 ),
 ( 0.000000000000000000, 0.0002476486447138990187, 0.0004952972925464390165, 0.0009604418836934789901 ),
 .UNSPECIFIED. ) ;
#29172 =( BOUNDED_SURFACE ( )  B_SPLINE_SURFACE ( 3, 2, ( 
 ( #27575, #20728, #3393 ),
 ( #31202, #13880, #27792 ),
 ( #24370, #8160, #39162 ),
 ( #25491, #36183, #21614 ),
 ( #25714, #42594, #4949 ),
 ( #32974, #43038, #11807 ),
 ( #14547, #28911, #1308 ),
 ( #35501, #36401, #15449 ),
 ( #4273, #22065, #7927 ),
 ( #39394, #18862, #18192 ) ),
 .UNSPECIFIED., .F., .F., .F. ) 
 B_SPLINE_SURFACE_WITH_KNOTS ( ( 4, 2, 2, 2, 4 ),
 ( 3, 3 ),
 ( 0.0008626443591432887605, 0.001000512151876073409, 0.001138379944608858057, 0.001276247737341642706, 0.001414115530074427354 ),
 ( 0.000000000000000000, 1.000000000000000000 ),
 .UNSPECIFIED. ) 
 GEOMETRIC_REPRESENTATION_ITEM ( )  RATIONAL_B_SPLINE_SURFACE ( (
 ( 1.000000000000000000, 0.9079001203735632686, 1.000000000000000000),
 ( 1.000000000000000000, 0.9079951794695932943, 1.000000000000000000),
 ( 1.000000000000000000, 0.9016384734332488771, 1.000000000000000000),
 ( 1.000000000000000000, 0.8796635664893247553, 1.000000000000000000),
 ( 1.000000000000000000, 0.8641413844937639865, 1.000000000000000000),
 ( 1.000000000000000000, 0.8276919187008282552, 1.000000000000000000),
 ( 1.000000000000000000, 0.8062482852324636129, 1.000000000000000000),
 ( 1.000000000000000000, 0.7597475340234437491, 1.000000000000000000),
 ( 1.000000000000000000, 0.7345850491789025494, 1.000000000000000000),
 ( 1.000000000000000000, 0.7071067811865467956, 1.000000000000000000) ) ) 
 REPRESENTATION_ITEM ( '' )  SURFACE ( )  );
#29173 = CARTESIAN_POINT ( 'NONE',  ( 136.2315975805980486, -10.28294944029322444, -15.60456038644257148 ) ) ;
#29174 = ORIENTED_EDGE ( 'NONE', *, *, #5828, .T. ) ;
#29175 = CARTESIAN_POINT ( 'NONE',  ( 115.0653281442453277, -6.344957434206662583, -7.627207830600332805 ) ) ;
#29176 = CARTESIAN_POINT ( 'NONE',  ( 125.9001214775786224, -4.089484607189486809, -7.948022111789456723 ) ) ;
#29177 = DIRECTION ( 'NONE',  ( 1.387778780781445676E-17, -0.9284778069183720062, -0.3713878862591650232 ) ) ;
#29178 = CARTESIAN_POINT ( 'NONE',  ( 124.3117748109119844, 0.1319031606808879209, -14.10382304977623669 ) ) ;
#29179 = EDGE_LOOP ( 'NONE', ( #1620, #31918, #6982, #1683 ) ) ;
#29180 = AXIS2_PLACEMENT_3D ( 'NONE', #30454, #30683, #34313 ) ;
#29181 = CARTESIAN_POINT ( 'NONE',  ( 116.8805814775786445, -6.344957434206662583, -7.627207830600332805 ) ) ;
#29182 = CARTESIAN_POINT ( 'NONE',  ( 121.9470836909669913, -24.14644159042263993, -12.62951656296512937 ) ) ;
#29183 = AXIS2_PLACEMENT_3D ( 'NONE', #43681, #22929, #36822 ) ;
#29184 = CARTESIAN_POINT ( 'NONE',  ( 111.6617281442453162, 0.4262465694468551280, -12.03445270309932269 ) ) ;
#29185 = CARTESIAN_POINT ( 'NONE',  ( 137.1399781293984290, -5.107918420449511387, -8.041068576975341387 ) ) ;
#29186 = CARTESIAN_POINT ( 'NONE',  ( 113.4769814775786330, 0.4262465694468514643, -12.03445270309931736 ) ) ;
#29187 = EDGE_CURVE ( 'NONE', #16480, #18690, #2947, .T. ) ;
#29188 = FACE_OUTER_BOUND ( 'NONE', #16113, .T. ) ;
#29189 = CARTESIAN_POINT ( 'NONE',  ( 125.3275354501026158, -3.173127855840466971, -20.30256202504349261 ) ) ;
#29190 = CARTESIAN_POINT ( 'NONE',  ( 112.9664414775786412, -9.859900752359374465, -12.68260735090039404 ) ) ;
#29191 = CARTESIAN_POINT ( 'NONE',  ( 112.3424481442453384, -6.344957434206662583, -7.627207830600332805 ) ) ;
#29192 = CARTESIAN_POINT ( 'NONE',  ( 120.5074391859119913, -1.406689858478933353, -17.56299727309130887 ) ) ;
#29193 = CARTESIAN_POINT ( 'NONE',  ( 124.3117748109119844, 0.1319031606808879209, -14.10382304977623669 ) ) ;
#29194 = LINE ( 'NONE', #33040, #44422 ) ;
#29195 = CARTESIAN_POINT ( 'NONE',  ( 118.2420214775786320, -3.383040157471821630, -19.15922257007629170 ) ) ;
#29196 = EDGE_CURVE ( 'NONE', #36673, #25696, #15177, .T. ) ;
#29197 = VERTEX_POINT ( 'NONE', #45051 ) ;
#29198 = CARTESIAN_POINT ( 'NONE',  ( 126.6211808763750213, -8.526882813983885256, -17.08637904477736669 ) ) ;
#29199 = EDGE_CURVE ( 'NONE', #19714, #28588, #25899, .T. ) ;
#29200 = CARTESIAN_POINT ( 'NONE',  ( 114.7192077545248594, -7.250697342233347165, -7.631215200338321125 ) ) ;
#29201 = CARTESIAN_POINT ( 'NONE',  ( 111.8021765045248372, -2.791137627527939813, -8.388885654883777576 ) ) ;
#29202 = CARTESIAN_POINT ( 'NONE',  ( 111.1076452545248259, -9.868328341294098749, -15.46607636864997204 ) ) ;
#29203 = VECTOR ( 'NONE', #15697, 1000.000000000000000 ) ;
#29204 = CARTESIAN_POINT ( 'NONE',  ( 125.7194014775786286, -9.814174330883794539, -12.68911139247586739 ) ) ;
#29205 = CARTESIAN_POINT ( 'NONE',  ( 114.6682414775786469, -1.561330072975668060, -17.79121239304076596 ) ) ;
#29206 = VERTEX_POINT ( 'NONE', #35198 ) ;
#29207 = CARTESIAN_POINT ( 'NONE',  ( 116.9373081442452929, -1.833838273342659253, -17.42832698103878286 ) ) ;
#29208 = CARTESIAN_POINT ( 'NONE',  ( 108.1906140045248463, -10.62599879583958717, -11.00651665394454604 ) ) ;
#29209 = LINE ( 'NONE', #43118, #35776 ) ;
#29210 = CARTESIAN_POINT ( 'NONE',  ( 125.9568481442452850, -6.344957434206665248, -7.627207830600338134 ) ) ;
#29211 = DIRECTION ( 'NONE',  ( -1.000000000000000000, 0.000000000000000000, 0.000000000000000000 ) ) ;
#29212 = CARTESIAN_POINT ( 'NONE',  ( 112.1722681442453222, -0.4660016031367893996, -10.09054647747474043 ) ) ;
#29213 = CARTESIAN_POINT ( 'NONE',  ( 114.3846081442453197, -10.63000616557722466, -14.87417383870573495 ) ) ;
#29214 = CARTESIAN_POINT ( 'NONE',  ( 111.4549108795247747, -8.938348069036489818, -9.318865927141430916 ) ) ;
#29215 = CARTESIAN_POINT ( 'NONE',  ( 112.6356140045247827, 0.1403307496149616695, -15.46607636864997204 ) ) ;
#29216 = VERTEX_POINT ( 'NONE', #4202 ) ;
#29217 = CARTESIAN_POINT ( 'NONE',  ( 124.6713397424434078, -0.9924539043446091169, -17.29976612834908423 ) ) ;
#29218 = AXIS2_PLACEMENT_3D ( 'NONE', #10283, #16281, #41961 ) ;
#29219 = CARTESIAN_POINT ( 'NONE',  ( 119.0929214775786278, -4.153390946401325223, -8.397313243818185668 ) ) ;
#29220 = CARTESIAN_POINT ( 'NONE',  ( 116.1998614775786507, -10.63000616557722466, -14.87417383870573495 ) ) ;
#29221 = CARTESIAN_POINT ( 'NONE',  ( 112.1722681442453222, -0.4660016031367893996, -10.09054647747474043 ) ) ;
#29222 = AXIS2_PLACEMENT_3D ( 'NONE', #21439, #32585, #35322 ) ;
#29223 = EDGE_CURVE ( 'NONE', #38146, #16801, #31793, .T. ) ;
#29224 = CARTESIAN_POINT ( 'NONE',  ( 117.8659193777725278, -1.267766418764730840, -16.93314635290706605 ) ) ;
#29225 = CARTESIAN_POINT ( 'NONE',  ( 123.0637881442452937, -8.899110576539710493, -16.42337572283490132 ) ) ;
#29226 = CARTESIAN_POINT ( 'NONE',  ( 114.8384214775786489, -10.15424416112533912, -14.75197769757731336 ) ) ;
#29227 = ORIENTED_EDGE ( 'NONE', *, *, #16988, .T. ) ;
#29228 = ADVANCED_FACE ( 'NONE', ( #118 ), #38857, .F. ) ;
#29229 = EDGE_CURVE ( 'NONE', #9699, #42672, #10962, .T. ) ;
#29230 = CARTESIAN_POINT ( 'NONE',  ( 122.7299391859119737, -1.406689858478933353, -17.56299727309130887 ) ) ;
#29231 = CARTESIAN_POINT ( 'NONE',  ( 121.9100498793805230, -2.191907684172563986, -18.20049396185734025 ) ) ;
#29232 = CARTESIAN_POINT ( 'NONE',  ( 119.0361948109119652, -2.084020599724406786, -8.691656652584148546 ) ) ;
#29233 = EDGE_LOOP ( 'NONE', ( #39093, #1677, #45012, #34517, #33454, #20048 ) ) ;
#29234 = CARTESIAN_POINT ( 'NONE',  ( 126.9932531981142745, -9.712336270502818891, -15.74219525057805846 ) ) ;
#29235 = CARTESIAN_POINT ( 'NONE',  ( 114.2711548109119803, -9.988377603198976828, -10.36322818467138340 ) ) ;
#29236 = CARTESIAN_POINT ( 'NONE',  ( 106.0375671295248310, 0.1403307496149613920, -13.39321520033831447 ) ) ;
#29237 = CARTESIAN_POINT ( 'NONE',  ( 118.9183259692789676, -1.179503403430467667, -17.05068175419387089 ) ) ;
#29238 = ORIENTED_EDGE ( 'NONE', *, *, #27263, .F. ) ;
#29239 = ORIENTED_EDGE ( 'NONE', *, *, #45138, .T. ) ;
#29240 = VECTOR ( 'NONE', #44124, 1000.000000000000000 ) ;
#29241 = CARTESIAN_POINT ( 'NONE',  ( 122.2128881442453263, -7.643976991954077427, -18.09477374809248928 ) ) ;
#29242 = CARTESIAN_POINT ( 'NONE',  ( 117.7882081442453170, -3.505236298600246325, -18.68346056562440793 ) ) ;
#29243 = LINE ( 'NONE', #19426, #7600 ) ;
#29244 = CARTESIAN_POINT ( 'NONE',  ( 116.1431348109119881, 0.1319031606808870605, -14.10382304977625090 ) ) ;
#29245 = ORIENTED_EDGE ( 'NONE', *, *, #16356, .F. ) ;
#29246 = LINE ( 'NONE', #39953, #16481 ) ;
#29247 = LINE ( 'NONE', #15338, #20841 ) ;
#29248 = CARTESIAN_POINT ( 'NONE',  ( 111.7327233795247849, -8.938348069036489818, -17.46756447353520159 ) ) ;
#29249 = CONICAL_SURFACE ( 'NONE', #5938, 2.445500000000004448, 0.9599310885968757034 ) ;
#29250 = CARTESIAN_POINT ( 'NONE',  ( 117.2776681442452968, -5.638512984488999180, -18.83840828888717311 ) ) ;
#29252 = CARTESIAN_POINT ( 'NONE',  ( 116.5402214775786405, -9.565557343593413364, -10.61323700422348004 ) ) ;
#29251 = CARTESIAN_POINT ( 'NONE',  ( 126.0135748109119902, -1.833838273342660141, -17.42832698103878286 ) ) ;
#29253 = CARTESIAN_POINT ( 'NONE',  ( 123.0070614775786169, -10.15424416112533912, -14.75197769757731336 ) ) ;
#29254 = CARTESIAN_POINT ( 'NONE',  ( 70.19189222814998175, -64.81574766768041229, -39.12908228425553858 ) ) ;
#29255 = VERTEX_POINT ( 'NONE', #38189 ) ;
#29256 = CARTESIAN_POINT ( 'NONE',  ( 118.5256548109119876, -8.899110576539710493, -16.42337572283490132 ) ) ;
#29257 = CARTESIAN_POINT ( 'NONE',  ( 125.3895814775786448, -2.084020599724406786, -8.691656652584148546 ) ) ;
#29258 = CARTESIAN_POINT ( 'NONE',  ( 112.7050671295247923, -10.62599879583958540, -13.39321520033831447 ) ) ;
#29259 = CARTESIAN_POINT ( 'NONE',  ( 116.1777233795247781, -1.325403438956436419, -9.854619843455211026 ) ) ;
#29260 = CARTESIAN_POINT ( 'NONE',  ( 113.5385046295247804, -4.863998795839590272, -7.631215200338315796 ) ) ;
#29261 = CARTESIAN_POINT ( 'NONE',  ( 117.5045748109119756, 0.5811942927096110934, -14.16772938898807510 ) ) ;
#29262 = ORIENTED_EDGE ( 'NONE', *, *, #11406, .F. ) ;
#29263 = CARTESIAN_POINT ( 'NONE',  ( 119.7169148109119874, -9.988377603198976828, -10.36322818467138340 ) ) ;
#29264 = CARTESIAN_POINT ( 'NONE',  ( 115.2188909814547344, -2.395992375830784837, -17.92872468182854107 ) ) ;
#29265 = CARTESIAN_POINT ( 'NONE',  ( 105.8986608795248401, -8.938348069036489818, -9.318865927141430916 ) ) ;
#29266 = CARTESIAN_POINT ( 'NONE',  ( 117.6180281442453150, -0.4660016031367893996, -10.09054647747474043 ) ) ;
#29267 = CARTESIAN_POINT ( 'NONE',  ( 118.9794681442453026, -9.261995988541697145, -16.69588392320189030 ) ) ;
#29268 = CARTESIAN_POINT ( 'NONE',  ( 62.37505303770993237, -3.555642511118201288, -19.24368838960830885 ) ) ;
#29269 = CARTESIAN_POINT ( 'NONE',  ( 117.0080256338066960, -11.48975918537441210, -5.808803638225159993 ) ) ;
#29270 = ORIENTED_EDGE ( 'NONE', *, *, #31744, .T. ) ;
#29271 = CARTESIAN_POINT ( 'NONE',  ( 67.30914723170953096, -52.30871106904351819, -35.02081913341498165 ) ) ;
#29272 = CARTESIAN_POINT ( 'NONE',  ( 109.2292177412187755, -9.286740210711322163, -9.723229054767012158 ) ) ;
#29273 = CARTESIAN_POINT ( 'NONE',  ( 121.9859814775786333, -9.565557343593413364, -10.61323700422348004 ) ) ;
#29274 = CARTESIAN_POINT ( 'NONE',  ( 111.4549108795247747, -1.325403438956436419, -16.93181055722141792 ) ) ;
#29275 = CARTESIAN_POINT ( 'NONE',  ( 107.2182702545248105, -10.62599879583958717, -15.77991374673208469 ) ) ;
#29276 = CARTESIAN_POINT ( 'NONE',  ( 113.3068014775786594, -1.833838273342658809, -17.42832698103878286 ) ) ;
#29277 = CARTESIAN_POINT ( 'NONE',  ( 70.19189222814998175, -65.04786711941002864, -39.22192925581980916 ) ) ;
#29278 = CARTESIAN_POINT ( 'NONE',  ( 113.7038881442453402, -6.222761293078241884, -8.102969835052219238 ) ) ;
#29279 = CARTESIAN_POINT ( 'NONE',  ( 120.1707281442453166, 0.2603800115204892296, -16.42320221600525088 ) ) ;
#29280 = EDGE_LOOP ( 'NONE', ( #27191, #32274, #37473, #12838 ) ) ;
#29281 = EDGE_CURVE ( 'NONE', #1972, #40326, #36428, .T. ) ;
#29282 = CARTESIAN_POINT ( 'NONE',  ( 118.2987481442453088, -7.894159318335828068, -9.358103419637847864 ) ) ;
#29283 = CIRCLE ( 'NONE', #11806, 4.999999999999999112 ) ;
#29284 = CARTESIAN_POINT ( 'NONE',  ( 116.9373081442452929, -8.166667518702817929, -8.995218007635861213 ) ) ;
#29285 = CARTESIAN_POINT ( 'NONE',  ( 122.9503348109119827, 0.5811942927096110934, -14.16772938898807510 ) ) ;
#29286 = CARTESIAN_POINT ( 'NONE',  ( 120.8514481442452961, -2.084020599724406786, -8.691656652584148546 ) ) ;
#29287 = ORIENTED_EDGE ( 'NONE', *, *, #2498, .F. ) ;
#29288 = EDGE_CURVE ( 'NONE', #34097, #15244, #16805, .T. ) ;
#29289 = CARTESIAN_POINT ( 'NONE',  ( 123.8012348109119642, -9.565557343593413364, -10.61323700422348004 ) ) ;
#29290 = CARTESIAN_POINT ( 'NONE',  ( 120.5678148109119832, -8.166667518702819706, -8.995218007635861213 ) ) ;
#29291 = CARTESIAN_POINT ( 'NONE',  ( 125.3566265649632072, -6.703367565947885964, -6.589706821340800325 ) ) ;
#29292 = CARTESIAN_POINT ( 'NONE',  ( 121.8158014775786171, -5.638512984488999180, -18.83840828888717311 ) ) ;
#29293 = CARTESIAN_POINT ( 'NONE',  ( 69.87572422742091760, -11.86958442233774313, -21.89321520033831447 ) ) ;
#29294 = AXIS2_PLACEMENT_3D ( 'NONE', #12127, #32848, #26486 ) ;
#29295 = CARTESIAN_POINT ( 'NONE',  ( 127.9412782985066599, -3.042519830159750249, -14.56988733893606991 ) ) ;
#29296 = CARTESIAN_POINT ( 'NONE',  ( 114.3024890045248156, -9.868328341294098749, -11.32035403202665869 ) ) ;
#29297 = AXIS2_PLACEMENT_3D ( 'NONE', #7781, #7547, #18497 ) ;
#29298 = CARTESIAN_POINT ( 'NONE',  ( 71.02242295334774269, -53.40349916253254747, -37.66903031182329897 ) ) ;
#29299 = CARTESIAN_POINT ( 'NONE',  ( 136.8192643132353510, -10.07312979839473499, -11.38871621322195971 ) ) ;
#29300 = CARTESIAN_POINT ( 'NONE',  ( 114.5547881442453217, -4.153390946401321671, -8.397313243818183892 ) ) ;
#29301 = CARTESIAN_POINT ( 'NONE',  ( 124.0281414775786146, -1.834011780172310813, -8.268836392978581529 ) ) ;
#29302 = CARTESIAN_POINT ( 'NONE',  ( 70.19189222814998175, -53.90613343638955968, -34.76527462071035046 ) ) ;
#29303 = LINE ( 'NONE', #12894, #30210 ) ;
#29304 = CARTESIAN_POINT ( 'NONE',  ( 111.0381921295247878, -9.868328341294093420, -13.39321520033831447 ) ) ;
#29305 = CARTESIAN_POINT ( 'NONE',  ( 114.8951481442453115, -8.899110576539710493, -16.42337572283490132 ) ) ;
#29306 = DIRECTION ( 'NONE',  ( 0.000000000000000000, -0.3818493186865936084, 0.9242245927363024194 ) ) ;
#29307 = AXIS2_PLACEMENT_3D ( 'NONE', #35035, #17308, #34163 ) ;
#29308 = DIRECTION ( 'NONE',  ( 0.000000000000000000, -0.3818493186865936084, 0.9242245927363024194 ) ) ;
#29310 = CARTESIAN_POINT ( 'NONE',  ( 120.0005481442453146, -5.638512984488999180, -18.83840828888717311 ) ) ;
#29309 = CARTESIAN_POINT ( 'NONE',  ( 62.89927913424436667, -13.37923420970709643, -8.047269637219322647 ) ) ;
#29311 = CARTESIAN_POINT ( 'NONE',  ( 121.7023481442452919, -0.8288870151387760510, -10.36305467784173118 ) ) ;
#29312 = EDGE_LOOP ( 'NONE', ( #8682, #2537, #3856, #8699, #6920, #27349 ) ) ;
#29313 = CARTESIAN_POINT ( 'NONE',  ( 137.5098831408921001, -7.763005863679194540, -9.317918806168908219 ) ) ;
#29314 = CARTESIAN_POINT ( 'NONE',  ( 66.82415148905926117, -40.21211973637273474, -19.39321520033831447 ) ) ;
#29315 = CARTESIAN_POINT ( 'NONE',  ( 110.8298327545248299, -6.936859964151250502, -8.388885654883777576 ) ) ;
#29316 = CARTESIAN_POINT ( 'NONE',  ( 117.9583881442453048, 0.1319031606808879209, -14.10382304977623669 ) ) ;
#29317 = EDGE_CURVE ( 'NONE', #20392, #18302, #4836, .T. ) ;
#29318 = CARTESIAN_POINT ( 'NONE',  ( 120.2841814775786276, -10.15424416112533912, -14.75197769757731336 ) ) ;
#29319 = CARTESIAN_POINT ( 'NONE',  ( 117.6180281442453150, -8.899110576539710493, -16.42337572283490132 ) ) ;
#29320 = DIRECTION ( 'NONE',  ( 0.000000000000000000, 0.6004852223388327248, -0.7996358532186277346 ) ) ;
#29321 = CARTESIAN_POINT ( 'NONE',  ( 110.5520202545248054, -10.62599879583958717, -15.77991374673208469 ) ) ;
#29322 = CARTESIAN_POINT ( 'NONE',  ( 125.1059481442452750, -1.833838273342660141, -17.42832698103878286 ) ) ;
#29323 = CARTESIAN_POINT ( 'NONE',  ( 123.0637881442452937, -8.899110576539710493, -16.42337572283490132 ) ) ;
#29324 = CARTESIAN_POINT ( 'NONE',  ( 3.060777270043529619, -5.064559853354640317, -8.893215200338314474 ) ) ;
#29325 = CARTESIAN_POINT ( 'NONE',  ( 112.6828081442453140, -2.084020599724394796, -8.691656652584146769 ) ) ;
#29326 = CARTESIAN_POINT ( 'NONE',  ( 120.9936110609119737, -6.340755971794695078, -8.611740276972781771 ) ) ;
#29327 = CARTESIAN_POINT ( 'NONE',  ( 115.8304577545247582, -7.250697342233347165, -7.631215200338321125 ) ) ;
#29328 = DIRECTION ( 'NONE',  ( 0.000000000000000000, 0.9284778069183720062, 0.3713878862591650232 ) ) ;
#29329 = CARTESIAN_POINT ( 'NONE',  ( 117.2294421295247844, 0.2335149919452661482, -21.89321520033831447 ) ) ;
#29330 = CARTESIAN_POINT ( 'NONE',  ( 121.7590748109119687, -7.893985811506177619, -18.51759400769804742 ) ) ;
#29331 = CARTESIAN_POINT ( 'NONE',  ( 117.8449348109119938, -8.166667518702817929, -8.995218007635861213 ) ) ;
#29332 = CARTESIAN_POINT ( 'NONE',  ( 106.3848327545248651, -2.477300249445798297, -19.15521520033831138 ) ) ;
#29333 = CARTESIAN_POINT ( 'NONE',  ( 117.2776681442452968, -5.638512984488999180, -18.83840828888717311 ) ) ;
#29334 = LINE ( 'NONE', #19301, #30119 ) ;
#29335 = EDGE_LOOP ( 'NONE', ( #21405, #312, #27981, #33197 ) ) ;
#29336 = CARTESIAN_POINT ( 'NONE',  ( 112.1997457829843938, 0.6362173239733635022, -14.64321520033831447 ) ) ;
#29337 = CIRCLE ( 'NONE', #24935, 5.999999999999997335 ) ;
#29338 = AXIS2_PLACEMENT_3D ( 'NONE', #23619, #27712, #19963 ) ;
#29339 = CARTESIAN_POINT ( 'NONE',  ( 119.6601881442453106, -8.166667518702819706, -8.995218007635861213 ) ) ;
#29340 = EDGE_CURVE ( 'NONE', #24500, #30574, #25192, .T. ) ;
#29341 = CARTESIAN_POINT ( 'NONE',  ( 112.2857214775786474, -4.089484607189486809, -7.948022111789456723 ) ) ;
#29342 = CARTESIAN_POINT ( 'NONE',  ( 114.0442481442453300, -7.643976991954077427, -18.09477374809248928 ) ) ;
#29343 = CARTESIAN_POINT ( 'NONE',  ( 111.5482748109120053, -0.1624402480850797581, -16.17319339645315424 ) ) ;
#29344 =( GEOMETRIC_REPRESENTATION_CONTEXT ( 3 ) GLOBAL_UNCERTAINTY_ASSIGNED_CONTEXT ( ( #6911 ) ) GLOBAL_UNIT_ASSIGNED_CONTEXT ( ( #38688, #45107, #35024 ) ) REPRESENTATION_CONTEXT ( 'NONE', 'WORKASPACE' ) );
#29345 = CARTESIAN_POINT ( 'NONE',  ( 108.1906140045248463, -10.62599879583958717, -11.00651665394454604 ) ) ;
#29346 = CARTESIAN_POINT ( 'NONE',  ( 121.6456214775786293, 0.4262465694468514643, -12.03445270309931736 ) ) ;
#29347 = CARTESIAN_POINT ( 'NONE',  ( 110.4131140045248145, -10.62599879583958540, -11.00651665394454071 ) ) ;
#29348 = CARTESIAN_POINT ( 'NONE',  ( 124.3344342554890716, -2.372251574601201174, -17.96033910819751611 ) ) ;
#29349 = ORIENTED_EDGE ( 'NONE', *, *, #14051, .F. ) ;
#29350 = CARTESIAN_POINT ( 'NONE',  ( 122.7993923109119692, -9.959231468620755479, -10.70263013195267199 ) ) ;
#29351 = CARTESIAN_POINT ( 'NONE',  ( 121.7023481442452777, -9.261995988541697145, -16.69588392320189030 ) ) ;
#29352 = EDGE_LOOP ( 'NONE', ( #12314, #36361, #8282, #21775, #35303, #1732 ) ) ;
#29353 = CARTESIAN_POINT ( 'NONE',  ( 111.2647102085435193, -8.897589485953298905, -16.42540022429002633 ) ) ;
#29354 = DIRECTION ( 'NONE',  ( 1.000000000000000000, 0.000000000000000000, 0.000000000000000000 ) ) ;
#29355 = CARTESIAN_POINT ( 'NONE',  ( 119.0361948109119652, -2.084020599724406786, -8.691656652584148546 ) ) ;
#29356 = LINE ( 'NONE', #43271, #36787 ) ;
#29357 = CARTESIAN_POINT ( 'NONE',  ( 124.5338130785779072, -9.828743235481264051, -12.79707124658312090 ) ) ;
#29358 =( BOUNDED_CURVE ( )  B_SPLINE_CURVE ( 2, ( #23393, #33857, #44826, #37279, #34090, #16787, #20429, #13584, #16559, #27494, #4198, #38853, #24957, #39313, #773, #21761, #28163 ),
 .UNSPECIFIED., .F., .F. ) 
 B_SPLINE_CURVE_WITH_KNOTS ( ( 3, 2, 2, 2, 2, 2, 2, 2, 3 ),
 ( 0.3920046674808919662, 0.3984375000000000000, 0.4062500000000000000, 0.4140625000000000000, 0.4218750000000000000, 0.4296875000000000000, 0.4375000000000000000, 0.4453125000000000000, 0.4517453325190590174 ),
 .UNSPECIFIED. ) 
 CURVE ( )  GEOMETRIC_REPRESENTATION_ITEM ( )  RATIONAL_B_SPLINE_CURVE ( ( 0.9778625265006459788, 0.9373222120152210346, 1.000000000000000000, 0.9238795325112869605, 1.000000000000000000, 0.9238795325112869605, 1.000000000000000000, 0.9238795325112869605, 1.000000000000000000, 0.9238795325112869605, 1.000000000000000000, 0.9238795325112869605, 1.000000000000000000, 0.9238795325112869605, 1.000000000000000000, 0.9373222120157019832, 0.9778625265000240319 ) ) 
 REPRESENTATION_ITEM ( '' )  );
#29359 = CARTESIAN_POINT ( 'NONE',  ( 124.8790414775786246, -8.899110576539710493, -16.42337572283490132 ) ) ;
#29360 = CARTESIAN_POINT ( 'NONE',  ( 121.0630641859119976, -0.8832429491016020595, -18.19431474523658565 ) ) ;
#29361 = VECTOR ( 'NONE', #12214, 1000.000000000000000 ) ;
#29362 = CARTESIAN_POINT ( 'NONE',  ( 124.6521348109119884, -7.894159318335828068, -9.358103419637847864 ) ) ;
#29363 = AXIS2_PLACEMENT_3D ( 'NONE', #42803, #15202, #42353 ) ;
#29364 = DIRECTION ( 'NONE',  ( 0.000000000000000000, -0.3818493186865927203, 0.9242245927363029745 ) ) ;
#29365 = CARTESIAN_POINT ( 'NONE',  ( 115.9729548109119861, -3.505236298600246325, -18.68346056562440793 ) ) ;
#29366 = CARTESIAN_POINT ( 'NONE',  ( 123.2339681442453241, -3.505236298600246325, -18.68346056562440793 ) ) ;
#29367 = CARTESIAN_POINT ( 'NONE',  ( 119.0929214775786278, -5.638512984488999180, -18.83840828888717311 ) ) ;
#29368 = CARTESIAN_POINT ( 'NONE',  ( 115.9162281442453235, -4.089484607189486809, -7.948022111789456723 ) ) ;
#29369 = CARTESIAN_POINT ( 'NONE',  ( 113.1912390045248031, -9.868328341294098749, -11.32035403202665869 ) ) ;
#29370 = CARTESIAN_POINT ( 'NONE',  ( 125.2761281442453054, 0.4262465694468514643, -12.03445270309931736 ) ) ;
#29371 = ORIENTED_EDGE ( 'NONE', *, *, #7588, .T. ) ;
#29372 = CARTESIAN_POINT ( 'NONE',  ( 120.2841814775786276, 0.9020085738987339008, -11.91225656197089222 ) ) ;
#29373 = CARTESIAN_POINT ( 'NONE',  ( 114.5803015045248117, -2.477300249445798297, -7.631215200338321125 ) ) ;
#29374 = CARTESIAN_POINT ( 'NONE',  ( 108.9545983795247821, -8.402594152722688392, -16.93181055722141792 ) ) ;
#29375 = DIRECTION ( 'NONE',  ( -1.000000000000000000, 0.000000000000000000, 0.000000000000000000 ) ) ;
#29376 = AXIS2_PLACEMENT_3D ( 'NONE', #34381, #10460, #7029 ) ;
#29377 = CARTESIAN_POINT ( 'NONE',  ( 112.2857214775786474, -5.574606645277164318, -18.38911715685844683 ) ) ;
#29378 = CARTESIAN_POINT ( 'NONE',  ( 122.1048610609119720, -6.340755971794695078, -8.611740276972781771 ) ) ;
#29379 = CARTESIAN_POINT ( 'NONE',  ( 117.0806140045248185, 0.1403307496149616695, -15.46607636864997204 ) ) ;
#29380 = ORIENTED_EDGE ( 'NONE', *, *, #20892, .F. ) ;
#29381 = CARTESIAN_POINT ( 'NONE',  ( 126.2404814775786264, -0.8288870151387760510, -10.36305467784173118 ) ) ;
#29382 = CARTESIAN_POINT ( 'NONE',  ( 121.7575954359119805, -11.07370829466463569, -12.81314460846529002 ) ) ;
#29383 = CARTESIAN_POINT ( 'NONE',  ( 122.5215798109119874, -2.173413727453600508, -8.297982527556802879 ) ) ;
#29384 = DIRECTION ( 'NONE',  ( -1.000000000000000000, 0.000000000000000000, 0.000000000000000000 ) ) ;
#29385 = CARTESIAN_POINT ( 'NONE',  ( 107.2877233795247776, -1.325403438956436419, -9.854619843455211026 ) ) ;
#29386 = ORIENTED_EDGE ( 'NONE', *, *, #36785, .T. ) ;
#29387 = CARTESIAN_POINT ( 'NONE',  ( 113.9875214775786532, -0.4660016031367893996, -10.09054647747474043 ) ) ;
#29388 = CARTESIAN_POINT ( 'NONE',  ( 126.1270281442452870, -10.30919188438810075, -12.61870101168855918 ) ) ;
#29389 = CARTESIAN_POINT ( 'NONE',  ( 120.3409081442453044, -8.899110576539710493, -16.42337572283490132 ) ) ;
#29390 = EDGE_CURVE ( 'NONE', #31284, #39770, #38620, .T. ) ;
#29391 = CARTESIAN_POINT ( 'NONE',  ( 113.3068014775786594, -1.833838273342658809, -17.42832698103878286 ) ) ;
#29392 =( LENGTH_UNIT ( ) NAMED_UNIT ( * ) SI_UNIT ( .MILLI., .METRE. ) );
#29393 = CARTESIAN_POINT ( 'NONE',  ( 88.22708560785949317, -3.622631779710408395, -16.89321520033831447 ) ) ;
#29394 = CARTESIAN_POINT ( 'NONE',  ( 71.79922130029189020, -25.12209812792223929, -4.893215200338314474 ) ) ;
#29395 = CARTESIAN_POINT ( 'NONE',  ( 113.0231681442453322, 0.9020085738987339008, -11.91225656197089222 ) ) ;
#29396 = AXIS2_PLACEMENT_3D ( 'NONE', #23864, #23176, #40273 ) ;
#29397 = CARTESIAN_POINT ( 'NONE',  ( 116.8722546295247895, -4.863998795839590272, -18.39754474579285315 ) ) ;
#29398 = CARTESIAN_POINT ( 'NONE',  ( 122.3830681442452857, -8.166667518702819706, -8.995218007635861213 ) ) ;
#29399 = CARTESIAN_POINT ( 'NONE',  ( 136.1673833308560972, -10.30576297294811461, -15.60264770220974029 ) ) ;
#29400 = EDGE_LOOP ( 'NONE', ( #4624, #2096, #34320, #4609, #21461 ) ) ;
#29401 = CARTESIAN_POINT ( 'NONE',  ( 115.1220548109119761, -8.166667518702817929, -8.995218007635861213 ) ) ;
#29402 = CARTESIAN_POINT ( 'NONE',  ( 125.2194014775786286, -10.30919188438810075, -12.61870101168855918 ) ) ;
#29403 = CARTESIAN_POINT ( 'NONE',  ( 110.7603796295247918, -4.863998795839638234, -8.388885654883775800 ) ) ;
#29404 = CARTESIAN_POINT ( 'NONE',  ( 124.5386814775786206, -4.153390946401325223, -8.397313243818185668 ) ) ;
#29405 = AXIS2_PLACEMENT_3D ( 'NONE', #35170, #41829, #7597 ) ;
#29406 = VERTEX_POINT ( 'NONE', #35658 ) ;
#29407 = CARTESIAN_POINT ( 'NONE',  ( 116.5402214775786405, 0.2603800115204892296, -16.42320221600525088 ) ) ;
#29408 = CARTESIAN_POINT ( 'NONE',  ( 125.4584548109119737, -4.863998795839242995, -13.39321520033831447 ) ) ;
#29409 = CARTESIAN_POINT ( 'NONE',  ( 125.4584548109119737, -2.316996251443989241, -21.63995271010855248 ) ) ;
#29410 = CARTESIAN_POINT ( 'NONE',  ( 111.7184548109119788, -0.8288870151387708329, -10.36305467784173828 ) ) ;
#29411 = DIRECTION ( 'NONE',  ( 0.000000000000000000, 0.4669533266896288004, 0.8842819633428518067 ) ) ;
#29412 = CARTESIAN_POINT ( 'NONE',  ( 116.0296814775786345, -1.833838273342658809, -17.42832698103878286 ) ) ;
#29413 = CARTESIAN_POINT ( 'NONE',  ( 114.3339130180080758, 0.7607806665038616689, -14.64321520033833579 ) ) ;
#29414 = DIRECTION ( 'NONE',  ( 0.9609149988134843001, -0.1028163501681632064, 0.2570431154366505933 ) ) ;
#29415 = CARTESIAN_POINT ( 'NONE',  ( 113.7606148109119886, -7.894159318335828068, -9.358103419637847864 ) ) ;
#29416 = CARTESIAN_POINT ( 'NONE',  ( 126.4673881442452910, -7.894159318335828068, -9.358103419637847864 ) ) ;
#29417 = CARTESIAN_POINT ( 'NONE',  ( 116.6331291116711526, -9.576227594267002985, -15.17824202297639857 ) ) ;
#29418 = CARTESIAN_POINT ( 'NONE',  ( 125.3328548109119964, -0.8288870151387760510, -10.36305467784173118 ) ) ;
#29419 = DIRECTION ( 'NONE',  ( 0.000000000000000000, 0.000000000000000000, 1.000000000000000000 ) ) ;
#29420 = CARTESIAN_POINT ( 'NONE',  ( 119.9438214775786378, -7.893985811506177619, -18.51759400769804742 ) ) ;
#29421 = CARTESIAN_POINT ( 'NONE',  ( 120.2841814775786276, 0.9020085738987339008, -11.91225656197089222 ) ) ;
#29422 = VERTEX_POINT ( 'NONE', #18347 ) ;
#29423 = CARTESIAN_POINT ( 'NONE',  ( 117.7088220330015389, -1.172797794773247304, -17.05961127468924587 ) ) ;
#29424 = CARTESIAN_POINT ( 'NONE',  ( 114.2330358795247776, -0.7896495226426338832, -17.46756447353520159 ) ) ;
#29425 = CARTESIAN_POINT ( 'NONE',  ( 108.6767858795247861, -8.402594152722688392, -9.854619843455216355 ) ) ;
#29426 = CARTESIAN_POINT ( 'NONE',  ( 108.2600671295247992, 0.1403307496149613920, -13.39321520033831447 ) ) ;
#29427 = CARTESIAN_POINT ( 'NONE',  ( 125.7761281442453196, -10.10582367741896093, -14.73954123521881066 ) ) ;
#29428 = CARTESIAN_POINT ( 'NONE',  ( 115.9162281442453235, -4.089484607189486809, -7.948022111789456723 ) ) ;
#29429 = ORIENTED_EDGE ( 'NONE', *, *, #10799, .T. ) ;
#29430 = CARTESIAN_POINT ( 'NONE',  ( 106.3848327545248651, -2.477300249445798297, -19.15521520033831138 ) ) ;
#29431 = CARTESIAN_POINT ( 'NONE',  ( 46.47434218039879283, -17.93412427487546523, -7.393215200338315363 ) ) ;
#29432 = DIRECTION ( 'NONE',  ( -0.000000000000000000, -0.9284778069183721172, -0.3713878862591650232 ) ) ;
#29433 = CARTESIAN_POINT ( 'NONE',  ( 112.8529881442453302, -1.561330072975668060, -17.79121239304076596 ) ) ;
#29434 = CARTESIAN_POINT ( 'NONE',  ( 120.0005481442453146, -5.638512984488999180, -18.83840828888717311 ) ) ;
#29435 = CARTESIAN_POINT ( 'NONE',  ( 112.2188952545247531, 0.8980012041604421569, -11.00651665394454071 ) ) ;
#29436 = CARTESIAN_POINT ( 'NONE',  ( 128.2184548109119930, -0.6896191363000483410, -17.70303589939592825 ) ) ;
#29437 = ORIENTED_EDGE ( 'NONE', *, *, #42324, .T. ) ;
#29438 = CARTESIAN_POINT ( 'NONE',  ( 65.10287265247758626, -0.4742552606671335269, -10.39321520033831625 ) ) ;
#29439 = CARTESIAN_POINT ( 'NONE',  ( 120.1140014775786398, -7.894159318335828068, -9.358103419637847864 ) ) ;
#29440 = CARTESIAN_POINT ( 'NONE',  ( 117.9016614775786280, -9.988377603198976828, -10.36322818467138340 ) ) ;
#29441 =( BOUNDED_SURFACE ( )  B_SPLINE_SURFACE ( 1, 2, ( 
 ( #9301, #9522, #12503, #33220, #36200, #40310, #40540, #26626, #40081, #23209, #12723, #37088, #40765, #44194, #5862, #19784, #5418, #26400, #4965, #22522, #19334, #1995, #9074, #8624, #36419, #32991, #8844, #30044, #33666, #2444, #18877, #22976, #16366, #5187, #30268, #15920, #26175, #12956, #29818, #25952, #36866, #19557, #32768, #26852, #43734, #5636, #33434, #1542, #15463, #1765, #12279, #43280, #2213, #16143, #43960, #22743, #36645, #29369, #12050, #39859, #15691, #29594, #24690, #44390, #24917, #74, #7582, #35154, #2875, #38813, #3710, #19988, #17853, #13987, #16576, #27902, #6068, #34107, #4160, #33875, #520, #21496, #35381, #20221, #28340, #21047, #41817, #18075, #31971, #297, #27057, #2644, #16806, #21272, #14655, #28124, #31302, #30470, #40977, #7136, #733, #28570, #10573, #38579, #3934, #11016, #9500, #17630, #23414, #31752, #34924, #7356, #23643, #37302, #42034, #24472, #13155, #9733, #31527, #37530, #6302, #38362, #14432, #42253, #14210, #10793, #4830, #19201, #18970, #22167, #11914, #11471, #25375, #42925, #21942, #29456, #8262, #32859, #25594, #5055, #26041, #12138, #35610, #18752, #36061, #42479, #39722, #4385, #15779, #11688, #18299, #32641, #1409, #15327, #43369, #35833, #32194, #1629, #8487, #39273, #29236 ),
 ( #39500, #43143, #25813, #14884, #28795, #8036, #15106, #36287, #39946, #8708, #11241, #22392, #22613, #4607, #36511, #15549, #32420, #5285, #33079, #967, #1851, #25149, #39044, #7816, #21723, #42701, #18528, #1193, #29015, #26497, #36953, #36733, #9385, #19878, #13040, #33529, #30140, #2767, #26266, #16237, #40173, #44055, #19642, #6426, #8938, #20110, #22841, #19419, #2535, #30365, #44287, #37180, #12821, #5498, #5724, #33306, #26719, #16005, #40628, #2081, #29682, #23761, #27173, #2307, #41094, #29913, #43593, #23295, #2992, #43827, #9853, #9616, #26939, #12594, #40405, #9165, #33766, #6191, #23069, #13267, #44504, #5953, #16461, #40863, #23536, #37421, #33996, #16691, #37651, #30583, #20336, #34219, #12366, #242, #14376, #24864, #10081, #34437, #24418, #23984, #20556, #28289, #44960, #27624, #7085, #14151, #13717, #13934, #17577, #38308, #27846, #461, #3216, #7525, #35095, #28067, #35327, #3442, #30812, #44736, #17143, #13495, #10301, #27400, #42198, #31469, #6648, #31693, #6869, #10959, #41976, #24202, #38755, #10516, #41322, #24640, #20778, #37872, #34657, #31029, #41538, #21441, #38093, #7300, #16918, #17361, #31249, #3877, #41756, #21, #20994, #34868, #3656, #10741, #38522, #21219, #17799, #8655, #22116, #11413, #14599 ) ),
 .UNSPECIFIED., .F., .F., .T. ) 
 B_SPLINE_SURFACE_WITH_KNOTS ( ( 2, 2 ),
 ( 3, 2, 2, 2, 2, 2, 2, 2, 2, 2, 2, 2, 2, 2, 2, 2, 2, 2, 2, 2, 2, 2, 2, 2, 2, 2, 2, 2, 2, 2, 2, 2, 2, 2, 2, 2, 2, 2, 2, 2, 2, 2, 2, 2, 2, 2, 2, 2, 2, 2, 2, 2, 2, 2, 2, 2, 2, 2, 2, 2, 2, 2, 2, 2, 2, 2, 2, 2, 2, 2, 2, 2, 2, 2, 2, 2, 2, 2, 2, 2, 3 ),
 ( 0.000000000000000000, 1.000000000000000000 ),
 ( 0.000000000000000000, 0.01250000000000000069, 0.02500000000000000139, 0.03749999999999999861, 0.05000000000000000278, 0.06250000000000000000, 0.07499999999999999722, 0.08749999999999999445, 0.1000000000000000056, 0.1125000000000000028, 0.1250000000000000000, 0.1375000000000000111, 0.1499999999999999944, 0.1625000000000000056, 0.1749999999999999889, 0.1875000000000000000, 0.2000000000000000111, 0.2124999999999999944, 0.2250000000000000056, 0.2374999999999999889, 0.2500000000000000000, 0.2625000000000000111, 0.2750000000000000222, 0.2874999999999999778, 0.2999999999999999889, 0.3125000000000000000, 0.3250000000000000111, 0.3375000000000000222, 0.3499999999999999778, 0.3624999999999999889, 0.3750000000000000000, 0.3875000000000000111, 0.4000000000000000222, 0.4124999999999999778, 0.4249999999999999889, 0.4375000000000000000, 0.4500000000000000111, 0.4625000000000000222, 0.4749999999999999778, 0.4874999999999999889, 0.5000000000000000000, 0.5124999999999999556, 0.5250000000000000222, 0.5374999999999999778, 0.5500000000000000444, 0.5625000000000000000, 0.5749999999999999556, 0.5875000000000000222, 0.5999999999999999778, 0.6125000000000000444, 0.6250000000000000000, 0.6374999999999999556, 0.6500000000000000222, 0.6624999999999999778, 0.6750000000000000444, 0.6875000000000000000, 0.6999999999999999556, 0.7125000000000000222, 0.7249999999999999778, 0.7375000000000000444, 0.7500000000000000000, 0.7624999999999999556, 0.7750000000000000222, 0.7874999999999999778, 0.8000000000000000444, 0.8125000000000000000, 0.8249999999999999556, 0.8375000000000000222, 0.8499999999999999778, 0.8625000000000000444, 0.8750000000000000000, 0.8874999999999999556, 0.9000000000000000222, 0.9124999999999999778, 0.9250000000000000444, 0.9375000000000000000, 0.9499999999999999556, 0.9625000000000000222, 0.9749999999999999778, 0.9875000000000000444, 1.000000000000000000 ),
 .UNSPECIFIED. ) 
 GEOMETRIC_REPRESENTATION_ITEM ( )  RATIONAL_B_SPLINE_SURFACE ( (
 ( 1.000000000000000000, 0.9238795325112869605, 1.000000000000000000, 0.9238795325112869605, 1.000000000000000000, 0.9238795325112869605, 1.000000000000000000, 0.9238795325112869605, 1.000000000000000000, 0.9238795325112869605, 1.000000000000000000, 0.9238795325112869605, 1.000000000000000000, 0.9238795325112869605, 1.000000000000000000, 0.9238795325112869605, 1.000000000000000000, 0.9238795325112869605, 1.000000000000000000, 0.9238795325112869605, 1.000000000000000000, 0.9238795325112869605, 1.000000000000000000, 0.9238795325112869605, 1.000000000000000000, 0.9238795325112869605, 1.000000000000000000, 0.9238795325112869605, 1.000000000000000000, 0.9238795325112869605, 1.000000000000000000, 0.9238795325112869605, 1.000000000000000000, 0.9238795325112869605, 1.000000000000000000, 0.9238795325112869605, 1.000000000000000000, 0.9238795325112869605, 1.000000000000000000, 0.9238795325112869605, 1.000000000000000000, 0.9238795325112869605, 1.000000000000000000, 0.9238795325112869605, 1.000000000000000000, 0.9238795325112869605, 1.000000000000000000, 0.9238795325112869605, 1.000000000000000000, 0.9238795325112869605, 1.000000000000000000, 0.9238795325112869605, 1.000000000000000000, 0.9238795325112869605, 1.000000000000000000, 0.9238795325112869605, 1.000000000000000000, 0.9238795325112869605, 1.000000000000000000, 0.9238795325112869605, 1.000000000000000000, 0.9238795325112869605, 1.000000000000000000, 0.9238795325112869605, 1.000000000000000000, 0.9238795325112869605, 1.000000000000000000, 0.9238795325112869605, 1.000000000000000000, 0.9238795325112869605, 1.000000000000000000, 0.9238795325112869605, 1.000000000000000000, 0.9238795325112869605, 1.000000000000000000, 0.9238795325112869605, 1.000000000000000000, 0.9238795325112869605, 1.000000000000000000, 0.9238795325112869605, 1.000000000000000000, 0.9238795325112869605, 1.000000000000000000, 0.9238795325112869605, 1.000000000000000000, 0.9238795325112869605, 1.000000000000000000, 0.9238795325112869605, 1.000000000000000000, 0.9238795325112869605, 1.000000000000000000, 0.9238795325112869605, 1.000000000000000000, 0.9238795325112869605, 1.000000000000000000, 0.9238795325112869605, 1.000000000000000000, 0.9238795325112869605, 1.000000000000000000, 0.9238795325112869605, 1.000000000000000000, 0.9238795325112869605, 1.000000000000000000, 0.9238795325112869605, 1.000000000000000000, 0.9238795325112869605, 1.000000000000000000, 0.9238795325112869605, 1.000000000000000000, 0.9238795325112869605, 1.000000000000000000, 0.9238795325112869605, 1.000000000000000000, 0.9238795325112869605, 1.000000000000000000, 0.9238795325112869605, 1.000000000000000000, 0.9238795325112869605, 1.000000000000000000, 0.9238795325112869605, 1.000000000000000000, 0.9238795325112869605, 1.000000000000000000, 0.9238795325112869605, 1.000000000000000000, 0.9238795325112869605, 1.000000000000000000, 0.9238795325112869605, 1.000000000000000000, 0.9238795325112869605, 1.000000000000000000, 0.9238795325112869605, 1.000000000000000000, 0.9238795325112869605, 1.000000000000000000, 0.9238795325112869605, 1.000000000000000000, 0.9238795325112869605, 1.000000000000000000, 0.9238795325112869605, 1.000000000000000000, 0.9238795325112869605, 1.000000000000000000, 0.9238795325112869605, 1.000000000000000000, 0.9238795325112869605, 1.000000000000000000, 0.9238795325112869605, 1.000000000000000000, 0.9238795325112869605, 1.000000000000000000, 0.9238795325112869605, 1.000000000000000000, 0.9238795325112869605, 1.000000000000000000, 0.9238795325112869605, 1.000000000000000000, 0.9238795325112869605, 1.000000000000000000, 0.9238795325112869605, 1.000000000000000000),
 ( 1.000000000000000000, 0.9238795325112869605, 1.000000000000000000, 0.9238795325112869605, 1.000000000000000000, 0.9238795325112869605, 1.000000000000000000, 0.9238795325112869605, 1.000000000000000000, 0.9238795325112869605, 1.000000000000000000, 0.9238795325112869605, 1.000000000000000000, 0.9238795325112869605, 1.000000000000000000, 0.9238795325112869605, 1.000000000000000000, 0.9238795325112869605, 1.000000000000000000, 0.9238795325112869605, 1.000000000000000000, 0.9238795325112869605, 1.000000000000000000, 0.9238795325112869605, 1.000000000000000000, 0.9238795325112869605, 1.000000000000000000, 0.9238795325112869605, 1.000000000000000000, 0.9238795325112869605, 1.000000000000000000, 0.9238795325112869605, 1.000000000000000000, 0.9238795325112869605, 1.000000000000000000, 0.9238795325112869605, 1.000000000000000000, 0.9238795325112869605, 1.000000000000000000, 0.9238795325112869605, 1.000000000000000000, 0.9238795325112869605, 1.000000000000000000, 0.9238795325112869605, 1.000000000000000000, 0.9238795325112869605, 1.000000000000000000, 0.9238795325112869605, 1.000000000000000000, 0.9238795325112869605, 1.000000000000000000, 0.9238795325112869605, 1.000000000000000000, 0.9238795325112869605, 1.000000000000000000, 0.9238795325112869605, 1.000000000000000000, 0.9238795325112869605, 1.000000000000000000, 0.9238795325112869605, 1.000000000000000000, 0.9238795325112869605, 1.000000000000000000, 0.9238795325112869605, 1.000000000000000000, 0.9238795325112869605, 1.000000000000000000, 0.9238795325112869605, 1.000000000000000000, 0.9238795325112869605, 1.000000000000000000, 0.9238795325112869605, 1.000000000000000000, 0.9238795325112869605, 1.000000000000000000, 0.9238795325112869605, 1.000000000000000000, 0.9238795325112869605, 1.000000000000000000, 0.9238795325112869605, 1.000000000000000000, 0.9238795325112869605, 1.000000000000000000, 0.9238795325112869605, 1.000000000000000000, 0.9238795325112869605, 1.000000000000000000, 0.9238795325112869605, 1.000000000000000000, 0.9238795325112869605, 1.000000000000000000, 0.9238795325112869605, 1.000000000000000000, 0.9238795325112869605, 1.000000000000000000, 0.9238795325112869605, 1.000000000000000000, 0.9238795325112869605, 1.000000000000000000, 0.9238795325112869605, 1.000000000000000000, 0.9238795325112869605, 1.000000000000000000, 0.9238795325112869605, 1.000000000000000000, 0.9238795325112869605, 1.000000000000000000, 0.9238795325112869605, 1.000000000000000000, 0.9238795325112869605, 1.000000000000000000, 0.9238795325112869605, 1.000000000000000000, 0.9238795325112869605, 1.000000000000000000, 0.9238795325112869605, 1.000000000000000000, 0.9238795325112869605, 1.000000000000000000, 0.9238795325112869605, 1.000000000000000000, 0.9238795325112869605, 1.000000000000000000, 0.9238795325112869605, 1.000000000000000000, 0.9238795325112869605, 1.000000000000000000, 0.9238795325112869605, 1.000000000000000000, 0.9238795325112869605, 1.000000000000000000, 0.9238795325112869605, 1.000000000000000000, 0.9238795325112869605, 1.000000000000000000, 0.9238795325112869605, 1.000000000000000000, 0.9238795325112869605, 1.000000000000000000, 0.9238795325112869605, 1.000000000000000000, 0.9238795325112869605, 1.000000000000000000, 0.9238795325112869605, 1.000000000000000000, 0.9238795325112869605, 1.000000000000000000, 0.9238795325112869605, 1.000000000000000000, 0.9238795325112869605, 1.000000000000000000, 0.9238795325112869605, 1.000000000000000000, 0.9238795325112869605, 1.000000000000000000, 0.9238795325112869605, 1.000000000000000000, 0.9238795325112869605, 1.000000000000000000, 0.9238795325112869605, 1.000000000000000000) ) ) 
 REPRESENTATION_ITEM ( '' )  SURFACE ( )  );
#29442 = DIRECTION ( 'NONE',  ( -0.9908103287288504424, 0.1352586133457951423, 0.000000000000000000 ) ) ;
#29443 = LINE ( 'NONE', #26252, #10469 ) ;
#29444 = CARTESIAN_POINT ( 'NONE',  ( 123.8012348109119642, -9.565557343593413364, -10.61323700422348004 ) ) ;
#29445 = CARTESIAN_POINT ( 'NONE',  ( 115.0653281442453277, -3.505236298600246325, -18.68346056562440793 ) ) ;
#29446 = ORIENTED_EDGE ( 'NONE', *, *, #40368, .F. ) ;
#29447 =( GEOMETRIC_REPRESENTATION_CONTEXT ( 3 ) GLOBAL_UNCERTAINTY_ASSIGNED_CONTEXT ( ( #42467 ) ) GLOBAL_UNIT_ASSIGNED_CONTEXT ( ( #25819, #16244, #33312 ) ) REPRESENTATION_CONTEXT ( 'NONE', 'WORKASPACE' ) );
#29448 = CARTESIAN_POINT ( 'NONE',  ( 123.1466579359119891, -4.360204210389833968, -8.000047426360245240 ) ) ;
#29449 = CARTESIAN_POINT ( 'NONE',  ( 63.69189222814998175, -50.16718729050181480, 3.106784799661685526 ) ) ;
#29450 = CARTESIAN_POINT ( 'NONE',  ( 118.3554748109119998, -9.565557343593413364, -10.61323700422348004 ) ) ;
#29451 = ORIENTED_EDGE ( 'NONE', *, *, #30678, .T. ) ;
#29452 = CARTESIAN_POINT ( 'NONE',  ( 110.6214888068194853, 0.1168444861213632779, -12.14321520033831625 ) ) ;
#29453 = CARTESIAN_POINT ( 'NONE',  ( 114.8951481442453115, -0.4660016031367893996, -10.09054647747474043 ) ) ;
#29454 = CIRCLE ( 'NONE', #37467, 2.999999999999999556 ) ;
#29455 = ADVANCED_FACE ( 'NONE', ( #10615 ), #32240, .T. ) ;
#29456 = CARTESIAN_POINT ( 'NONE',  ( 107.7738952545248310, -9.868328341294098749, -15.46607636864997204 ) ) ;
#29457 = CARTESIAN_POINT ( 'NONE',  ( 113.3635281442453504, -0.1624402480850797581, -16.17319339645315424 ) ) ;
#29458 = EDGE_LOOP ( 'NONE', ( #24063, #18531, #13214, #28509, #27599 ) ) ;
#29459 = VERTEX_POINT ( 'NONE', #24518 ) ;
#29460 = CARTESIAN_POINT ( 'NONE',  ( 121.1918081442452859, -10.15424416112533912, -14.75197769757731336 ) ) ;
#29461 = CARTESIAN_POINT ( 'NONE',  ( 122.5532481442453019, 0.4262465694468514643, -12.03445270309931736 ) ) ;
#29462 = CARTESIAN_POINT ( 'NONE',  ( 65.92808964132663618, -15.33417687497728643, -16.39321520033831447 ) ) ;
#29463 = EDGE_LOOP ( 'NONE', ( #29058, #16892, #26914, #36778 ) ) ;
#29464 = CARTESIAN_POINT ( 'NONE',  ( 61.69189222814998175, -49.76310523276723785, -34.89321520033831092 ) ) ;
#29465 = CARTESIAN_POINT ( 'NONE',  ( 62.15747001998436616, -65.30058926756809967, -44.86669339845351345 ) ) ;
#29466 = CARTESIAN_POINT ( 'NONE',  ( 107.1488171295247867, -10.62599879583958540, -13.39321520033831447 ) ) ;
#29467 = CARTESIAN_POINT ( 'NONE',  ( 115.1220548109119761, -8.166667518702817929, -8.995218007635861213 ) ) ;
#29468 = ADVANCED_FACE ( 'NONE', ( #7176 ), #35713, .F. ) ;
#29470 = CARTESIAN_POINT ( 'NONE',  ( 116.4267681442453153, -6.222761293078241884, -8.102969835052219238 ) ) ;
#29469 = CARTESIAN_POINT ( 'NONE',  ( 113.6471614775786492, -5.638512984488999180, -18.83840828888717311 ) ) ;
#29471 = CARTESIAN_POINT ( 'NONE',  ( 123.1205148109119563, -7.643976991954077427, -18.09477374809248928 ) ) ;
#29472 = CARTESIAN_POINT ( 'NONE',  ( 65.19189222814998175, -41.76310523276723785, -24.39321520033831447 ) ) ;
#29473 = EDGE_CURVE ( 'NONE', #26936, #42171, #753, .T. ) ;
#29474 = EDGE_CURVE ( 'NONE', #32359, #3982, #22433, .T. ) ;
#29475 = ORIENTED_EDGE ( 'NONE', *, *, #30899, .F. ) ;
#29476 = CARTESIAN_POINT ( 'NONE',  ( 121.1918081442452859, -10.15424416112533912, -14.75197769757731336 ) ) ;
#29477 = DIRECTION ( 'NONE',  ( 1.000000000000000000, 0.000000000000000000, -0.000000000000000000 ) ) ;
#29478 = AXIS2_PLACEMENT_3D ( 'NONE', #44456, #20061, #44236 ) ;
#29479 = CARTESIAN_POINT ( 'NONE',  ( 110.9687390045248350, 0.8980012041604421569, -15.77991374673208469 ) ) ;
#29480 = CARTESIAN_POINT ( 'NONE',  ( 116.3860827545247787, -6.936859964151250502, -8.388885654883777576 ) ) ;
#29481 = CARTESIAN_POINT ( 'NONE',  ( 110.3436608795247764, -8.938348069036489818, -9.318865927141430916 ) ) ;
#29482 = CARTESIAN_POINT ( 'NONE',  ( 119.6034614775786196, -6.344957434206665248, -7.627207830600338134 ) ) ;
#29483 = EDGE_LOOP ( 'NONE', ( #27380, #25366, #14466, #4465 ) ) ;
#29484 = CARTESIAN_POINT ( 'NONE',  ( 119.7736414775786358, -10.30919188438810075, -12.61870101168855918 ) ) ;
#29485 = CARTESIAN_POINT ( 'NONE',  ( 62.22678445075433018, -36.72958069525633817, -5.531797115907686191 ) ) ;
#29486 = CARTESIAN_POINT ( 'NONE',  ( 70.19189222814998175, -55.76308905022629858, -35.50805039322867884 ) ) ;
#29487 = CARTESIAN_POINT ( 'NONE',  ( 116.5969481442453031, 0.5811942927096154232, -14.16772938898807155 ) ) ;
#29488 = CARTESIAN_POINT ( 'NONE',  ( 118.8660148109119774, -10.30919188438810075, -12.61870101168855918 ) ) ;
#29490 = VECTOR ( 'NONE', #13344, 1000.000000000000114 ) ;
#29489 = CARTESIAN_POINT ( 'NONE',  ( 67.37136766119182596, -67.53150897494617766, -41.09057840265009531 ) ) ;
#29491 = CARTESIAN_POINT ( 'NONE',  ( 116.6168215951329472, -11.86651415378938879, -6.422085954748080638 ) ) ;
#29492 = ORIENTED_EDGE ( 'NONE', *, *, #7632, .T. ) ;
#29493 = FACE_OUTER_BOUND ( 'NONE', #268, .T. ) ;
#29494 = CARTESIAN_POINT ( 'NONE',  ( 109.2294501619033156, -10.07790831936271658, -11.17625042590223927 ) ) ;
#29495 = CARTESIAN_POINT ( 'NONE',  ( 120.5678148109119832, -1.833838273342659253, -17.42832698103878286 ) ) ;
#29496 = CARTESIAN_POINT ( 'NONE',  ( 110.6909265045248247, -2.791137627527939813, -8.388885654883777576 ) ) ;
#29497 = CARTESIAN_POINT ( 'NONE',  ( 106.8015515045248378, -2.477300249445798297, -7.631215200338321125 ) ) ;
#29498 = CARTESIAN_POINT ( 'NONE',  ( 113.5904348109119866, -2.084020599724406786, -8.691656652584148546 ) ) ;
#29499 = DIRECTION ( 'NONE',  ( 0.000000000000000000, -0.3818493186865936084, 0.9242245927363024194 ) ) ;
#29500 = CARTESIAN_POINT ( 'NONE',  ( 69.92918015000313403, -25.34836422082628715, -5.722398249991065278 ) ) ;
#29501 = CARTESIAN_POINT ( 'NONE',  ( 113.7606148109119886, -7.894159318335828068, -9.358103419637847864 ) ) ;
#29502 = CARTESIAN_POINT ( 'NONE',  ( 120.7947214775786193, -9.261995988541697145, -16.69588392320189030 ) ) ;
#29503 = ORIENTED_EDGE ( 'NONE', *, *, #15842, .F. ) ;
#29504 = EDGE_CURVE ( 'NONE', #44074, #9856, #24090, .T. ) ;
#29505 = CARTESIAN_POINT ( 'NONE',  ( 118.4689281442453250, -10.15424416112533912, -14.75197769757731336 ) ) ;
#29506 = CARTESIAN_POINT ( 'NONE',  ( 115.7460481442453357, 0.9020085738987339008, -11.91225656197089222 ) ) ;
#29507 = CARTESIAN_POINT ( 'NONE',  ( 123.2339681442453241, -6.344957434206665248, -7.627207830600338134 ) ) ;
#29508 = CARTESIAN_POINT ( 'NONE',  ( 120.9081748109119872, -4.153390946401325223, -8.397313243818185668 ) ) ;
#29509 = ORIENTED_EDGE ( 'NONE', *, *, #44007, .T. ) ;
#29510 = CARTESIAN_POINT ( 'NONE',  ( 116.4244054349294686, -1.040089454026965399, -17.23633227186632766 ) ) ;
#29511 = EDGE_CURVE ( 'NONE', #42460, #17168, #24122, .T. ) ;
#29512 = EDGE_CURVE ( 'NONE', #15883, #1412, #43413, .T. ) ;
#29513 = CIRCLE ( 'NONE', #36073, 0.2499999999999990841 ) ;
#29514 = CARTESIAN_POINT ( 'NONE',  ( 120.1707281442453166, 0.2603800115204892296, -16.42320221600525088 ) ) ;
#29515 = CARTESIAN_POINT ( 'NONE',  ( 124.1726284085847709, -5.853720688424037810, -5.454752289499457341 ) ) ;
#29516 = CARTESIAN_POINT ( 'NONE',  ( 122.5532481442453019, -10.63000616557722466, -14.87417383870573495 ) ) ;
#29517 = CARTESIAN_POINT ( 'NONE',  ( 107.5655358795247736, -0.7896495226426338832, -17.46756447353520159 ) ) ;
#29518 = AXIS2_PLACEMENT_3D ( 'NONE', #7576, #39494, #21718 ) ;
#29519 = CARTESIAN_POINT ( 'NONE',  ( 85.70478001548416103, -25.99489077589524300, -13.39321520033831447 ) ) ;
#29520 = CARTESIAN_POINT ( 'NONE',  ( 118.8101210407382382, -2.419733177069661512, -17.89711025544711376 ) ) ;
#29521 = CARTESIAN_POINT ( 'NONE',  ( 113.8857702545248003, 0.1403307496149616695, -11.32035403202665336 ) ) ;
#29522 = CARTESIAN_POINT ( 'NONE',  ( 79.72353890764954087, 4.236894767232761261, -14.64321520033831447 ) ) ;
#29523 = DIRECTION ( 'NONE',  ( 0.000000000000000000, 0.000000000000000000, -1.000000000000000000 ) ) ;
#29524 = CARTESIAN_POINT ( 'NONE',  ( 119.7736414775786358, 0.1319031606808879209, -14.10382304977623669 ) ) ;
#29525 = CARTESIAN_POINT ( 'NONE',  ( 124.4252281442452812, -9.261995988541697145, -16.69588392320189030 ) ) ;
#29526 = LINE ( 'NONE', #1923, #32301 ) ;
#29527 = ADVANCED_FACE ( 'NONE', ( #33345 ), #43773, .T. ) ;
#29528 = ORIENTED_EDGE ( 'NONE', *, *, #25373, .F. ) ;
#29529 = CARTESIAN_POINT ( 'NONE',  ( 116.9448827545247696, -2.792930983974093007, -18.39321520033830737 ) ) ;
#29530 = CARTESIAN_POINT ( 'NONE',  ( 112.8439733795247832, -1.325403438956436419, -9.854619843455211026 ) ) ;
#29531 = CARTESIAN_POINT ( 'NONE',  ( 117.1074881442453233, 0.4262465694468514643, -12.03445270309931736 ) ) ;
#29532 = FACE_OUTER_BOUND ( 'NONE', #19143, .T. ) ;
#29533 = CARTESIAN_POINT ( 'NONE',  ( 65.25964473381483799, -0.4011607976803650000, -10.39321520033831447 ) ) ;
#29534 = CARTESIAN_POINT ( 'NONE',  ( -2.287846945405087595, -6.971096200682639576, -19.14905881027154422 ) ) ;
#29536 = CARTESIAN_POINT ( 'NONE',  ( 122.0427081442452817, 0.5811942927096110934, -14.16772938898807510 ) ) ;
#29535 = CARTESIAN_POINT ( 'NONE',  ( 62.31172044813433075, -14.51131609691315383, -9.168783104843154064 ) ) ;
#29537 = CARTESIAN_POINT ( 'NONE',  ( 122.4965214775786251, 0.1319031606808879209, -14.10382304977623669 ) ) ;
#29538 = EDGE_LOOP ( 'NONE', ( #38820, #41090, #3438, #26105 ) ) ;
#29539 = CARTESIAN_POINT ( 'NONE',  ( 91.11246428952674137, -24.14644159042263993, -12.62951656296512937 ) ) ;
#29540 = CARTESIAN_POINT ( 'NONE',  ( 65.52069343109694444, -15.46830775796534319, -10.39321520033831625 ) ) ;
#29541 = CARTESIAN_POINT ( 'NONE',  ( 108.3295202545248657, 0.1403307496149616695, -11.32035403202665336 ) ) ;
#29542 = CARTESIAN_POINT ( 'NONE',  ( 121.3619881442452879, -5.574606645277164318, -18.38911715685844683 ) ) ;
#29543 = CARTESIAN_POINT ( 'NONE',  ( 120.6812681442452941, 0.1319031606808879209, -14.10382304977623669 ) ) ;
#29544 = CARTESIAN_POINT ( 'NONE',  ( 121.1918081442452859, -10.15424416112533912, -14.75197769757731336 ) ) ;
#29545 = CARTESIAN_POINT ( 'NONE',  ( 125.0048763211397471, 2.279351556901532128, -15.91318496429555296 ) ) ;
#29546 = CARTESIAN_POINT ( 'NONE',  ( 107.6349890045248401, 0.8980012041604421569, -15.77991374673208469 ) ) ;
#29547 = AXIS2_PLACEMENT_3D ( 'NONE', #11640, #31926, #39457 ) ;
#29548 = CARTESIAN_POINT ( 'NONE',  ( 73.60369002873177635, -5.846784287000932778, -18.64321520033831803 ) ) ;
#29549 = DIRECTION ( 'NONE',  ( -1.000000000000000000, 1.214306433183763980E-15, 0.000000000000000000 ) ) ;
#29550 = LINE ( 'NONE', #39592, #3701 ) ;
#29551 = CARTESIAN_POINT ( 'NONE',  ( 112.9828796295247884, -4.863998795839590272, -19.15521520033831493 ) ) ;
#29552 = CARTESIAN_POINT ( 'NONE',  ( 82.89134431723762475, -31.13449359622123680, -21.94632144483577818 ) ) ;
#29553 = CARTESIAN_POINT ( 'NONE',  ( 119.5467348109119712, -4.089484607189486809, -7.948022111789456723 ) ) ;
#29554 = CARTESIAN_POINT ( 'NONE',  ( 116.8238548109119819, -4.089484607189486809, -7.948022111789456723 ) ) ;
#29555 = CARTESIAN_POINT ( 'NONE',  ( 107.5655358795247736, -0.7896495226426338832, -17.46756447353520159 ) ) ;
#29556 = CARTESIAN_POINT ( 'NONE',  ( 117.1074881442453233, -10.63000616557722466, -14.87417383870573495 ) ) ;
#29557 = DIRECTION ( 'NONE',  ( 1.000000000000000000, 0.000000000000000000, -0.000000000000000000 ) ) ;
#29558 = ORIENTED_EDGE ( 'NONE', *, *, #18171, .T. ) ;
#29559 = CARTESIAN_POINT ( 'NONE',  ( 112.2879504682428831, 0.5115630086001619059, -14.64321520033830026 ) ) ;
#29560 = CIRCLE ( 'NONE', #40466, 2.445500000000004448 ) ;
#29561 = CARTESIAN_POINT ( 'NONE',  ( 122.8936081442453059, 0.2603800115204892296, -16.42320221600525088 ) ) ;
#29562 = CARTESIAN_POINT ( 'NONE',  ( 120.1707281442453166, 0.2603800115204892296, -16.42320221600525088 ) ) ;
#29563 = AXIS2_PLACEMENT_3D ( 'NONE', #28056, #18008, #7515 ) ;
#29564 = CARTESIAN_POINT ( 'NONE',  ( 126.5808414775786446, -9.859900752359378018, -12.68260735090039759 ) ) ;
#29565 = CARTESIAN_POINT ( 'NONE',  ( 112.3991748109119868, -1.833838273342658809, -17.42832698103878286 ) ) ;
#29566 = CARTESIAN_POINT ( 'NONE',  ( 112.1722681442453222, -8.899110576539710493, -16.42337572283490132 ) ) ;
#29567 = CARTESIAN_POINT ( 'NONE',  ( 110.8992858795247827, -0.7896495226426338832, -17.46756447353520159 ) ) ;
#29568 = CARTESIAN_POINT ( 'NONE',  ( 121.5888948109119809, 0.1319031606808879209, -14.10382304977623669 ) ) ;
#29569 = CARTESIAN_POINT ( 'NONE',  ( 116.7862463306490355, -3.361876234510294381, -18.36316846464617214 ) ) ;
#29570 = AXIS2_PLACEMENT_3D ( 'NONE', #14691, #17887, #28606 ) ;
#29571 = CARTESIAN_POINT ( 'NONE',  ( 124.4129961498676948, -2.324775150319219108, -18.02356106541841996 ) ) ;
#29572 = ORIENTED_EDGE ( 'NONE', *, *, #34615, .F. ) ;
#29573 = EDGE_CURVE ( 'NONE', #7942, #166, #16109, .T. ) ;
#29574 = CARTESIAN_POINT ( 'NONE',  ( 121.1325173109119788, -9.289237151508434209, -11.05642687123711276 ) ) ;
#29575 = CARTESIAN_POINT ( 'NONE',  ( 121.3619881442452879, -4.089484607189486809, -7.948022111789456723 ) ) ;
#29576 = AXIS2_PLACEMENT_3D ( 'NONE', #40996, #3348, #17267 ) ;
#29577 = CARTESIAN_POINT ( 'NONE',  ( 70.19189222814998175, -75.31442247550839397, -37.94335727672635983 ) ) ;
#29578 = FACE_OUTER_BOUND ( 'NONE', #29400, .T. ) ;
#29579 = DIRECTION ( 'NONE',  ( -0.000000000000000000, -0.9284778069183721172, -0.3713878862591650232 ) ) ;
#29580 = CARTESIAN_POINT ( 'NONE',  ( 119.3765548109119834, -10.15424416112533912, -14.75197769757731336 ) ) ;
#29581 = CARTESIAN_POINT ( 'NONE',  ( 92.32016463086877422, -25.99489077589524300, -13.39321520033831447 ) ) ;
#29582 = CARTESIAN_POINT ( 'NONE',  ( 64.01282776924008999, -34.86145050234441811, -5.893215200338315363 ) ) ;
#29583 = CARTESIAN_POINT ( 'NONE',  ( 124.5386814775786206, -4.153390946401325223, -8.397313243818185668 ) ) ;
#29584 = CARTESIAN_POINT ( 'NONE',  ( 109.6473066399283880, 0.4261359969231631739, -14.64321520033828605 ) ) ;
#29585 = CARTESIAN_POINT ( 'NONE',  ( 125.6164881442453094, -9.565557343593413364, -10.61323700422348004 ) ) ;
#29586 = CARTESIAN_POINT ( 'NONE',  ( 125.2559326335950232, -11.97226500772692681, -14.83370496690971940 ) ) ;
#29587 = CARTESIAN_POINT ( 'NONE',  ( 122.4965214775786251, -10.30919188438810075, -12.61870101168855918 ) ) ;
#29588 = CARTESIAN_POINT ( 'NONE',  ( 118.2420214775786320, -6.222761293078241884, -8.102969835052219238 ) ) ;
#29589 = CARTESIAN_POINT ( 'NONE',  ( 122.0427081442452817, -9.859900752359378018, -12.68260735090039759 ) ) ;
#29590 = ORIENTED_EDGE ( 'NONE', *, *, #44006, .F. ) ;
#29591 = CARTESIAN_POINT ( 'NONE',  ( 124.5386814775786206, -5.638512984488999180, -18.83840828888717311 ) ) ;
#29592 = EDGE_CURVE ( 'NONE', #39160, #15102, #11001, .T. ) ;
#29593 = CARTESIAN_POINT ( 'NONE',  ( 114.9518748109119883, -1.834011780172310813, -8.268836392978581529 ) ) ;
#29594 = CARTESIAN_POINT ( 'NONE',  ( 112.9134265045247645, -2.791137627527939813, -8.388885654883777576 ) ) ;
#29595 = CARTESIAN_POINT ( 'NONE',  ( 124.6521348109119884, -7.894159318335828068, -9.358103419637847864 ) ) ;
#29596 = CARTESIAN_POINT ( 'NONE',  ( 120.7947214775786193, -9.261995988541697145, -16.69588392320189030 ) ) ;
#29597 = CARTESIAN_POINT ( 'NONE',  ( 114.3024890045248156, 0.8980012041604421569, -15.77991374673208469 ) ) ;
#29598 = CARTESIAN_POINT ( 'NONE',  ( 109.8574890045248509, -9.868328341294098749, -11.32035403202665869 ) ) ;
#29599 = DIRECTION ( 'NONE',  ( 0.000000000000000000, -1.000000000000000000, 0.000000000000000000 ) ) ;
#29600 = DIRECTION ( 'NONE',  ( 0.000000000000000000, -0.9242245927363028635, -0.3818493186865930533 ) ) ;
#29601 = CARTESIAN_POINT ( 'NONE',  ( 63.69189222814998175, -50.16718729050181480, -6.893215200338315363 ) ) ;
#29602 = AXIS2_PLACEMENT_3D ( 'NONE', #23819, #6477, #40917 ) ;
#29603 = CARTESIAN_POINT ( 'NONE',  ( 124.3685014775786328, -10.63000616557722466, -14.87417383870573495 ) ) ;
#29604 = ORIENTED_EDGE ( 'NONE', *, *, #29167, .T. ) ;
#29605 = CARTESIAN_POINT ( 'NONE',  ( 124.5954081442453116, -6.222761293078241884, -8.102969835052219238 ) ) ;
#29606 = CARTESIAN_POINT ( 'NONE',  ( 120.0907204359119760, -10.25716656981731489, -12.88942061488890545 ) ) ;
#29607 = CARTESIAN_POINT ( 'NONE',  ( 122.8688454359119646, -11.07370829466463569, -12.81314460846529002 ) ) ;
#29608 = CARTESIAN_POINT ( 'NONE',  ( 123.6843602343419377, -8.309924745830986836, -17.19909913565936321 ) ) ;
#29609 = CARTESIAN_POINT ( 'NONE',  ( 108.8156921295247912, -9.868328341294093420, -13.39321520033831447 ) ) ;
#29610 = AXIS2_PLACEMENT_3D ( 'NONE', #24563, #16893, #42793 ) ;
#29611 = VERTEX_POINT ( 'NONE', #25855 ) ;
#29612 = CARTESIAN_POINT ( 'NONE',  ( 114.1009748109119784, -4.089484607189486809, -7.948022111789456723 ) ) ;
#29613 = DIRECTION ( 'NONE',  ( 0.1352586133457950590, 0.9908103287288504424, 0.000000000000000000 ) ) ;
#29614 = CARTESIAN_POINT ( 'NONE',  ( 124.6521348109119884, -7.894159318335828068, -9.358103419637847864 ) ) ;
#29615 = CARTESIAN_POINT ( 'NONE',  ( 114.8384214775786489, -10.15424416112533912, -14.75197769757731336 ) ) ;
#29616 = CARTESIAN_POINT ( 'NONE',  ( 116.1265176481213928, -2.395992375830784837, -17.92872468182854107 ) ) ;
#29617 = CARTESIAN_POINT ( 'NONE',  ( 124.0281414775786288, -1.834011780172276396, -8.268836392978611727 ) ) ;
#29618 = CARTESIAN_POINT ( 'NONE',  ( 116.1431348109119881, -10.30919188438810075, -12.61870101168855918 ) ) ;
#29619 = VECTOR ( 'NONE', #40579, 1000.000000000000000 ) ;
#29620 = CARTESIAN_POINT ( 'NONE',  ( 110.6214733795247867, -1.325403438956436419, -9.854619843455211026 ) ) ;
#29621 = CARTESIAN_POINT ( 'NONE',  ( 122.5532481442453019, -10.63000616557722466, -14.87417383870573495 ) ) ;
#29622 = CARTESIAN_POINT ( 'NONE',  ( 87.14323352029596492, -25.99489077589524300, -13.39321520033831625 ) ) ;
#29623 = VERTEX_POINT ( 'NONE', #22209 ) ;
#29624 =( BOUNDED_CURVE ( )  B_SPLINE_CURVE ( 2, ( #12945, #6082, #22965, #29360, #16357, #15681, #5177, #29809, #44184, #12269, #39850, #33656, #33425, #2432, #5626, #22734, #36409 ),
 .UNSPECIFIED., .F., .F. ) 
 B_SPLINE_CURVE_WITH_KNOTS ( ( 3, 2, 2, 2, 2, 2, 2, 2, 3 ),
 ( 0.2589135524044680059, 0.2812500000000000000, 0.3125000000000000000, 0.3437500000000000000, 0.3750000000000000000, 0.4062500000000000000, 0.4375000000000000000, 0.4687500000000000000, 0.4910864475955319941 ),
 .UNSPECIFIED. ) 
 CURVE ( )  GEOMETRIC_REPRESENTATION_ITEM ( )  RATIONAL_B_SPLINE_CURVE ( ( 0.9689618144536780164, 0.9455916533437099813, 1.000000000000000000, 0.9238795325112869605, 1.000000000000000000, 0.9238795325112869605, 1.000000000000000000, 0.9238795325112869605, 1.000000000000000000, 0.9238795325112869605, 1.000000000000000000, 0.9238795325112869605, 1.000000000000000000, 0.9238795325112869605, 1.000000000000000000, 0.9455916533437099813, 0.9689618144536780164 ) ) 
 REPRESENTATION_ITEM ( '' )  );
#29625 = CARTESIAN_POINT ( 'NONE',  ( 115.8595014775786609, -1.834011780172310813, -8.268836392978581529 ) ) ;
#29626 = CARTESIAN_POINT ( 'NONE',  ( 114.4413348109119823, -0.8288870151387760510, -10.36305467784173118 ) ) ;
#29627 = DIRECTION ( 'NONE',  ( 0.000000000000000000, 0.000000000000000000, -1.000000000000000000 ) ) ;
#29628 = CARTESIAN_POINT ( 'NONE',  ( 126.4106614775786284, -6.222761293078241884, -8.102969835052219238 ) ) ;
#29629 = ORIENTED_EDGE ( 'NONE', *, *, #20016, .T. ) ;
#29630 = CARTESIAN_POINT ( 'NONE',  ( 116.7671281442453335, -1.834011780172310813, -8.268836392978581529 ) ) ;
#29632 = DIRECTION ( 'NONE',  ( 0.000000000000000000, 0.000000000000000000, 1.000000000000000000 ) ) ;
#29631 = CIRCLE ( 'NONE', #14370, 5.635000000000000675 ) ;
#29633 = DIRECTION ( 'NONE',  ( 0.000000000000000000, 0.4669533266896288004, 0.8842819633428518067 ) ) ;
#29634 = CARTESIAN_POINT ( 'NONE',  ( 111.9453614775786434, -7.894159318335820963, -9.358103419637842535 ) ) ;
#29635 = CARTESIAN_POINT ( 'NONE',  ( 136.8611794030164788, -2.888169013652136741, -8.200740947275496850 ) ) ;
#29636 = CARTESIAN_POINT ( 'NONE',  ( 112.7962614775786676, -6.222761293078241884, -8.102969835052219238 ) ) ;
#29637 = CARTESIAN_POINT ( 'NONE',  ( 89.01247232317646763, -26.75858941326842810, -11.54476601486570964 ) ) ;
#29638 = EDGE_CURVE ( 'NONE', #17567, #3982, #19242, .T. ) ;
#29639 = CARTESIAN_POINT ( 'NONE',  ( 121.3105849628857129, -6.095137211460710525, -18.44441274085890115 ) ) ;
#29640 = CARTESIAN_POINT ( 'NONE',  ( 113.2500748109119968, -3.505236298600246325, -18.68346056562440793 ) ) ;
#29641 = CARTESIAN_POINT ( 'NONE',  ( 111.9453614775786434, -1.561330072975668060, -17.79121239304076596 ) ) ;
#29642 = CARTESIAN_POINT ( 'NONE',  ( 120.4379860609119675, -6.564341423271550902, -7.887810678476487425 ) ) ;
#29643 = CARTESIAN_POINT ( 'NONE',  ( 126.2972081442452890, -2.084020599724406786, -8.691656652584148546 ) ) ;
#29644 = CARTESIAN_POINT ( 'NONE',  ( 112.3424481442453384, -3.505236298600246325, -18.68346056562440793 ) ) ;
#29645 = CARTESIAN_POINT ( 'NONE',  ( 121.9859814775786333, 0.2603800115204892296, -16.42320221600525088 ) ) ;
#29646 = CARTESIAN_POINT ( 'NONE',  ( 121.8158014775786171, -5.638512984488999180, -18.83840828888717311 ) ) ;
#29647 = ORIENTED_EDGE ( 'NONE', *, *, #29511, .F. ) ;
#29648 = CARTESIAN_POINT ( 'NONE',  ( 127.0264730702694038, -8.469371566854281497, -17.41871083769240514 ) ) ;
#29649 = CARTESIAN_POINT ( 'NONE',  ( 113.4690515045247992, -2.477300249445798297, -7.631215200338321125 ) ) ;
#29650 = CARTESIAN_POINT ( 'NONE',  ( 109.4407702545248355, 0.1403307496149616695, -11.32035403202665336 ) ) ;
#29651 = CARTESIAN_POINT ( 'NONE',  ( 107.4266296295248821, -4.863998795839590272, -8.388885654883775800 ) ) ;
#29652 = CARTESIAN_POINT ( 'NONE',  ( 87.80477198183443477, -25.23119213852205789, -15.24166438581092109 ) ) ;
#29653 = B_SPLINE_CURVE_WITH_KNOTS ( 'NONE', 3,
 ( #13921, #10506, #34205, #34424 ),
 .UNSPECIFIED., .F., .F.,
 ( 4, 4 ),
 ( 0.000000000000000000, 1.000000000000000000 ),
 .UNSPECIFIED. ) ;
#29654 = CARTESIAN_POINT ( 'NONE',  ( 114.9518748109119883, -1.834011780172310813, -8.268836392978581529 ) ) ;
#29655 = VERTEX_POINT ( 'NONE', #43193 ) ;
#29656 = LINE ( 'NONE', #15980, #36885 ) ;
#29657 = CARTESIAN_POINT ( 'NONE',  ( 124.0495485609119584, -0.08252387247370973622, -11.91645802438287483 ) ) ;
#29658 = CYLINDRICAL_SURFACE ( 'NONE', #8836, 3.500000000000003109 ) ;
#29659 = CARTESIAN_POINT ( 'NONE',  ( 112.8529881442453302, -7.894159318335828068, -9.358103419637847864 ) ) ;
#29660 = CARTESIAN_POINT ( 'NONE',  ( 111.8886348109120092, -3.383040157471821630, -19.15922257007629170 ) ) ;
#29661 = CARTESIAN_POINT ( 'NONE',  ( 118.8660148109119774, -10.30919188438810075, -12.61870101168855918 ) ) ;
#29662 = CARTESIAN_POINT ( 'NONE',  ( 108.6073327545248048, -2.477300249445798297, -19.15521520033831138 ) ) ;
#29663 = DIRECTION ( 'NONE',  ( 0.000000000000000000, 0.000000000000000000, -1.000000000000000000 ) ) ;
#29664 = ORIENTED_EDGE ( 'NONE', *, *, #6978, .T. ) ;
#29665 = CARTESIAN_POINT ( 'NONE',  ( 90.45092582798827152, -25.99489077589524300, -13.39321520033831625 ) ) ;
#29666 = CARTESIAN_POINT ( 'NONE',  ( 118.0718414775786442, -0.8288870151387760510, -10.36305467784173118 ) ) ;
#29667 = CARTESIAN_POINT ( 'NONE',  ( 116.7671281442453335, -1.834011780172310813, -8.268836392978581529 ) ) ;
#29668 = AXIS2_PLACEMENT_3D ( 'NONE', #11491, #4410, #43616 ) ;
#29669 = CARTESIAN_POINT ( 'NONE',  ( 114.7249681442453237, -9.565557343593413364, -10.61323700422348004 ) ) ;
#29670 = CARTESIAN_POINT ( 'NONE',  ( 113.8173414775786512, 0.2603800115204892296, -16.42320221600525088 ) ) ;
#29671 = CARTESIAN_POINT ( 'NONE',  ( 85.70478001548416103, -24.14644159042263993, -12.62951656296512937 ) ) ;
#29672 = CARTESIAN_POINT ( 'NONE',  ( 123.7445081442452874, -7.894159318335828068, -9.358103419637847864 ) ) ;
#29673 = CARTESIAN_POINT ( 'NONE',  ( 120.7947214775786193, -0.8288870151387760510, -10.36305467784173118 ) ) ;
#29674 = ORIENTED_EDGE ( 'NONE', *, *, #13860, .T. ) ;
#29675 = CARTESIAN_POINT ( 'NONE',  ( 122.8688454359119646, -11.07370829466463569, -12.81314460846529002 ) ) ;
#29676 = CARTESIAN_POINT ( 'NONE',  ( 112.1155414775786454, 0.9020085738987339008, -11.91225656197089222 ) ) ;
#29677 = CARTESIAN_POINT ( 'NONE',  ( 122.7234281442452755, -4.153390946401325223, -8.397313243818185668 ) ) ;
#29678 = ORIENTED_EDGE ( 'NONE', *, *, #12476, .T. ) ;
#29679 = CARTESIAN_POINT ( 'NONE',  ( 64.71877406242255404, -15.46959563142843130, -10.63875690036632271 ) ) ;
#29680 = CARTESIAN_POINT ( 'NONE',  ( 115.9162281442453235, -4.089484607189486809, -7.948022111789456723 ) ) ;
#29681 = CIRCLE ( 'NONE', #15855, 5.000000000000004441 ) ;
#29682 = CARTESIAN_POINT ( 'NONE',  ( 112.4272546295247821, -4.863998795839590272, -7.631215200338315796 ) ) ;
#29683 = CARTESIAN_POINT ( 'NONE',  ( 116.5402214775786405, -9.565557343593413364, -10.61323700422348004 ) ) ;
#29684 = ORIENTED_EDGE ( 'NONE', *, *, #22078, .F. ) ;
#29685 = ORIENTED_EDGE ( 'NONE', *, *, #8870, .F. ) ;
#29686 = CARTESIAN_POINT ( 'NONE',  ( 120.4543614775786295, -5.574606645277164318, -18.38911715685844683 ) ) ;
#29687 = CARTESIAN_POINT ( 'NONE',  ( 121.9292548109119849, -7.894159318335828068, -9.358103419637847864 ) ) ;
#29688 = CARTESIAN_POINT ( 'NONE',  ( 70.19189222814998175, -57.25954915413987578, -36.10662921840084749 ) ) ;
#29689 = VERTEX_POINT ( 'NONE', #4876 ) ;
#29690 = DIRECTION ( 'NONE',  ( 0.000000000000000000, 0.6004852223388321697, -0.7996358532186279566 ) ) ;
#29691 = CARTESIAN_POINT ( 'NONE',  ( 71.83824405425508530, -26.34469659010723674, -4.893215200338314474 ) ) ;
#29692 = CARTESIAN_POINT ( 'NONE',  ( 106.1764733795248219, -8.938348069036489818, -17.46756447353520159 ) ) ;
#29693 = AXIS2_PLACEMENT_3D ( 'NONE', #32049, #39124, #1043 ) ;
#29694 = CARTESIAN_POINT ( 'NONE',  ( 115.9162281442453235, -4.089484607189486809, -7.948022111789456723 ) ) ;
#29696 = CARTESIAN_POINT ( 'NONE',  ( 117.6180281442453150, -8.899110576539710493, -16.42337572283490132 ) ) ;
#29695 = CARTESIAN_POINT ( 'NONE',  ( 116.3700414775786527, -5.638512984488999180, -18.83840828888717311 ) ) ;
#29697 = CARTESIAN_POINT ( 'NONE',  ( 121.7023481442452777, -0.8288870151387760510, -10.36305467784173118 ) ) ;
#29698 = CARTESIAN_POINT ( 'NONE',  ( 113.2500748109119968, -6.344957434206662583, -7.627207830600332805 ) ) ;
#29699 = VERTEX_POINT ( 'NONE', #42963 ) ;
#29700 = CARTESIAN_POINT ( 'NONE',  ( 120.3409081442453044, -8.899110576539710493, -16.42337572283490132 ) ) ;
#29701 = DIRECTION ( 'NONE',  ( 1.000000000000000000, 0.000000000000000000, 0.000000000000000000 ) ) ;
#29702 = CARTESIAN_POINT ( 'NONE',  ( 113.5385046295247804, -4.863998795839590272, -7.631215200338315796 ) ) ;
#29703 = CARTESIAN_POINT ( 'NONE',  ( 91.77400275106518279, -26.75858941326842810, -11.54476601486570964 ) ) ;
#29704 = CARTESIAN_POINT ( 'NONE',  ( 109.6491296295247793, -4.863998795839590272, -19.15521520033831493 ) ) ;
#29705 = CARTESIAN_POINT ( 'NONE',  ( 117.3911214775786505, -1.561330072975668504, -17.79121239304076951 ) ) ;
#29706 = ORIENTED_EDGE ( 'NONE', *, *, #42726, .T. ) ;
#29707 = CARTESIAN_POINT ( 'NONE',  ( 120.7947214775786193, -9.261995988541697145, -16.69588392320189030 ) ) ;
#29708 = PLANE ( 'NONE',  #5052 ) ;
#29709 = CARTESIAN_POINT ( 'NONE',  ( 108.3295202545248657, -10.62599879583958717, -15.77991374673208469 ) ) ;
#29710 = CARTESIAN_POINT ( 'NONE',  ( 119.0929214775786278, -5.638512984488999180, -18.83840828888717311 ) ) ;
#29711 = CARTESIAN_POINT ( 'NONE',  ( 116.7671281442453335, -1.834011780172310813, -8.268836392978581529 ) ) ;
#29712 = DIRECTION ( 'NONE',  ( 1.000000000000000000, 2.774032902257834535E-17, 0.000000000000000000 ) ) ;
#29713 = CARTESIAN_POINT ( 'NONE',  ( 116.9589894550429250, -11.55723876051829180, -5.895360932783320962 ) ) ;
#29714 = VERTEX_POINT ( 'NONE', #29055 ) ;
#29715 = DIRECTION ( 'NONE',  ( 0.9908103287288504424, -0.1352586133457950590, 0.000000000000000000 ) ) ;
#29716 = CARTESIAN_POINT ( 'NONE',  ( 109.2295558771343309, -9.780153738166868393, -15.77098437576014334 ) ) ;
#29717 = CARTESIAN_POINT ( 'NONE',  ( 118.5256548109119876, -8.899110576539710493, -16.42337572283490132 ) ) ;
#29718 = CARTESIAN_POINT ( 'NONE',  ( 110.8992858795247827, -8.402594152722688392, -9.854619843455216355 ) ) ;
#29719 = CARTESIAN_POINT ( 'NONE',  ( 112.2883483795247770, -8.402594152722688392, -16.93181055722141792 ) ) ;
#29720 = CARTESIAN_POINT ( 'NONE',  ( 117.6747548109119919, -7.643976991954077427, -18.09477374809248928 ) ) ;
#29721 = CARTESIAN_POINT ( 'NONE',  ( 70.19189222814998175, -58.18802696105826300, -36.47801710466001879 ) ) ;
#29722 = CARTESIAN_POINT ( 'NONE',  ( 69.24601164033393275, -26.03124926770523473, -5.871647083323535021 ) ) ;
#29723 = CARTESIAN_POINT ( 'NONE',  ( 125.9001214775786224, -4.089484607189486809, -7.948022111789456723 ) ) ;
#29724 = CARTESIAN_POINT ( 'NONE',  ( 124.5954081442453116, -3.383040157471821630, -19.15922257007629170 ) ) ;
#29725 = ORIENTED_EDGE ( 'NONE', *, *, #19789, .F. ) ;
#29726 = CARTESIAN_POINT ( 'NONE',  ( 118.2420214775786320, -6.222761293078241884, -8.102969835052219238 ) ) ;
#29727 = CARTESIAN_POINT ( 'NONE',  ( 115.5758681442453053, -1.561330072975668060, -17.79121239304076951 ) ) ;
#29728 = CARTESIAN_POINT ( 'NONE',  ( 119.8870948109119752, -9.261995988541697145, -16.69588392320189030 ) ) ;
#29729 = CIRCLE ( 'NONE', #17371, 2.000000000000000444 ) ;
#29730 = CARTESIAN_POINT ( 'NONE',  ( 122.6099748109119929, -0.8288870151387760510, -10.36305467784173118 ) ) ;
#29731 = ORIENTED_EDGE ( 'NONE', *, *, #32082, .T. ) ;
#29732 = DIRECTION ( 'NONE',  ( 0.000000000000000000, -0.3818493186865927203, 0.9242245927363029745 ) ) ;
#29733 = ADVANCED_FACE ( 'NONE', ( #12409 ), #1673, .T. ) ;
#29734 = B_SPLINE_CURVE_WITH_KNOTS ( 'NONE', 3,
 ( #22347, #38995, #11422, #35559, #1141, #21449, #7764, #15277, #21672, #12092, #39677, #25548, #8217, #4103, #11867, #1367, #14837, #18924, #25997, #43324, #29185, #28747, #25329, #39221, #43097, #7986, #1581, #39901, #21895, #28973, #36016, #12769, #29863, #37372, #44238, #26894, #12998, #15960, #43779, #16187, #15733, #8662, #29635, #19597, #33481, #30312, #5679, #40814, #2260, #16643, #5234, #22564, #30092, #36907, #36468, #44008 ),
 .UNSPECIFIED., .F., .F.,
 ( 4, 2, 2, 2, 2, 2, 2, 1, 2, 2, 2, 2, 2, 2, 2, 2, 2, 2, 2, 2, 2, 1, 2, 2, 2, 2, 2, 2, 4 ),
 ( 0.000000000000000000, 0.06250000000003547163, 0.09375000000004662937, 0.1093750000000587308, 0.1250000000000708322, 0.1875000000001189049, 0.2187500000001370570, 0.2343750000001460498, 0.2421875000001448286, 0.2500000000001436073, 0.3125000000001424416, 0.3437500000001458278, 0.3593750000001435518, 0.3750000000001412759, 0.5000000000001461054, 0.5625000000001483258, 0.5937500000001509903, 0.6093750000001524336, 0.6250000000001537659, 0.6875000000001595390, 0.7187500000001625367, 0.7343750000001639799, 0.7421875000001597611, 0.7500000000001555422, 0.8125000000001221245, 0.8437500000001054712, 0.8593750000000912603, 0.8750000000000770495, 1.000000000000000000 ),
 .UNSPECIFIED. ) ;
#29735 = CARTESIAN_POINT ( 'NONE',  ( 123.1772414775786189, -4.089484607189486809, -7.948022111789456723 ) ) ;
#29736 = CARTESIAN_POINT ( 'NONE',  ( 112.1722681442453222, -8.899110576539710493, -16.42337572283490132 ) ) ;
#29737 = CARTESIAN_POINT ( 'NONE',  ( 111.3213681442453264, -7.643976991954077427, -18.09477374809248928 ) ) ;
#29738 = CARTESIAN_POINT ( 'NONE',  ( 107.4266296295248821, -4.863998795839590272, -19.15521520033831493 ) ) ;
#29739 = DIRECTION ( 'NONE',  ( 1.000000000000000000, 0.000000000000000000, 0.000000000000000000 ) ) ;
#29740 = DIRECTION ( 'NONE',  ( -0.000000000000000000, -0.9284778069183720062, -0.3713878862591650232 ) ) ;
#29741 = CARTESIAN_POINT ( 'NONE',  ( 111.4549108795247747, -1.325403438956436419, -16.93181055722141792 ) ) ;
#29742 = CARTESIAN_POINT ( 'NONE',  ( 123.3550173109119612, -9.289237151508434209, -11.05642687123711276 ) ) ;
#29743 = CARTESIAN_POINT ( 'NONE',  ( 136.8340972670076781, -10.06728345606325625, -11.39864759042615816 ) ) ;
#29744 = CARTESIAN_POINT ( 'NONE',  ( 117.9583881442453048, 0.1319031606808879209, -14.10382304977623669 ) ) ;
#29745 = CARTESIAN_POINT ( 'NONE',  ( 123.9146881442452894, 0.9020085738987339008, -11.91225656197089222 ) ) ;
#29746 = CARTESIAN_POINT ( 'NONE',  ( 136.4689272580752686, -7.050714571525749541, -18.72418924296322729 ) ) ;
#29747 = B_SPLINE_CURVE_WITH_KNOTS ( 'NONE', 3,
 ( #42042, #28350, #38371, #39056, #31761, #10582, #7827, #25387, #18312, #17419 ),
 .UNSPECIFIED., .F., .F.,
 ( 4, 3, 3, 4 ),
 ( 6.115116239063360172E-19, 1.132108808049913944E-05, 5.660634449920369976E-05, 9.445515394676020900E-05 ),
 .UNSPECIFIED. ) ;
#29748 = VERTEX_POINT ( 'NONE', #22656 ) ;
#29749 = LINE ( 'NONE', #25885, #14203 ) ;
#29750 = CARTESIAN_POINT ( 'NONE',  ( 108.2600671295247992, 0.1403307496149613920, -13.39321520033831447 ) ) ;
#29751 = CARTESIAN_POINT ( 'NONE',  ( 115.7460481442453357, -10.15424416112533912, -14.75197769757731336 ) ) ;
#29752 = FACE_OUTER_BOUND ( 'NONE', #6369, .T. ) ;
#29753 = ADVANCED_FACE ( 'NONE', ( #25643 ), #21988, .T. ) ;
#29754 = CARTESIAN_POINT ( 'NONE',  ( 66.95945348646621653, -0.07477774445813356596, -10.39321520033831270 ) ) ;
#29755 = CARTESIAN_POINT ( 'NONE',  ( 122.5731102343419536, -8.309924745830986836, -17.19909913565936321 ) ) ;
#29757 = CARTESIAN_POINT ( 'NONE',  ( 121.8725281442453223, -3.383040157471821630, -19.15922257007629170 ) ) ;
#29756 = CARTESIAN_POINT ( 'NONE',  ( 70.38348191167295909, -26.39350520520921961, -5.594626746640797954 ) ) ;
#29758 = CARTESIAN_POINT ( 'NONE',  ( 123.5743281442453139, -2.084020599724406786, -8.691656652584148546 ) ) ;
#29759 = EDGE_LOOP ( 'NONE', ( #36878, #15702, #31274, #19084 ) ) ;
#29760 = CARTESIAN_POINT ( 'NONE',  ( 114.7886454522301989, 0.1168444861213632779, -14.64321520033831447 ) ) ;
#29761 = CARTESIAN_POINT ( 'NONE',  ( 125.5030348109119558, -3.383040157471821630, -19.15922257007629170 ) ) ;
#29762 = CARTESIAN_POINT ( 'NONE',  ( 109.9963952545248134, -9.868328341294098749, -15.46607636864997204 ) ) ;
#29763 = ADVANCED_FACE ( 'NONE', ( #33125 ), #8531, .T. ) ;
#29764 = CARTESIAN_POINT ( 'NONE',  ( 121.7023481442452919, -0.8288870151387760510, -10.36305467784173118 ) ) ;
#29765 = CARTESIAN_POINT ( 'NONE',  ( 121.3052614775786111, -7.643976991954077427, -18.09477374809248928 ) ) ;
#29766 = ADVANCED_FACE ( 'NONE', ( #15822 ), #40217, .T. ) ;
#29767 = CARTESIAN_POINT ( 'NONE',  ( 124.1726284085855951, 1.449181222348162157, -18.30671709505454103 ) ) ;
#29768 = CARTESIAN_POINT ( 'NONE',  ( 106.1764733795248219, -8.938348069036489818, -17.46756447353520159 ) ) ;
#29769 = CARTESIAN_POINT ( 'NONE',  ( 75.95778847736481509, -3.256761025687722189, -7.993215200338315007 ) ) ;
#29770 = CARTESIAN_POINT ( 'NONE',  ( 82.31000308962319423, -13.76004065658516673, -18.64321520033831803 ) ) ;
#29771 = FACE_OUTER_BOUND ( 'NONE', #28846, .T. ) ;
#29772 = CARTESIAN_POINT ( 'NONE',  ( 109.7880358795247986, -0.7896495226426338832, -17.46756447353520159 ) ) ;
#29773 = CARTESIAN_POINT ( 'NONE',  ( -13.90346622911597052, -4.337920416975999061, -17.89321520033826474 ) ) ;
#29774 = CARTESIAN_POINT ( 'NONE',  ( 83.43891948909487155, -32.91635598341913749, -23.82430106395967684 ) ) ;
#29775 = CARTESIAN_POINT ( 'NONE',  ( 121.4187148109119789, -6.344957434206665248, -7.627207830600338134 ) ) ;
#29776 = CARTESIAN_POINT ( 'NONE',  ( 121.6456214775786293, -10.63000616557722466, -14.87417383870573495 ) ) ;
#29777 = CARTESIAN_POINT ( 'NONE',  ( 107.2182702545248105, -10.62599879583958717, -15.77991374673208469 ) ) ;
#29778 = CARTESIAN_POINT ( 'NONE',  ( 116.8238548109119819, -4.089484607189486809, -7.948022111789456723 ) ) ;
#29779 = FACE_OUTER_BOUND ( 'NONE', #25532, .T. ) ;
#29780 = ORIENTED_EDGE ( 'NONE', *, *, #24222, .T. ) ;
#29781 = DIRECTION ( 'NONE',  ( -0.000000000000000000, -0.9284778069183720062, -0.3713878862591650232 ) ) ;
#29782 = ADVANCED_FACE ( 'NONE', ( #36774 ), #5545, .F. ) ;
#29783 = CARTESIAN_POINT ( 'NONE',  ( 123.3474214775786209, -9.988377603198976828, -10.36322818467138340 ) ) ;
#29784 = CARTESIAN_POINT ( 'NONE',  ( 119.8870948109119752, -9.261995988541697145, -16.69588392320189030 ) ) ;
#29785 = CARTESIAN_POINT ( 'NONE',  ( 111.7184548109119788, -9.261995988541697145, -16.69588392320189030 ) ) ;
#29786 = ITEM_DEFINED_TRANSFORMATION ( 'NONE', 'NONE', #15478,  #12375 ) ;
#29787 = CARTESIAN_POINT ( 'NONE',  ( 112.7962614775786676, -6.222761293078241884, -8.102969835052219238 ) ) ;
#29788 = EDGE_CURVE ( 'NONE', #20112, #5874, #35740, .T. ) ;
#29789 = CARTESIAN_POINT ( 'NONE',  ( 113.7038881442453402, -6.222761293078241884, -8.102969835052219238 ) ) ;
#29790 = CARTESIAN_POINT ( 'NONE',  ( 124.4819548109119722, -7.893985811506177619, -18.51759400769804742 ) ) ;
#29791 = EDGE_CURVE ( 'NONE', #11630, #14918, #27142, .T. ) ;
#29792 = EDGE_CURVE ( 'NONE', #44542, #5526, #8097, .T. ) ;
#29793 = CARTESIAN_POINT ( 'NONE',  ( 107.0099108795247815, -8.938348069036489818, -9.318865927141430916 ) ) ;
#29794 = AXIS2_PLACEMENT_3D ( 'NONE', #838, #35482, #24574 ) ;
#29795 = CARTESIAN_POINT ( 'NONE',  ( 119.4332814775786318, -8.899110576539710493, -16.42337572283490132 ) ) ;
#29796 = CARTESIAN_POINT ( 'NONE',  ( 110.0170221536727553, 0.3967854368540359999, -10.50530088663810169 ) ) ;
#29797 = CARTESIAN_POINT ( 'NONE',  ( 124.3737138206744959, -2.348512537728041583, -17.99195118506215962 ) ) ;
#29798 = ORIENTED_EDGE ( 'NONE', *, *, #28095, .T. ) ;
#29799 = VECTOR ( 'NONE', #30889, 1000.000000000000000 ) ;
#29800 = CARTESIAN_POINT ( 'NONE',  ( 122.5910329359119970, -5.367793381288652910, -18.78638297431638904 ) ) ;
#29801 = CARTESIAN_POINT ( 'NONE',  ( 121.8158014775786171, -5.638512984488999180, -18.83840828888717311 ) ) ;
#29802 = CARTESIAN_POINT ( 'NONE',  ( 87.68939540009954214, -26.75858941326842810, -11.54476601486570964 ) ) ;
#29803 = CARTESIAN_POINT ( 'NONE',  ( 62.62817532774667484, -3.458832888097430835, -7.587504157255726689 ) ) ;
#29804 = FACE_OUTER_BOUND ( 'NONE', #29538, .T. ) ;
#29805 = CARTESIAN_POINT ( 'NONE',  ( 119.7169148109119874, -0.1624402480850797581, -16.17319339645315424 ) ) ;
#29806 = CARTESIAN_POINT ( 'NONE',  ( 68.15530245861752690, -1.266379369369464492, -16.39321520033831092 ) ) ;
#29807 = DIRECTION ( 'NONE',  ( 0.000000000000000000, 0.000000000000000000, -1.000000000000000000 ) ) ;
#29808 = CARTESIAN_POINT ( 'NONE',  ( 122.0427081442452817, -9.859900752359378018, -12.68260735090039759 ) ) ;
#29809 = CARTESIAN_POINT ( 'NONE',  ( 121.3408766859119794, -0.06289925094098414160, -9.412459353600681311 ) ) ;
#29810 = CARTESIAN_POINT ( 'NONE',  ( 135.5334395969766206, -4.108503626107443907, -19.33946713067309275 ) ) ;
#29811 = CARTESIAN_POINT ( 'NONE',  ( 125.3519896833715848, -11.65604236765752688, -15.30335118913170156 ) ) ;
#29812 = CARTESIAN_POINT ( 'NONE',  ( 125.1059481442452750, -8.166667518702819706, -8.995218007635861213 ) ) ;
#29813 = CARTESIAN_POINT ( 'NONE',  ( 118.0151148109119816, 0.4262465694468514643, -12.03445270309931736 ) ) ;
#29814 = CARTESIAN_POINT ( 'NONE',  ( 122.3830681442452857, -1.833838273342659697, -17.42832698103878286 ) ) ;
#29815 = VERTEX_POINT ( 'NONE', #20543 ) ;
#29816 = CARTESIAN_POINT ( 'NONE',  ( 124.6521348109119884, -1.561330072975668948, -17.79121239304076951 ) ) ;
#29817 = CARTESIAN_POINT ( 'NONE',  ( 116.2565881442452991, -9.261995988541697145, -16.69588392320189030 ) ) ;
#29818 = CARTESIAN_POINT ( 'NONE',  ( 114.5108483795247878, -8.402594152722688392, -16.93181055722141792 ) ) ;
#29819 = CARTESIAN_POINT ( 'NONE',  ( 112.6828081442453282, -2.084020599724406786, -8.691656652584148546 ) ) ;
#29820 = CARTESIAN_POINT ( 'NONE',  ( 124.8223148109119762, -10.15424416112533912, -14.75197769757731336 ) ) ;
#29821 = CARTESIAN_POINT ( 'NONE',  ( 122.4397948109119767, -9.988377603198976828, -10.36322818467138340 ) ) ;
#29822 = CARTESIAN_POINT ( 'NONE',  ( 112.9828796295247884, -4.863998795839590272, -19.15521520033831493 ) ) ;
#29823 = CARTESIAN_POINT ( 'NONE',  ( 109.0240515045248202, -6.936859964151250502, -18.39754474579286025 ) ) ;
#29824 = CARTESIAN_POINT ( 'NONE',  ( 80.41643495664496299, -3.865424785743087899, -15.89321520033831447 ) ) ;
#29825 = CARTESIAN_POINT ( 'NONE',  ( 113.4202548109119846, 0.1319031606808879209, -14.10382304977623669 ) ) ;
#29826 = AXIS2_PLACEMENT_3D ( 'NONE', #6204, #30601, #41338 ) ;
#29827 = CARTESIAN_POINT ( 'NONE',  ( 86.34560043013698305, -9.320000780048239619, -18.64321520033831803 ) ) ;
#29828 = CARTESIAN_POINT ( 'NONE',  ( 112.0105358795247810, -8.402594152722688392, -9.854619843455216355 ) ) ;
#29829 = ORIENTED_EDGE ( 'NONE', *, *, #29340, .T. ) ;
#29830 = AXIS2_PLACEMENT_3D ( 'NONE', #32338, #7057, #38275 ) ;
#29831 = CARTESIAN_POINT ( 'NONE',  ( 125.5597614775786326, -7.894159318335828068, -9.358103419637847864 ) ) ;
#29832 = CARTESIAN_POINT ( 'NONE',  ( 120.0212673109119805, -9.289237151508434209, -11.05642687123711276 ) ) ;
#29833 = CARTESIAN_POINT ( 'NONE',  ( 120.2296266859119953, -0.06289925094097943703, -9.412459353600674206 ) ) ;
#29834 = ORIENTED_EDGE ( 'NONE', *, *, #6115, .T. ) ;
#29835 = FACE_OUTER_BOUND ( 'NONE', #11565, .T. ) ;
#29836 = CARTESIAN_POINT ( 'NONE',  ( 107.2182702545248105, 0.1403307496149616695, -11.32035403202665336 ) ) ;
#29837 = EDGE_CURVE ( 'NONE', #44995, #38458, #224, .T. ) ;
#29838 = EDGE_LOOP ( 'NONE', ( #42896, #19118, #30703, #3683, #33879, #16900, #39035, #43819, #1711 ) ) ;
#29839 = CARTESIAN_POINT ( 'NONE',  ( 116.6536748109119941, 0.9020085738987339008, -11.91225656197089222 ) ) ;
#29840 = CARTESIAN_POINT ( 'NONE',  ( 124.2550481442452792, -0.1624402480850797581, -16.17319339645315424 ) ) ;
#29841 = CARTESIAN_POINT ( 'NONE',  ( 116.5402214775786405, -9.565557343593413364, -10.61323700422348004 ) ) ;
#29842 = VECTOR ( 'NONE', #43267, 1000.000000000000000 ) ;
#29843 = CARTESIAN_POINT ( 'NONE',  ( 2.181596283295915484, -11.50482699009217669, -7.393215200338315363 ) ) ;
#29844 = CARTESIAN_POINT ( 'NONE',  ( 114.7273308535611562, -2.239543233855025850, -18.13706010537467606 ) ) ;
#29845 = CARTESIAN_POINT ( 'NONE',  ( 114.8384214775786489, 0.9020085738987339008, -11.91225656197089222 ) ) ;
#29846 = ADVANCED_FACE ( 'NONE', ( #28053 ), #791, .T. ) ;
#29847 = CARTESIAN_POINT ( 'NONE',  ( 110.8992858795247827, -8.402594152722688392, -9.854619843455216355 ) ) ;
#29848 = ADVANCED_FACE ( 'NONE', ( #38079 ), #30693, .T. ) ;
#29849 = CARTESIAN_POINT ( 'NONE',  ( 124.0281414775786146, -1.834011780172310813, -8.268836392978581529 ) ) ;
#29850 = DIRECTION ( 'NONE',  ( -0.2768435750659239414, -0.3568721902840664151, 0.8921882507333142032 ) ) ;
#29851 = ORIENTED_EDGE ( 'NONE', *, *, #2037, .T. ) ;
#29852 = ADVANCED_FACE ( 'NONE', ( #34422 ), #6630, .T. ) ;
#29853 = CARTESIAN_POINT ( 'NONE',  ( 114.6682414775786469, -1.561330072975668060, -17.79121239304076596 ) ) ;
#29854 = CARTESIAN_POINT ( 'NONE',  ( 113.7038881442453402, -6.222761293078241884, -8.102969835052219238 ) ) ;
#29855 = CARTESIAN_POINT ( 'NONE',  ( 61.69189222814998175, -68.13214146720427777, -20.74076566292611545 ) ) ;
#29856 = CARTESIAN_POINT ( 'NONE',  ( 111.7184548109119788, -9.261995988541697145, -16.69588392320189030 ) ) ;
#29857 = EDGE_LOOP ( 'NONE', ( #31303, #45116, #30849, #39876 ) ) ;
#29858 = CARTESIAN_POINT ( 'NONE',  ( 122.2696148109119889, -4.089484607189486809, -7.948022111789456723 ) ) ;
#29859 = AXIS2_PLACEMENT_3D ( 'NONE', #21693, #6891, #10765 ) ;
#29860 = FACE_OUTER_BOUND ( 'NONE', #36863, .T. ) ;
#29861 = CARTESIAN_POINT ( 'NONE',  ( 115.6683931944929498, -1.036737761566197014, -17.24079555149560861 ) ) ;
#29862 = CARTESIAN_POINT ( 'NONE',  ( 90.71204046351577688, -10.71075648645643774, -8.143215200338314474 ) ) ;
#29863 = CARTESIAN_POINT ( 'NONE',  ( 137.3930029278099312, -3.553605451871880039, -8.436688146991468074 ) ) ;
#29864 = CARTESIAN_POINT ( 'NONE',  ( 112.7395348109119766, -4.153390946401321671, -8.397313243818183892 ) ) ;
#29865 = DIRECTION ( 'NONE',  ( -0.000000000000000000, -0.9284778069183721172, -0.3713878862591650232 ) ) ;
#29866 = CARTESIAN_POINT ( 'NONE',  ( 125.2638605181402056, -3.430414653771011846, -20.49516738280293637 ) ) ;
#29867 = CARTESIAN_POINT ( 'NONE',  ( 112.2289948109119848, -7.643976991954077427, -18.09477374809248928 ) ) ;
#29868 = CIRCLE ( 'NONE', #39339, 6.999999999999999112 ) ;
#29869 = CARTESIAN_POINT ( 'NONE',  ( 112.9097148109120070, 0.2603800115204892296, -16.42320221600525088 ) ) ;
#29870 = CARTESIAN_POINT ( 'NONE',  ( 124.4662673109119737, -9.289237151508434209, -11.05642687123711276 ) ) ;
#29871 = CARTESIAN_POINT ( 'NONE',  ( 126.5808414775786446, -9.859900752359378018, -12.68260735090039759 ) ) ;
#29872 = CARTESIAN_POINT ( 'NONE',  ( 114.0442481442453300, -7.643976991954077427, -18.09477374809248928 ) ) ;
#29873 = CARTESIAN_POINT ( 'NONE',  ( 124.5954081442453116, -3.383040157471821630, -19.15922257007629170 ) ) ;
#29874 = CARTESIAN_POINT ( 'NONE',  ( 123.1772414775786189, -4.089484607189486809, -7.948022111789456723 ) ) ;
#29875 = ORIENTED_EDGE ( 'NONE', *, *, #40181, .T. ) ;
#29876 = CARTESIAN_POINT ( 'NONE',  ( 114.9518748109119883, -1.834011780172310813, -8.268836392978581529 ) ) ;
#29877 = CARTESIAN_POINT ( 'NONE',  ( 112.7745202545247878, -10.62599879583958717, -15.77991374673208469 ) ) ;
#29878 = CARTESIAN_POINT ( 'NONE',  ( 111.1076452545248259, -9.868328341294098749, -15.46607636864997204 ) ) ;
#29879 = CARTESIAN_POINT ( 'NONE',  ( 106.9404577545248145, -2.791137627527939813, -18.39754474579286025 ) ) ;
#29880 = CARTESIAN_POINT ( 'NONE',  ( 96.46827370896536991, -25.99489077589524300, -13.39321520033831447 ) ) ;
#29881 = CARTESIAN_POINT ( 'NONE',  ( 120.1707281442453166, 0.2603800115204892296, -16.42320221600525088 ) ) ;
#29882 = VERTEX_POINT ( 'NONE', #24626 ) ;
#29883 = CARTESIAN_POINT ( 'NONE',  ( 126.1270281442452870, -10.30919188438810075, -12.61870101168855918 ) ) ;
#29884 = CARTESIAN_POINT ( 'NONE',  ( 124.4662673109119737, -9.289237151508427104, -11.05642687123710033 ) ) ;
#29885 = CARTESIAN_POINT ( 'NONE',  ( 119.5467348109119712, -5.574606645277192740, -18.38911715685844328 ) ) ;
#29886 = CARTESIAN_POINT ( 'NONE',  ( 114.9518748109119883, -7.643976991954077427, -18.09477374809248928 ) ) ;
#29887 = CARTESIAN_POINT ( 'NONE',  ( 105.8986608795248401, -1.325403438956436419, -16.93181055722141792 ) ) ;
#29888 = EDGE_CURVE ( 'NONE', #25152, #29197, #9209, .T. ) ;
#29889 = CARTESIAN_POINT ( 'NONE',  ( 121.0783548109119749, 0.2603800115204892296, -16.42320221600525088 ) ) ;
#29890 = CARTESIAN_POINT ( 'NONE',  ( 112.3578015045248861, -2.477300249445798297, -7.631215200338321125 ) ) ;
#29891 = CARTESIAN_POINT ( 'NONE',  ( 122.5664060953690466, -6.001247023715324147, -18.26661038929047010 ) ) ;
#29892 = ORIENTED_EDGE ( 'NONE', *, *, #7463, .T. ) ;
#29893 = CARTESIAN_POINT ( 'NONE',  ( 121.3619881442452879, -5.574606645277164318, -18.38911715685844683 ) ) ;
#29894 = CARTESIAN_POINT ( 'NONE',  ( 121.6456214775786293, 0.4262465694468514643, -12.03445270309931736 ) ) ;
#29895 = CARTESIAN_POINT ( 'NONE',  ( 119.3765548109119834, 0.9020085738987339008, -11.91225656197089222 ) ) ;
#29896 = CIRCLE ( 'NONE', #18239, 0.4999999999999999445 ) ;
#29897 = DIRECTION ( 'NONE',  ( -0.000000000000000000, -0.9284778069183718952, -0.3713878862591649677 ) ) ;
#29898 = CARTESIAN_POINT ( 'NONE',  ( 115.4056881442453459, -7.893985811506177619, -18.51759400769804742 ) ) ;
#29899 = CARTESIAN_POINT ( 'NONE',  ( 135.3184548109119874, -7.252096815532139473, -18.89748516540533529 ) ) ;
#29900 =( BOUNDED_CURVE ( )  B_SPLINE_CURVE ( 3, ( #8249, #4369, #8475, #721 ),
 .UNSPECIFIED., .F., .F. ) 
 B_SPLINE_CURVE_WITH_KNOTS ( ( 4, 4 ),
 ( 1.570796326794895004, 4.712388980384689674 ),
 .UNSPECIFIED. ) 
 CURVE ( )  GEOMETRIC_REPRESENTATION_ITEM ( )  RATIONAL_B_SPLINE_CURVE ( ( 1.000000000000000000, 0.3333333333333335369, 0.3333333333333335369, 1.000000000000000000 ) ) 
 REPRESENTATION_ITEM ( '' )  );
#29901 = CARTESIAN_POINT ( 'NONE',  ( 124.3685014775786328, 0.4262465694468514643, -12.03445270309931736 ) ) ;
#29902 = CARTESIAN_POINT ( 'NONE',  ( 119.3198281442452924, -9.859900752359374465, -12.68260735090039404 ) ) ;
#29903 = VERTEX_POINT ( 'NONE', #3203 ) ;
#29904 = CARTESIAN_POINT ( 'NONE',  ( 121.7575954359119805, -11.07370829466463569, -12.81314460846529002 ) ) ;
#29905 = CIRCLE ( 'NONE', #38632, 2.000000000000000444 ) ;
#29906 = ADVANCED_FACE ( 'NONE', ( #31016 ), #33574, .T. ) ;
#29907 = CARTESIAN_POINT ( 'NONE',  ( 112.8529881442453302, -1.561330072975668060, -17.79121239304076596 ) ) ;
#29908 = CARTESIAN_POINT ( 'NONE',  ( 119.8870948109119752, -0.8288870151387760510, -10.36305467784173118 ) ) ;
#29909 = ORIENTED_EDGE ( 'NONE', *, *, #36724, .T. ) ;
#29910 = CONICAL_SURFACE ( 'NONE', #15357, 5.000000000000000888, 0.7853981633974419507 ) ;
#29911 = CARTESIAN_POINT ( 'NONE',  ( 119.9518141859119851, -0.8832429491016019485, -18.19431474523657855 ) ) ;
#29912 = CARTESIAN_POINT ( 'NONE',  ( 118.2987481442453088, -1.561330072975668504, -17.79121239304076951 ) ) ;
#29913 = CARTESIAN_POINT ( 'NONE',  ( 112.0799890045248475, 0.8980012041604421569, -15.77991374673208469 ) ) ;
#29914 = CARTESIAN_POINT ( 'NONE',  ( 114.4413348109119823, -0.8288870151387760510, -10.36305467784173118 ) ) ;
#29915 = ORIENTED_EDGE ( 'NONE', *, *, #3612, .T. ) ;
#29916 = ORIENTED_EDGE ( 'NONE', *, *, #44807, .T. ) ;
#29917 = CARTESIAN_POINT ( 'NONE',  ( 124.4819548109119722, -2.084020599724406786, -8.691656652584148546 ) ) ;
#29918 = CARTESIAN_POINT ( 'NONE',  ( 120.1140014775786398, -7.894159318335828068, -9.358103419637847864 ) ) ;
#29919 = SURFACE_STYLE_USAGE ( .BOTH. , #19885 ) ;
#29920 = DIRECTION ( 'NONE',  ( -1.000000000000000000, 0.000000000000000000, 0.000000000000000000 ) ) ;
#29921 = CARTESIAN_POINT ( 'NONE',  ( 118.8092881442453290, -9.988377603198976828, -10.36322818467138340 ) ) ;
#29922 = CARTESIAN_POINT ( 'NONE',  ( 106.6626452545248611, 0.8980012041604421569, -11.00651665394454071 ) ) ;
#29923 = CIRCLE ( 'NONE', #10281, 4.500000000000003553 ) ;
#29924 = EDGE_CURVE ( 'NONE', #9778, #1762, #2119, .T. ) ;
#29925 = CARTESIAN_POINT ( 'NONE',  ( 116.8805814775786445, -6.344957434206662583, -7.627207830600332805 ) ) ;
#29927 = CARTESIAN_POINT ( 'NONE',  ( 115.8027748109119841, -8.899110576539710493, -16.42337572283490132 ) ) ;
#29926 = CARTESIAN_POINT ( 'NONE',  ( 116.7104014775786425, -0.4660016031367893996, -10.09054647747474043 ) ) ;
#29928 = CARTESIAN_POINT ( 'NONE',  ( 124.9924948109119924, -5.574606645277164318, -18.38911715685844683 ) ) ;
#29929 = CARTESIAN_POINT ( 'NONE',  ( 113.7038881442453402, -3.383040157471821630, -19.15922257007629170 ) ) ;
#29930 = ORIENTED_EDGE ( 'NONE', *, *, #4384, .F. ) ;
#29931 = CARTESIAN_POINT ( 'NONE',  ( 123.6310548109119765, -4.153390946401325223, -8.397313243818185668 ) ) ;
#29932 = CARTESIAN_POINT ( 'NONE',  ( 125.4584548109119737, -4.863998795839242995, -13.39321520033831447 ) ) ;
#29933 = CARTESIAN_POINT ( 'NONE',  ( 114.1934435773848833, -2.467220198592768199, -17.83387418641523325 ) ) ;
#29934 = CARTESIAN_POINT ( 'NONE',  ( 114.7886608795247696, -8.938348069036489818, -9.318865927141430916 ) ) ;
#29935 = CARTESIAN_POINT ( 'NONE',  ( 114.2330358795247776, -8.402594152722688392, -9.854619843455216355 ) ) ;
#29936 = CARTESIAN_POINT ( 'NONE',  ( 112.9134265045247645, -7.250697342233347165, -19.15521520033831138 ) ) ;
#29937 = CARTESIAN_POINT ( 'NONE',  ( 117.6747548109119919, -1.834011780172310813, -8.268836392978581529 ) ) ;
#29938 = ORIENTED_EDGE ( 'NONE', *, *, #3313, .F. ) ;
#29939 = AXIS2_PLACEMENT_3D ( 'NONE', #14835, #32593, #35331 ) ;
#29940 = CARTESIAN_POINT ( 'NONE',  ( 121.4187148109119789, -6.344957434206665248, -7.627207830600338134 ) ) ;
#29941 = FACE_OUTER_BOUND ( 'NONE', #29759, .T. ) ;
#29942 = CARTESIAN_POINT ( 'NONE',  ( 107.8433483795247838, -0.7896495226426338832, -9.318865927141430916 ) ) ;
#29943 = CARTESIAN_POINT ( 'NONE',  ( 120.3409081442453044, -0.4660016031367893996, -10.09054647747474043 ) ) ;
#29944 = CARTESIAN_POINT ( 'NONE',  ( 121.5888948109119809, -10.30919188438810075, -12.61870101168855918 ) ) ;
#29945 = CARTESIAN_POINT ( 'NONE',  ( 64.59905953672186740, -2.705726756842734559, -18.63794755288801852 ) ) ;
#29946 = CARTESIAN_POINT ( 'NONE',  ( 116.6234607133849295, -11.86235199658483985, -6.412683223725688109 ) ) ;
#29947 = VERTEX_POINT ( 'NONE', #30183 ) ;
#29948 = DIRECTION ( 'NONE',  ( 0.000000000000000000, -0.3818493186865927203, 0.9242245927363029745 ) ) ;
#29949 = CARTESIAN_POINT ( 'NONE',  ( 113.0231681442453180, -10.15424416112533912, -14.75197769757731336 ) ) ;
#29950 = CARTESIAN_POINT ( 'NONE',  ( 125.7299414775786346, -10.15424416112533912, -14.75197769757731336 ) ) ;
#29951 = CARTESIAN_POINT ( 'NONE',  ( 111.9410827545248708, -6.936859964151250502, -8.388885654883777576 ) ) ;
#29952 = CARTESIAN_POINT ( 'NONE',  ( 113.3301452545248083, -9.868328341294098749, -15.46607636864997204 ) ) ;
#29953 = CARTESIAN_POINT ( 'NONE',  ( 119.4332814775786318, -8.899110576539710493, -16.42337572283490132 ) ) ;
#29954 = DIRECTION ( 'NONE',  ( -0.000000000000000000, -0.9284778069183718952, -0.3713878862591649677 ) ) ;
#29955 = CARTESIAN_POINT ( 'NONE',  ( 69.16666358353634791, -25.68530218154914024, -5.871463680831265464 ) ) ;
#29956 = CARTESIAN_POINT ( 'NONE',  ( 126.2404814775786264, -9.261995988541697145, -16.69588392320189030 ) ) ;
#29957 = CARTESIAN_POINT ( 'NONE',  ( 121.9859814775786333, 0.2603800115204892296, -16.42320221600525088 ) ) ;
#29958 = ORIENTED_EDGE ( 'NONE', *, *, #37559, .T. ) ;
#29959 = CARTESIAN_POINT ( 'NONE',  ( 122.3263414775786373, -3.505236298600246325, -18.68346056562440793 ) ) ;
#29960 = CARTESIAN_POINT ( 'NONE',  ( 115.0086014775786509, -4.089484607189486809, -7.948022111789456723 ) ) ;
#29961 = CARTESIAN_POINT ( 'NONE',  ( 121.8725281442453223, -3.383040157471821630, -19.15922257007629170 ) ) ;
#29962 = EDGE_CURVE ( 'NONE', #11942, #40078, #22963, .T. ) ;
#29963 = CARTESIAN_POINT ( 'NONE',  ( 122.4397948109119767, -0.1624402480850797581, -16.17319339645315424 ) ) ;
#29964 = VERTEX_POINT ( 'NONE', #40675 ) ;
#29965 = CARTESIAN_POINT ( 'NONE',  ( 120.7852516859119731, -0.6942167230862464899, -9.935906262978006609 ) ) ;
#29966 = CIRCLE ( 'NONE', #16868, 2.999999999999999556 ) ;
#29967 = CARTESIAN_POINT ( 'NONE',  ( 123.1205148109119563, -1.834011780172310813, -8.268836392978581529 ) ) ;
#29968 = CARTESIAN_POINT ( 'NONE',  ( 124.3692356341924636, -8.482484215924628757, -6.318052624112218574 ) ) ;
#29969 = CARTESIAN_POINT ( 'NONE',  ( 124.4252281442452812, -9.261995988541697145, -16.69588392320189030 ) ) ;
#29970 = CARTESIAN_POINT ( 'NONE',  ( 106.7320983795247855, -0.7896495226426338832, -9.318865927141430916 ) ) ;
#29971 = PLANE ( 'NONE',  #44666 ) ;
#29972 = CARTESIAN_POINT ( 'NONE',  ( 127.9617136114945879, -3.003383010795549701, -14.62204112140151047 ) ) ;
#29973 = CARTESIAN_POINT ( 'NONE',  ( 107.6349890045248401, -9.868328341294098749, -11.32035403202665869 ) ) ;
#29974 = CARTESIAN_POINT ( 'NONE',  ( 96.46827370896536991, -24.99618726903056753, -13.53781830588664903 ) ) ;
#29975 = CARTESIAN_POINT ( 'NONE',  ( 119.2063748109119814, -7.894159318335828068, -9.358103419637847864 ) ) ;
#29976 = CARTESIAN_POINT ( 'NONE',  ( 124.5386814775786206, -5.638512984488999180, -18.83840828888717311 ) ) ;
#29977 = CARTESIAN_POINT ( 'NONE',  ( 126.9932531981088033, -0.01566132117990067310, -11.04423515009607470 ) ) ;
#29978 = ORIENTED_EDGE ( 'NONE', *, *, #41810, .F. ) ;
#29979 = CARTESIAN_POINT ( 'NONE',  ( 115.7132342721482843, -2.287189184988710267, -18.07361239780447448 ) ) ;
#29980 = CARTESIAN_POINT ( 'NONE',  ( 114.7816948109119863, -9.859900752359374465, -12.68260735090039404 ) ) ;
#29981 = CARTESIAN_POINT ( 'NONE',  ( 113.1366214775786432, -7.643976991954077427, -18.09477374809248928 ) ) ;
#29983 = AXIS2_PLACEMENT_3D ( 'NONE', #42192, #23976, #3209 ) ;
#29982 = CARTESIAN_POINT ( 'NONE',  ( 66.70735521015549807, -0.06012111411771998981, -10.39321520033831625 ) ) ;
#29984 = CARTESIAN_POINT ( 'NONE',  ( 111.8319081442453182, -4.153390946401321671, -8.397313243818183892 ) ) ;
#29986 = CARTESIAN_POINT ( 'NONE',  ( 121.9859814775786333, 0.2603800115204892296, -16.42320221600525088 ) ) ;
#29985 = CARTESIAN_POINT ( 'NONE',  ( 76.69189222814998175, -45.49566950204133065, -19.39321520033831447 ) ) ;
#29987 = CARTESIAN_POINT ( 'NONE',  ( 121.0783548109119749, -9.565557343593413364, -10.61323700422348004 ) ) ;
#29988 = ORIENTED_EDGE ( 'NONE', *, *, #21144, .T. ) ;
#29989 = CARTESIAN_POINT ( 'NONE',  ( 109.9772457829843830, 0.6362173239733635022, -14.64321520033829849 ) ) ;
#29990 = CARTESIAN_POINT ( 'NONE',  ( 65.92902809793561403, -15.33347626600828839, -10.39321520033831803 ) ) ;
#29991 = CARTESIAN_POINT ( 'NONE',  ( 111.5243640045248412, 0.1403307496149616695, -15.46607636864997204 ) ) ;
#29992 = CARTESIAN_POINT ( 'NONE',  ( 122.0427081442452817, -9.859900752359378018, -12.68260735090039759 ) ) ;
#29993 = CARTESIAN_POINT ( 'NONE',  ( 118.9794681442453026, -0.8288870151387760510, -10.36305467784173118 ) ) ;
#29994 = CARTESIAN_POINT ( 'NONE',  ( 124.6574308310796937, 1.356445862163998095, -18.15072565491285417 ) ) ;
#29995 = CARTESIAN_POINT ( 'NONE',  ( 113.3995983795247895, -8.402594152722688392, -16.93181055722141792 ) ) ;
#29996 = VECTOR ( 'NONE', #38715, 1000.000000000000000 ) ;
#29997 = DIRECTION ( 'NONE',  ( 1.000000000000000000, 0.000000000000000000, -0.000000000000000000 ) ) ;
#29998 = PLANE ( 'NONE',  #7766 ) ;
#29999 = CARTESIAN_POINT ( 'NONE',  ( -13.43709533753589724, -4.951753300544988967, -8.615451148147142746 ) ) ;
#30000 = CARTESIAN_POINT ( 'NONE',  ( 111.5938171295247940, -10.62599879583958540, -13.39321520033831447 ) ) ;
#30001 = CARTESIAN_POINT ( 'NONE',  ( -13.59781860028402889, -3.880472447307081740, -18.65072185953338391 ) ) ;
#30002 = CARTESIAN_POINT ( 'NONE',  ( 115.3442858795247759, -0.7896495226426338832, -17.46756447353520159 ) ) ;
#30003 = CARTESIAN_POINT ( 'NONE',  ( 120.5678148109119832, -8.166667518702819706, -8.995218007635861213 ) ) ;
#30004 = CARTESIAN_POINT ( 'NONE',  ( 121.5888948109119809, -10.30919188438810075, -12.61870101168855918 ) ) ;
#30005 = CARTESIAN_POINT ( 'NONE',  ( 105.7597546295248350, -4.863998795839590272, -7.631215200338315796 ) ) ;
#30006 = CARTESIAN_POINT ( 'NONE',  ( 117.0507614775786465, -10.30919188438810075, -12.61870101168855918 ) ) ;
#30007 = CARTESIAN_POINT ( 'NONE',  ( 111.7184548109119788, -8.862178061932382889, -16.39564131203247399 ) ) ;
#30008 = ORIENTED_EDGE ( 'NONE', *, *, #13912, .T. ) ;
#30009 = CARTESIAN_POINT ( 'NONE',  ( 112.5661454522301739, 0.1168444861213632779, -14.64321520033832691 ) ) ;
#30010 = CARTESIAN_POINT ( 'NONE',  ( 124.7088614775786226, 0.2603800115204892296, -16.42320221600525088 ) ) ;
#30011 = CARTESIAN_POINT ( 'NONE',  ( 121.1350814775786233, 0.5811942927096110934, -14.16772938898807510 ) ) ;
#30012 = CARTESIAN_POINT ( 'NONE',  ( 112.2289948109119848, -1.834011780172310813, -8.268836392978581529 ) ) ;
#30013 = CARTESIAN_POINT ( 'NONE',  ( 114.2144281442453178, -1.833838273342658809, -17.42832698103878286 ) ) ;
#30014 = ORIENTED_EDGE ( 'NONE', *, *, #23940, .T. ) ;
#30015 = CARTESIAN_POINT ( 'NONE',  ( 114.8384214775786489, -10.15424416112533912, -14.75197769757731336 ) ) ;
#30016 = CARTESIAN_POINT ( 'NONE',  ( 124.3117748109119844, -10.30919188438810075, -12.61870101168855918 ) ) ;
#30017 = EDGE_CURVE ( 'NONE', #4387, #12877, #2254, .T. ) ;
#30018 = CARTESIAN_POINT ( 'NONE',  ( 111.3160046295247838, -4.863998795839590272, -7.631215200338315796 ) ) ;
#30019 = AXIS2_PLACEMENT_3D ( 'NONE', #18772, #29477, #14282 ) ;
#30020 = CARTESIAN_POINT ( 'NONE',  ( 120.2274548109119934, -9.859900752359378018, -12.68260735090039759 ) ) ;
#30021 = CARTESIAN_POINT ( 'NONE',  ( 116.8068830708325692, -2.406742318435596051, -17.99911713909528643 ) ) ;
#30022 = CARTESIAN_POINT ( 'NONE',  ( 63.69189222814998175, -64.02637234200076932, -46.77412892735921446 ) ) ;
#30023 = VERTEX_POINT ( 'NONE', #23118 ) ;
#30024 = APPLICATION_CONTEXT ( 'automotive_design' ) ;
#30025 = CARTESIAN_POINT ( 'NONE',  ( 66.56203039180191183, 0.2060721959768717360, -11.55262144894435927 ) ) ;
#30026 = EDGE_CURVE ( 'NONE', #15215, #13698, #9263, .T. ) ;
#30027 = CARTESIAN_POINT ( 'NONE',  ( 124.2550481442452792, -9.988377603198980381, -10.36322818467138518 ) ) ;
#30028 = DIRECTION ( 'NONE',  ( 0.000000000000000000, -0.9242245927363027524, -0.3818493186865929423 ) ) ;
#30029 = AXIS2_PLACEMENT_3D ( 'NONE', #40574, #27115, #26439 ) ;
#30030 = DIRECTION ( 'NONE',  ( 1.000000000000000000, 0.000000000000000000, -0.000000000000000000 ) ) ;
#30031 = CARTESIAN_POINT ( 'NONE',  ( 122.3132204359119868, 1.345710702986147034, -13.97328579221134603 ) ) ;
#30032 = FACE_OUTER_BOUND ( 'NONE', #24789, .T. ) ;
#30033 = CARTESIAN_POINT ( 'NONE',  ( 105.4124890045248293, -9.868328341294098749, -11.32035403202665869 ) ) ;
#30034 = CARTESIAN_POINT ( 'NONE',  ( 70.19189222814998175, -61.33395589173655793, -37.73637771078311687 ) ) ;
#30035 = LINE ( 'NONE', #36636, #41330 ) ;
#30036 = CARTESIAN_POINT ( 'NONE',  ( 125.3358932077582892, -11.73929824459550986, -15.14057442325835012 ) ) ;
#30037 = CARTESIAN_POINT ( 'NONE',  ( 125.9568481442452850, -6.344957434206665248, -7.627207830600338134 ) ) ;
#30038 = CARTESIAN_POINT ( 'NONE',  ( 116.1431348109119881, 0.1319031606808879209, -14.10382304977623669 ) ) ;
#30039 = CARTESIAN_POINT ( 'NONE',  ( 119.7434548109119561, -0.3205909622538446468, -16.32243156402693174 ) ) ;
#30040 = EDGE_CURVE ( 'NONE', #12514, #7405, #33551, .T. ) ;
#30041 = ORIENTED_EDGE ( 'NONE', *, *, #45087, .F. ) ;
#30042 = CARTESIAN_POINT ( 'NONE',  ( 121.6456214775786293, -10.63000616557722466, -14.87417383870573495 ) ) ;
#30043 = CARTESIAN_POINT ( 'NONE',  ( 116.7104014775786425, -0.4660016031367893996, -10.09054647747474043 ) ) ;
#30044 = CARTESIAN_POINT ( 'NONE',  ( 115.2748327545248657, -6.936859964151250502, -8.388885654883777576 ) ) ;
#30045 = DIRECTION ( 'NONE',  ( 0.000000000000000000, 0.000000000000000000, -1.000000000000000000 ) ) ;
#30046 = EDGE_CURVE ( 'NONE', #12113, #41318, #34856, .T. ) ;
#30047 = EDGE_CURVE ( 'NONE', #14434, #10139, #14639, .T. ) ;
#30048 = CARTESIAN_POINT ( 'NONE',  ( 123.3474214775786209, -0.1624402480850797581, -16.17319339645315424 ) ) ;
#30050 = CARTESIAN_POINT ( 'NONE',  ( 124.4252281442452812, -9.261995988541697145, -16.69588392320189030 ) ) ;
#30049 = AXIS2_PLACEMENT_3D ( 'NONE', #43304, #5661, #5887 ) ;
#30051 = CARTESIAN_POINT ( 'NONE',  ( 113.4690515045247992, -2.477300249445798297, -7.631215200338321125 ) ) ;
#30052 = CARTESIAN_POINT ( 'NONE',  ( 107.0793640045248196, 0.1403307496149616695, -15.46607636864997204 ) ) ;
#30053 = CARTESIAN_POINT ( 'NONE',  ( 83.24887369766287293, -31.94491598976167168, -23.46817222872420317 ) ) ;
#30054 = CARTESIAN_POINT ( 'NONE',  ( 115.2355081442453155, 0.1319031606808879209, -14.10382304977623669 ) ) ;
#30055 = VECTOR ( 'NONE', #41845, 1000.000000000000227 ) ;
#30056 = CARTESIAN_POINT ( 'NONE',  ( 117.6747548109119919, -7.643976991954077427, -18.09477374809248928 ) ) ;
#30057 = DIRECTION ( 'NONE',  ( 1.156482317317869950E-15, 1.000000000000000000, 0.000000000000000000 ) ) ;
#30058 = CARTESIAN_POINT ( 'NONE',  ( 114.0941296295247867, -4.863998795839590272, -8.388885654883775800 ) ) ;
#30059 = ORIENTED_EDGE ( 'NONE', *, *, #37359, .F. ) ;
#30060 = CARTESIAN_POINT ( 'NONE',  ( 122.6099748109119929, -0.8288870151387726093, -10.36305467784173651 ) ) ;
#30061 = CARTESIAN_POINT ( 'NONE',  ( 126.1270281442452870, 0.1319031606808879209, -14.10382304977623669 ) ) ;
#30062 = CARTESIAN_POINT ( 'NONE',  ( 120.7157985609119635, -0.08252387247370887580, -11.91645802438286417 ) ) ;
#30063 = CARTESIAN_POINT ( 'NONE',  ( 121.6881423109119709, -9.959231468620755479, -10.70263013195267199 ) ) ;
#30064 = EDGE_LOOP ( 'NONE', ( #24637, #2353, #39252, #15532, #9312, #36623, #881 ) ) ;
#30065 = MECHANICAL_DESIGN_GEOMETRIC_PRESENTATION_REPRESENTATION (  '', ( #35187 ), #33689 ) ;
#30066 = DIRECTION ( 'NONE',  ( 0.1352586133457952255, 0.9908103287288504424, 0.000000000000000000 ) ) ;
#30067 = CARTESIAN_POINT ( 'NONE',  ( 116.5635957019662357, -11.89801664228175859, -21.17206575103167765 ) ) ;
#30068 = VERTEX_POINT ( 'NONE', #8420 ) ;
#30069 = AXIS2_PLACEMENT_3D ( 'NONE', #31143, #20894, #34335 ) ;
#30070 = CARTESIAN_POINT ( 'NONE',  ( 119.9438214775786378, -7.893985811506177619, -18.51759400769804742 ) ) ;
#30071 = CARTESIAN_POINT ( 'NONE',  ( 124.0281414775786146, -7.643976991954077427, -18.09477374809248928 ) ) ;
#30072 = CARTESIAN_POINT ( 'NONE',  ( 114.3846081442453197, 0.4262465694468514643, -12.03445270309931736 ) ) ;
#30073 =( NAMED_UNIT ( * ) PLANE_ANGLE_UNIT ( ) SI_UNIT ( $, .RADIAN. ) );
#30074 = CARTESIAN_POINT ( 'NONE',  ( 116.3176581477680145, -2.280480477428486363, -18.08254604495228435 ) ) ;
#30075 = CARTESIAN_POINT ( 'NONE',  ( 124.5386814775786206, -5.638512984489033819, -18.83840828888716956 ) ) ;
#30076 = CARTESIAN_POINT ( 'NONE',  ( 114.4980614775786592, -7.893985811506177619, -18.51759400769804742 ) ) ;
#30077 = EDGE_CURVE ( 'NONE', #7733, #35058, #13926, .T. ) ;
#30078 = CARTESIAN_POINT ( 'NONE',  ( 112.7745202545247878, 0.1403307496149616695, -11.32035403202665336 ) ) ;
#30079 = CARTESIAN_POINT ( 'NONE',  ( 125.1626748109119802, -9.988377603198980381, -10.36322818467138518 ) ) ;
#30080 = ORIENTED_EDGE ( 'NONE', *, *, #5785, .F. ) ;
#30081 = CARTESIAN_POINT ( 'NONE',  ( 114.2711548109119803, -9.988377603198976828, -10.36322818467138340 ) ) ;
#30082 = CARTESIAN_POINT ( 'NONE',  ( 115.5191414775786569, -6.222761293078241884, -8.102969835052219238 ) ) ;
#30083 = TOROIDAL_SURFACE ( 'NONE', #41747, 1.500000000000000000, 0.5000000000000000000 ) ;
#30084 = CARTESIAN_POINT ( 'NONE',  ( 9.052690036452151645, -4.182915634381243919, -7.393215200338315363 ) ) ;
#30085 = CARTESIAN_POINT ( 'NONE',  ( 112.1155414775786454, 0.9020085738987339008, -11.91225656197089222 ) ) ;
#30086 = VERTEX_POINT ( 'NONE', #7963 ) ;
#30087 = AXIS2_PLACEMENT_3D ( 'NONE', #22802, #25341, #28760 ) ;
#30088 = CARTESIAN_POINT ( 'NONE',  ( 122.3830681442452857, -8.166667518702819706, -8.995218007635861213 ) ) ;
#30089 = CARTESIAN_POINT ( 'NONE',  ( 71.02242295334774269, -63.74513109682822432, -41.80564703645547553 ) ) ;
#30090 = CARTESIAN_POINT ( 'NONE',  ( 115.9721219144190485, -1.220279397241700758, -16.99638242193885063 ) ) ;
#30091 = CARTESIAN_POINT ( 'NONE',  ( 123.9584548109119737, -1.204716393658298523, -20.50726132761981901 ) ) ;
#30092 = CARTESIAN_POINT ( 'NONE',  ( 136.1332990479140506, -2.569798562088685845, -7.975597057175941806 ) ) ;
#30093 = CARTESIAN_POINT ( 'NONE',  ( 114.2144281442453178, -1.833838273342658809, -17.42832698103878286 ) ) ;
#30094 = DIRECTION ( 'NONE',  ( -0.000000000000000000, -0.9284778069183721172, -0.3713878862591650232 ) ) ;
#30095 = CARTESIAN_POINT ( 'NONE',  ( 121.4551560953690483, -6.001247023715324147, -18.26661038929047010 ) ) ;
#30096 = CARTESIAN_POINT ( 'NONE',  ( 115.1220548109119761, -1.833838273342658809, -17.42832698103878286 ) ) ;
#30097 = CARTESIAN_POINT ( 'NONE',  ( 115.1787814775786387, -9.988377603198976828, -10.36322818467138340 ) ) ;
#30098 = CARTESIAN_POINT ( 'NONE',  ( 122.6604860609119640, -3.387241619883791355, -18.17469012370385073 ) ) ;
#30099 = CARTESIAN_POINT ( 'NONE',  ( 113.9307948109119906, 0.9020085738987339008, -11.91225656197089222 ) ) ;
#30100 = CARTESIAN_POINT ( 'NONE',  ( 113.9307948109119764, -10.15424416112533912, -14.75197769757731336 ) ) ;
#30101 = CARTESIAN_POINT ( 'NONE',  ( 121.7023481442452777, -9.261995988541697145, -16.69588392320189030 ) ) ;
#30102 = EDGE_CURVE ( 'NONE', #11934, #23514, #25751, .T. ) ;
#30103 = CARTESIAN_POINT ( 'NONE',  ( 121.7023481442452777, -9.261995988541697145, -16.69588392320189030 ) ) ;
#30104 = ORIENTED_EDGE ( 'NONE', *, *, #10025, .T. ) ;
#30105 = CARTESIAN_POINT ( 'NONE',  ( 112.7962614775786676, -3.383040157471821630, -19.15922257007629170 ) ) ;
#30106 = CARTESIAN_POINT ( 'NONE',  ( 112.8439733795247832, -8.938348069036489818, -17.46756447353520159 ) ) ;
#30107 = CARTESIAN_POINT ( 'NONE',  ( 110.6214733795247867, -1.325403438956436419, -9.854619843455211026 ) ) ;
#30108 = CARTESIAN_POINT ( 'NONE',  ( 110.8298327545248299, -6.936859964151250502, -8.388885654883777576 ) ) ;
#30109 = FACE_OUTER_BOUND ( 'NONE', #44395, .T. ) ;
#30110 = CARTESIAN_POINT ( 'NONE',  ( 118.5256548109119876, -0.4660016031367893996, -10.09054647747474043 ) ) ;
#30111 = ORIENTED_EDGE ( 'NONE', *, *, #41746, .T. ) ;
#30112 = CARTESIAN_POINT ( 'NONE',  ( 64.69189222814998175, -41.76310523276723785, -7.393215200338315363 ) ) ;
#30113 = CARTESIAN_POINT ( 'NONE',  ( 109.2294468747734300, -7.889554749245212939, -8.547382946171255824 ) ) ;
#30114 = CARTESIAN_POINT ( 'NONE',  ( 121.9470836909669913, -25.99489077589524300, -13.39321520033831447 ) ) ;
#30115 = ADVANCED_FACE ( 'NONE', ( #7738 ), #446, .T. ) ;
#30116 = CARTESIAN_POINT ( 'NONE',  ( 113.0798948109119948, -8.899110576539710493, -16.42337572283490132 ) ) ;
#30117 = CARTESIAN_POINT ( 'NONE',  ( 105.4124890045248293, -9.868328341294098749, -11.32035403202665869 ) ) ;
#30118 = CARTESIAN_POINT ( 'NONE',  ( 118.8092881442453290, -9.988377603198976828, -10.36322818467138340 ) ) ;
#30119 = VECTOR ( 'NONE', #43692, 1000.000000000000227 ) ;
#30120 = CARTESIAN_POINT ( 'NONE',  ( 115.6220983795247861, -8.402594152722688392, -16.93181055722141792 ) ) ;
#30121 = CARTESIAN_POINT ( 'NONE',  ( 61.69189222814998175, -80.85404093559408523, -31.07034979220001603 ) ) ;
#30122 = ORIENTED_EDGE ( 'NONE', *, *, #44046, .T. ) ;
#30123 = FACE_OUTER_BOUND ( 'NONE', #38384, .T. ) ;
#30124 = CARTESIAN_POINT ( 'NONE',  ( 123.1205148109119563, -7.643976991954077427, -18.09477374809248928 ) ) ;
#30125 = CIRCLE ( 'NONE', #32916, 0.3599999999999998201 ) ;
#30126 = CARTESIAN_POINT ( 'NONE',  ( 120.7947214775786193, -9.261995988541697145, -16.69588392320189030 ) ) ;
#30127 = CARTESIAN_POINT ( 'NONE',  ( 112.4559014775786778, -0.1624402480850797581, -16.17319339645315424 ) ) ;
#30128 = CARTESIAN_POINT ( 'NONE',  ( 117.0507614775786465, -10.30919188438810075, -12.61870101168855918 ) ) ;
#30129 = LINE ( 'NONE', #9605, #21288 ) ;
#30130 = CARTESIAN_POINT ( 'NONE',  ( 127.4620922276975534, -1.264427456653780091, -9.074754333436022335 ) ) ;
#30131 = CARTESIAN_POINT ( 'NONE',  ( 118.1285681442453068, -2.084020599724406786, -8.691656652584148546 ) ) ;
#30132 = ORIENTED_EDGE ( 'NONE', *, *, #15250, .F. ) ;
#30133 = CARTESIAN_POINT ( 'NONE',  ( 119.4332814775786318, -0.4660016031367946177, -10.09054647747473332 ) ) ;
#30134 = CIRCLE ( 'NONE', #23599, 2.999999999999999556 ) ;
#30135 = CARTESIAN_POINT ( 'NONE',  ( 114.5547881442453217, -5.638512984488999180, -18.83840828888717311 ) ) ;
#30136 = CARTESIAN_POINT ( 'NONE',  ( 121.7590748109119687, -2.084020599724406786, -8.691656652584148546 ) ) ;
#30137 = VERTEX_POINT ( 'NONE', #35080 ) ;
#30138 = CARTESIAN_POINT ( 'NONE',  ( 124.0495485609119584, -0.08252387247370887580, -11.91645802438286417 ) ) ;
#30139 = CARTESIAN_POINT ( 'NONE',  ( 120.0005481442453146, -5.638512984488999180, -18.83840828888717311 ) ) ;
#30140 = CARTESIAN_POINT ( 'NONE',  ( 114.0941296295247867, -4.863998795839590272, -19.15521520033831493 ) ) ;
#30141 = CARTESIAN_POINT ( 'NONE',  ( 115.7460481442453357, -10.15424416112533912, -14.75197769757731336 ) ) ;
#30142 = EDGE_LOOP ( 'NONE', ( #34871, #7574, #20092, #44985, #36236 ) ) ;
#30143 = EDGE_LOOP ( 'NONE', ( #3262, #39638, #501, #32714, #4289, #44128 ) ) ;
#30144 = CARTESIAN_POINT ( 'NONE',  ( 126.6375681442452930, -10.15424416112533912, -14.75197769757731336 ) ) ;
#30145 = CARTESIAN_POINT ( 'NONE',  ( 121.9859814775786333, -9.565557343593413364, -10.61323700422348004 ) ) ;
#30146 = CARTESIAN_POINT ( 'NONE',  ( 66.09831493924600920, -15.19954166770336990, -16.39321520033831447 ) ) ;
#30147 = EDGE_CURVE ( 'NONE', #32113, #45010, #9697, .T. ) ;
#30148 = CYLINDRICAL_SURFACE ( 'NONE', #40336, 1.999999999999998890 ) ;
#30149 = CARTESIAN_POINT ( 'NONE',  ( 118.7525614775786380, -8.166667518702819706, -8.995218007635861213 ) ) ;
#30150 = CARTESIAN_POINT ( 'NONE',  ( 106.5931921295248372, 0.8980012041604618078, -13.39321520033831447 ) ) ;
#30151 = CARTESIAN_POINT ( 'NONE',  ( 118.2420214775786320, -3.383040157471821630, -19.15922257007629170 ) ) ;
#30153 = CARTESIAN_POINT ( 'NONE',  ( 116.9940348109119839, -0.1624402480850797581, -16.17319339645315424 ) ) ;
#30152 = CARTESIAN_POINT ( 'NONE',  ( 114.6115148109119986, -3.383040157471821630, -19.15922257007629170 ) ) ;
#30154 = CARTESIAN_POINT ( 'NONE',  ( 124.4819548109119722, -2.084020599724406786, -8.691656652584148546 ) ) ;
#30155 = CARTESIAN_POINT ( 'NONE',  ( 114.1009748109119784, -4.089484607189486809, -7.948022111789456723 ) ) ;
#30156 = EDGE_LOOP ( 'NONE', ( #5633, #41808, #22755, #34567, #6390 ) ) ;
#30157 = CARTESIAN_POINT ( 'NONE',  ( 122.7801548109119665, -6.222761293078241884, -8.102969835052219238 ) ) ;
#30158 = PLANE ( 'NONE',  #40952 ) ;
#30159 = CARTESIAN_POINT ( 'NONE',  ( 143.3676850761856940, -41.90950876995113816, -19.14091845747268295 ) ) ;
#30160 = CARTESIAN_POINT ( 'NONE',  ( 113.3301452545248083, 0.8980012041604421569, -11.00651665394454071 ) ) ;
#30161 = CARTESIAN_POINT ( 'NONE',  ( 114.6497546295247929, -4.863998795839590272, -18.39754474579285315 ) ) ;
#30162 = CARTESIAN_POINT ( 'NONE',  ( 112.6356140045247827, -10.62599879583958717, -11.00651665394454604 ) ) ;
#30163 = ADVANCED_FACE ( 'NONE', ( #28948 ), #23240, .T. ) ;
#30164 = EDGE_CURVE ( 'NONE', #32198, #29032, #38222, .T. ) ;
#30165 = CARTESIAN_POINT ( 'NONE',  ( 123.2906948109119867, -8.166667518702819706, -8.995218007635861213 ) ) ;
#30166 = ORIENTED_EDGE ( 'NONE', *, *, #15266, .T. ) ;
#30167 = CARTESIAN_POINT ( 'NONE',  ( 119.4900081442453086, -1.834011780172310813, -8.268836392978581529 ) ) ;
#30168 = CARTESIAN_POINT ( 'NONE',  ( 113.2500748109119968, -3.505236298600246325, -18.68346056562440793 ) ) ;
#30169 = CARTESIAN_POINT ( 'NONE',  ( 65.49983523453742862, -18.16718729050178993, -4.893215200338314474 ) ) ;
#30170 = CARTESIAN_POINT ( 'NONE',  ( 121.1350814775786233, 0.5811942927096110934, -14.16772938898807510 ) ) ;
#30171 = CARTESIAN_POINT ( 'NONE',  ( 121.7023481442452777, -9.261995988541697145, -16.69588392320189030 ) ) ;
#30172 = CARTESIAN_POINT ( 'NONE',  ( 64.40214619852623912, -2.780995199376929516, -18.71258234879876881 ) ) ;
#30173 = CARTESIAN_POINT ( 'NONE',  ( 125.6164881442453094, -9.565557343593413364, -10.61323700422348004 ) ) ;
#30174 = CARTESIAN_POINT ( 'NONE',  ( 70.19189222814998175, -58.18802696105826300, -36.47801710466001879 ) ) ;
#30175 = CARTESIAN_POINT ( 'NONE',  ( 123.5633766859119760, -9.033780868592240054, -16.85052413769862056 ) ) ;
#30176 = ORIENTED_EDGE ( 'NONE', *, *, #16476, .T. ) ;
#30177 = CARTESIAN_POINT ( 'NONE',  ( -2.128438283008827092, -6.923168977537326185, -7.764336790352773576 ) ) ;
#30178 = CARTESIAN_POINT ( 'NONE',  ( 118.4645848073892722, -1.081026697600512732, -17.18181821144401056 ) ) ;
#30179 = CARTESIAN_POINT ( 'NONE',  ( 123.0637881442452937, -8.899110576539710493, -16.42337572283490132 ) ) ;
#30180 = CARTESIAN_POINT ( 'NONE',  ( 109.0240515045248202, -6.936859964151250502, -18.39754474579286025 ) ) ;
#30181 = CARTESIAN_POINT ( 'NONE',  ( 112.4967077545247633, -2.791137627527939813, -18.39754474579286025 ) ) ;
#30182 = CARTESIAN_POINT ( 'NONE',  ( 117.5045748109119756, -9.859900752359374465, -12.68260735090039404 ) ) ;
#30183 = CARTESIAN_POINT ( 'NONE',  ( 67.69189222814998175, -62.82237896425675672, -47.71602681600972318 ) ) ;
#30184 = CARTESIAN_POINT ( 'NONE',  ( 68.68839935636917460, -25.95913848132418522, -5.893215200338315363 ) ) ;
#30185 = CARTESIAN_POINT ( 'NONE',  ( 112.1155414775786454, -10.15424416112533912, -14.75197769757731336 ) ) ;
#30186 = CARTESIAN_POINT ( 'NONE',  ( 122.8936081442453059, 0.2603800115204892296, -16.42320221600525088 ) ) ;
#30187 = VERTEX_POINT ( 'NONE', #3570 ) ;
#30188 = CARTESIAN_POINT ( 'NONE',  ( 123.4608748109119745, 0.4262465694468514643, -12.03445270309931736 ) ) ;
#30189 = CARTESIAN_POINT ( 'NONE',  ( 114.4980614775786592, -7.893985811506177619, -18.51759400769804742 ) ) ;
#30190 = CARTESIAN_POINT ( 'NONE',  ( 124.5386814775786206, -5.638512984488999180, -18.83840828888717311 ) ) ;
#30191 = CARTESIAN_POINT ( 'NONE',  ( 124.5386814775786206, -4.153390946401325223, -8.397313243818185668 ) ) ;
#30192 = ORIENTED_EDGE ( 'NONE', *, *, #32304, .F. ) ;
#30193 = CARTESIAN_POINT ( 'NONE',  ( 123.3089807241438933, -2.443475742715334853, -17.86549347949429389 ) ) ;
#30194 = CARTESIAN_POINT ( 'NONE',  ( 125.0492214775786266, -6.344957434206665248, -7.627207830600338134 ) ) ;
#30195 = CARTESIAN_POINT ( 'NONE',  ( 114.3278814775786429, 0.1319031606808879209, -14.10382304977623669 ) ) ;
#30196 = CARTESIAN_POINT ( 'NONE',  ( 111.4348214775786801, -3.505236298600246325, -18.68346056562440793 ) ) ;
#30197 = CARTESIAN_POINT ( 'NONE',  ( 107.6349890045248401, 0.8980012041604421569, -15.77991374673208469 ) ) ;
#30198 = CARTESIAN_POINT ( 'NONE',  ( 68.80767435282035649, -66.83222807083036798, -34.76098800215376627 ) ) ;
#30199 = ORIENTED_EDGE ( 'NONE', *, *, #21172, .F. ) ;
#30200 = LINE ( 'NONE', #26098, #17198 ) ;
#30201=STYLED_ITEM('',(#45190),#36408);
#30202 = CARTESIAN_POINT ( 'NONE',  ( 108.9545983795247821, -8.402594152722688392, -16.93181055722141792 ) ) ;
#30203 = FACE_BOUND ( 'NONE', #7545, .T. ) ;
#30204 = CARTESIAN_POINT ( 'NONE',  ( 119.4332814775786318, -8.899110576539710493, -16.42337572283490132 ) ) ;
#30205 = CARTESIAN_POINT ( 'NONE',  ( 112.5693548109119888, 0.4262465694468514643, -12.03445270309931736 ) ) ;
#30206 = CARTESIAN_POINT ( 'NONE',  ( 126.8396850857285756, -0.1243826821608716021, -10.99732104622448681 ) ) ;
#30207 = VERTEX_POINT ( 'NONE', #41888 ) ;
#30208 = CARTESIAN_POINT ( 'NONE',  ( 115.6349575202278146, -2.239543233855044058, -18.13706010537467606 ) ) ;
#30209 = CARTESIAN_POINT ( 'NONE',  ( 117.2209414775786485, -2.084020599724406786, -8.691656652584148546 ) ) ;
#30210 = VECTOR ( 'NONE', #33601, 1000.000000000000114 ) ;
#30211 = CARTESIAN_POINT ( 'NONE',  ( 113.2500748109119968, -3.505236298600246325, -18.68346056562440793 ) ) ;
#30212 = DIRECTION ( 'NONE',  ( 0.000000000000000000, 0.000000000000000000, 1.000000000000000000 ) ) ;
#30213 = CARTESIAN_POINT ( 'NONE',  ( -2.674541079949086519, -7.087030491801339593, -19.34356310333839701 ) ) ;
#30215 = CARTESIAN_POINT ( 'NONE',  ( 121.2485348109119769, -0.4660016031367893996, -10.09054647747474043 ) ) ;
#30214 = CARTESIAN_POINT ( 'NONE',  ( 71.67504600870660170, -26.72445618319088823, -4.893215200338314474 ) ) ;
#30216 = ADVANCED_FACE ( 'NONE', ( #37780 ), #38668, .T. ) ;
#30217 = CARTESIAN_POINT ( 'NONE',  ( 112.2289948109119848, -1.834011780172310813, -8.268836392978581529 ) ) ;
#30218 = VERTEX_POINT ( 'NONE', #17273 ) ;
#30219 = DIRECTION ( 'NONE',  ( 0.000000000000000000, -0.3818493186865897226, 0.9242245927363041957 ) ) ;
#30220 = CARTESIAN_POINT ( 'NONE',  ( 121.9470836909669913, -25.99489077589524300, -13.39321520033831447 ) ) ;
#30221 = CARTESIAN_POINT ( 'NONE',  ( 106.3153796295248412, -4.863998795839590272, -8.388885654883775800 ) ) ;
#30222 = CARTESIAN_POINT ( 'NONE',  ( 125.1626748109119802, -0.1624402480850797581, -16.17319339645315424 ) ) ;
#30223 = CARTESIAN_POINT ( 'NONE',  ( 119.5467348109119712, -5.574606645277164318, -18.38911715685844683 ) ) ;
#30224 = CARTESIAN_POINT ( 'NONE',  ( 119.3722114740559448, -1.081026697600536046, -17.18181821144402832 ) ) ;
#30225 = CARTESIAN_POINT ( 'NONE',  ( 113.2606921295247702, -9.868328341294093420, -13.39321520033831447 ) ) ;
#30226 = CARTESIAN_POINT ( 'NONE',  ( 87.44708369096657918, -25.99489077589588604, -12.39321520033831447 ) ) ;
#30227 = CARTESIAN_POINT ( 'NONE',  ( 112.7962614775786676, -6.222761293078241884, -8.102969835052219238 ) ) ;
#30228 = CARTESIAN_POINT ( 'NONE',  ( 109.1629577545248395, -7.250697342233347165, -7.631215200338321125 ) ) ;
#30229 = DIRECTION ( 'NONE',  ( -0.9908103287288505534, 0.1352586133457950590, 0.000000000000000000 ) ) ;
#30230 = CARTESIAN_POINT ( 'NONE',  ( 116.1777233795247781, -8.938348069036489818, -17.46756447353520159 ) ) ;
#30231 = CARTESIAN_POINT ( 'NONE',  ( 122.4397948109119767, -9.988377603198976828, -10.36322818467138340 ) ) ;
#30232 = CARTESIAN_POINT ( 'NONE',  ( 122.3263414775786373, -6.344957434206665248, -7.627207830600338134 ) ) ;
#30233 = CARTESIAN_POINT ( 'NONE',  ( 69.69189222814998175, -41.76310523276723785, -20.39321520033831447 ) ) ;
#30234 = CARTESIAN_POINT ( 'NONE',  ( 118.1285681442453068, -7.893985811506177619, -18.51759400769804742 ) ) ;
#30235 = CARTESIAN_POINT ( 'NONE',  ( 113.1366214775786432, -1.834011780172310813, -8.268836392978581529 ) ) ;
#30236 = VERTEX_POINT ( 'NONE', #34787 ) ;
#30237 = CARTESIAN_POINT ( 'NONE',  ( 113.4202548109119846, 0.1319031606808879209, -14.10382304977623669 ) ) ;
#30238 = VECTOR ( 'NONE', #3222, 1000.000000000000000 ) ;
#30239 = CARTESIAN_POINT ( 'NONE',  ( 111.6050014775786536, 0.1319031606808879209, -14.10382304977623669 ) ) ;
#30240 = CARTESIAN_POINT ( 'NONE',  ( 121.2485348109119769, -0.4660016031367893996, -10.09054647747474043 ) ) ;
#30241 = CARTESIAN_POINT ( 'NONE',  ( 113.5904348109119866, -7.893985811506177619, -18.51759400769804742 ) ) ;
#30242 = CARTESIAN_POINT ( 'NONE',  ( 113.1933481442453058, -5.574606645277164318, -18.38911715685844683 ) ) ;
#30243 = ORIENTED_EDGE ( 'NONE', *, *, #29167, .F. ) ;
#30244 = CARTESIAN_POINT ( 'NONE',  ( 119.3198281442452924, -9.859900752359374465, -12.68260735090039404 ) ) ;
#30245 = CARTESIAN_POINT ( 'NONE',  ( 111.6617281442453304, 0.4262465694468514643, -12.03445270309931736 ) ) ;
#30246 = CARTESIAN_POINT ( 'NONE',  ( 107.6349890045248401, 0.8980012041604421569, -15.77991374673208469 ) ) ;
#30247 = CARTESIAN_POINT ( 'NONE',  ( 121.4187148109119789, -3.505236298600246325, -18.68346056562440793 ) ) ;
#30248 = CARTESIAN_POINT ( 'NONE',  ( 116.8247182375590825, -1.639145683561697542, -17.51101245992349220 ) ) ;
#30249 = VERTEX_POINT ( 'NONE', #10207 ) ;
#30250 = CARTESIAN_POINT ( 'NONE',  ( 122.9382985609119743, -0.08252387247370887580, -11.91645802438286417 ) ) ;
#30251 = CARTESIAN_POINT ( 'NONE',  ( 121.6456214775786293, -10.63000616557722466, -14.87417383870573495 ) ) ;
#30252 = FACE_OUTER_BOUND ( 'NONE', #34368, .T. ) ;
#30253 = SURFACE_SIDE_STYLE ('',( #27520 ) ) ;
#30254 = PRODUCT_RELATED_PRODUCT_CATEGORY ( 'part', '', ( #28885 ) ) ;
#30255 = CARTESIAN_POINT ( 'NONE',  ( 112.6260814775786514, -9.261995988541698921, -16.69588392320189030 ) ) ;
#30256 = CARTESIAN_POINT ( 'NONE',  ( 70.19189222814998175, -60.04498257489500190, -37.22079287717834717 ) ) ;
#30257 = CARTESIAN_POINT ( 'NONE',  ( 108.3295202545248657, 0.1403307496149616695, -11.32035403202665336 ) ) ;
#30258 = CARTESIAN_POINT ( 'NONE',  ( 109.5083551332721896, 0.2334052082820642360, -14.64321520033828605 ) ) ;
#30259 = CARTESIAN_POINT ( 'NONE',  ( 137.3872759786617053, -6.189116507261323008, -18.35186304430243709 ) ) ;
#30260 = VECTOR ( 'NONE', #6439, 1000.000000000000000 ) ;
#30261 = CARTESIAN_POINT ( 'NONE',  ( 125.0889430353348786, -2.469647041402692977, -17.83064248237198868 ) ) ;
#30262 = CARTESIAN_POINT ( 'NONE',  ( 86.75477599865929790, -25.38011337280982715, -14.88121679464376257 ) ) ;
#30263 = CARTESIAN_POINT ( 'NONE',  ( 123.0637881442452937, -8.899110576539710493, -16.42337572283490132 ) ) ;
#30264 = CARTESIAN_POINT ( 'NONE',  ( 119.7434548109119703, -2.686739459735783875, -18.49927484697928648 ) ) ;
#30265 = ORIENTED_EDGE ( 'NONE', *, *, #26611, .F. ) ;
#30266 = CARTESIAN_POINT ( 'NONE',  ( 123.4608748109119745, -10.63000616557722466, -14.87417383870573495 ) ) ;
#30267 = CARTESIAN_POINT ( 'NONE',  ( 118.6958348109119754, -6.344957434206665248, -7.627207830600338134 ) ) ;
#30268 = CARTESIAN_POINT ( 'NONE',  ( 114.7886608795247696, -1.325403438956436419, -16.93181055722141792 ) ) ;
#30269 = CARTESIAN_POINT ( 'NONE',  ( 113.1366214775786432, -7.643976991954077427, -18.09477374809248928 ) ) ;
#30270 = AXIS2_PLACEMENT_3D ( 'NONE', #3766, #4448, #32477 ) ;
#30271 = CARTESIAN_POINT ( 'NONE',  ( 112.6260814775786514, -9.261995988541697145, -16.69588392320189030 ) ) ;
#30272 = CARTESIAN_POINT ( 'NONE',  ( 122.9503348109119827, 0.5811942927096110934, -14.16772938898807510 ) ) ;
#30273 = CARTESIAN_POINT ( 'NONE',  ( 116.0388171295248014, -10.62599879583958540, -13.39321520033831447 ) ) ;
#30274 = CARTESIAN_POINT ( 'NONE',  ( 109.9963952545248134, -9.868328341294098749, -15.46607636864997204 ) ) ;
#30275 = CARTESIAN_POINT ( 'NONE',  ( 116.3860827545247787, -2.477300249445798297, -19.15521520033831138 ) ) ;
#30276 = CARTESIAN_POINT ( 'NONE',  ( 117.5045748109119756, -9.859900752359374465, -12.68260735090039404 ) ) ;
#30277 = CARTESIAN_POINT ( 'NONE',  ( 115.4624148109119943, -4.153390946401321671, -8.397313243818183892 ) ) ;
#30278 = CARTESIAN_POINT ( 'NONE',  ( 136.7911968929755062, -2.114665601771191561, -18.30335334318372276 ) ) ;
#30279 = CARTESIAN_POINT ( 'NONE',  ( 113.6079577545248043, -2.791137627527939813, -18.39754474579286025 ) ) ;
#30280 = EDGE_LOOP ( 'NONE', ( #17145, #44447, #37084, #30587 ) ) ;
#30281 = CARTESIAN_POINT ( 'NONE',  ( 109.2295991976226190, -0.1639994721771769748, -15.37948311923997657 ) ) ;
#30282 = CARTESIAN_POINT ( 'NONE',  ( 125.4463081442452932, -4.153390946401325223, -8.397313243818185668 ) ) ;
#30283 = CARTESIAN_POINT ( 'NONE',  ( 120.8547048109119686, -2.527210466738041728, -8.967976844669124148 ) ) ;
#30284 = CARTESIAN_POINT ( 'NONE',  ( 124.0495485609119584, -10.36940331770106916, -15.09355782777062061 ) ) ;
#30285 = ORIENTED_EDGE ( 'NONE', *, *, #44562, .F. ) ;
#30286 = DIRECTION ( 'NONE',  ( 5.948557404824750648E-16, 0.7876185884367599144, -0.6161630946014909904 ) ) ;
#30287 = CARTESIAN_POINT ( 'NONE',  ( 116.5974073229478876, -11.87839771549831624, -21.20499330233542068 ) ) ;
#30288 = ORIENTED_EDGE ( 'NONE', *, *, #36815, .F. ) ;
#30289 = CARTESIAN_POINT ( 'NONE',  ( 119.5467348109119712, -4.089484607189486809, -7.948022111789456723 ) ) ;
#30290 = CARTESIAN_POINT ( 'NONE',  ( 125.0492214775786266, -3.505236298600246325, -18.68346056562440793 ) ) ;
#30291 = CARTESIAN_POINT ( 'NONE',  ( 115.8027748109119841, -8.899110576539710493, -16.42337572283490132 ) ) ;
#30292 = PRESENTATION_STYLE_ASSIGNMENT (( #41255 ) ) ;
#30293 = DIRECTION ( 'NONE',  ( 0.000000000000000000, 0.000000000000000000, 1.000000000000000000 ) ) ;
#30294 = CARTESIAN_POINT ( 'NONE',  ( 120.2841814775786276, 0.9020085738987339008, -11.91225656197089222 ) ) ;
#30295 = CARTESIAN_POINT ( 'NONE',  ( 114.9518748109119883, -1.834011780172310813, -8.268836392978581529 ) ) ;
#30296 = CARTESIAN_POINT ( 'NONE',  ( 111.8716296295247901, -4.863998795839590272, -8.388885654883775800 ) ) ;
#30297 = CARTESIAN_POINT ( 'NONE',  ( 125.5030348109119558, -3.383040157471821630, -19.15922257007629170 ) ) ;
#30298 = DIRECTION ( 'NONE',  ( 0.5735764363510498232, -0.3127926500124802445, 0.7570804645221007600 ) ) ;
#30299 = EDGE_LOOP ( 'NONE', ( #16527, #2368, #9890, #33329 ) ) ;
#30300 = CARTESIAN_POINT ( 'NONE',  ( 119.5467348109119712, -4.089484607189486809, -7.948022111789456723 ) ) ;
#30301 = EDGE_CURVE ( 'NONE', #41818, #6998, #9757, .T. ) ;
#30302 = CARTESIAN_POINT ( 'NONE',  ( 113.0231681442453180, -10.15424416112533912, -14.75197769757731336 ) ) ;
#30303 = VECTOR ( 'NONE', #12766, 1000.000000000000227 ) ;
#30304 = CARTESIAN_POINT ( 'NONE',  ( 87.62389663665700823, -12.03403077406018440, -9.893215200338316251 ) ) ;
#30305 = CARTESIAN_POINT ( 'NONE',  ( 113.8173414775786512, 0.2603800115204892296, -16.42320221600525088 ) ) ;
#30306 = EDGE_LOOP ( 'NONE', ( #10777, #6479 ) ) ;
#30307 = CARTESIAN_POINT ( 'NONE',  ( 119.9438214775786378, -7.893985811506177619, -18.51759400769804742 ) ) ;
#30308 = CARTESIAN_POINT ( 'NONE',  ( 72.69189222814998175, -41.76310523276723785, -24.89321520033831447 ) ) ;
#30309 = CYLINDRICAL_SURFACE ( 'NONE', #37136, 1.587500000000000355 ) ;
#30310 = CARTESIAN_POINT ( 'NONE',  ( 79.79010115959992788, 5.106172230548759572, -14.64321520033831447 ) ) ;
#30311 = CARTESIAN_POINT ( 'NONE',  ( 115.8027748109119841, -8.899110576539710493, -16.42337572283490132 ) ) ;
#30312 = CARTESIAN_POINT ( 'NONE',  ( 136.7036351579039035, -2.784237195798857645, -8.139038447917522845 ) ) ;
#30313 = CARTESIAN_POINT ( 'NONE',  ( 119.3765548109119834, -10.15424416112533912, -14.75197769757731336 ) ) ;
#30314 = CARTESIAN_POINT ( 'NONE',  ( 72.54180985774836188, -58.79995985531765967, -35.99361511320584128 ) ) ;
#30315 = CARTESIAN_POINT ( 'NONE',  ( 125.4584548109119737, -2.316996251443989241, -21.63995271010855248 ) ) ;
#30316 = B_SPLINE_CURVE_WITH_KNOTS ( 'NONE', 3,
 ( #32415, #24912, #11908, #11235, #728, #39267, #39717, #35604, #4154, #29231 ),
 .UNSPECIFIED., .F., .F.,
 ( 4, 3, 3, 4 ),
 ( 0.000000000000000000, 0.0001671877548681280042, 0.0003343755096277710101, 0.0006463528481650629171 ),
 .UNSPECIFIED. ) ;
#30317 = CARTESIAN_POINT ( 'NONE',  ( 115.8595014775786609, -7.643976991954077427, -18.09477374809248928 ) ) ;
#30318 = CARTESIAN_POINT ( 'NONE',  ( 116.5402214775786405, 0.2603800115204892296, -16.42320221600525088 ) ) ;
#30319 = CARTESIAN_POINT ( 'NONE',  ( 120.2296266859119953, -0.06289925094097943703, -9.412459353600674206 ) ) ;
#30320 = CARTESIAN_POINT ( 'NONE',  ( 125.6732148109119862, -9.859900752359378018, -12.68260735090039759 ) ) ;
#30321 = CARTESIAN_POINT ( 'NONE',  ( 115.9729548109119861, -3.505236298600246325, -18.68346056562440793 ) ) ;
#30322 = CARTESIAN_POINT ( 'NONE',  ( 123.1772414775786189, -4.089484607189486809, -7.948022111789456723 ) ) ;
#30323 = CARTESIAN_POINT ( 'NONE',  ( 121.9859814775786333, 0.2603800115204892296, -16.42320221600525088 ) ) ;
#30324 = ORIENTED_EDGE ( 'NONE', *, *, #10023, .F. ) ;
#30325 = CARTESIAN_POINT ( 'NONE',  ( 113.0231681442453322, 0.9020085738987339008, -11.91225656197089222 ) ) ;
#30326 = CARTESIAN_POINT ( 'NONE',  ( 111.9410827545248708, -2.477300249445798297, -19.15521520033831138 ) ) ;
#30327 = ADVANCED_FACE ( 'NONE', ( #27984 ), #27050, .T. ) ;
#30328 = AXIS2_PLACEMENT_3D ( 'NONE', #24761, #367, #7884 ) ;
#30329 = CARTESIAN_POINT ( 'NONE',  ( 105.5513952545248060, -9.868328341294098749, -15.46607636864997204 ) ) ;
#30330 = CARTESIAN_POINT ( 'NONE',  ( 105.4819421295248247, -9.868328341294093420, -13.39321520033831447 ) ) ;
#30331 = CARTESIAN_POINT ( 'NONE',  ( 64.33426790211569823, -36.45104289022312827, -5.633705335131980796 ) ) ;
#30332 = CARTESIAN_POINT ( 'NONE',  ( 120.3409081442453044, -0.4660016031367893996, -10.09054647747474043 ) ) ;
#30333 = VERTEX_POINT ( 'NONE', #27535 ) ;
#30334 = CARTESIAN_POINT ( 'NONE',  ( 125.6732148109119862, 0.5811942927096110934, -14.16772938898807510 ) ) ;
#30335 = DIRECTION ( 'NONE',  ( 0.000000000000000000, 0.7996358532186282897, 0.6004852223388319477 ) ) ;
#30336 = CARTESIAN_POINT ( 'NONE',  ( 114.4413348109119823, -0.8288870151387760510, -10.36305467784173118 ) ) ;
#30337 = EDGE_CURVE ( 'NONE', #21796, #22202, #4442, .T. ) ;
#30338 = CARTESIAN_POINT ( 'NONE',  ( 124.7088614775786226, -9.565557343593420470, -10.61323700422348715 ) ) ;
#30339 = CIRCLE ( 'NONE', #35431, 2.000000000000000444 ) ;
#30340 = CARTESIAN_POINT ( 'NONE',  ( 120.5110881442453206, -6.344957434206665248, -7.627207830600338134 ) ) ;
#30341 = ADVANCED_FACE ( 'NONE', ( #27758 ), #1535, .T. ) ;
#30342 = CARTESIAN_POINT ( 'NONE',  ( 105.8986608795248401, -8.938348069036489818, -9.318865927141430916 ) ) ;
#30343 = CARTESIAN_POINT ( 'NONE',  ( 119.3046025628257070, -2.263366209404225504, -18.10533625161308180 ) ) ;
#30344 = ORIENTED_EDGE ( 'NONE', *, *, #38422, .F. ) ;
#30345 = CARTESIAN_POINT ( 'NONE',  ( 112.4559014775786494, -9.988377603198976828, -10.36322818467138340 ) ) ;
#30346 = CARTESIAN_POINT ( 'NONE',  ( 122.0994348109119443, -10.15424416112533912, -14.75197769757731336 ) ) ;
#30347 = CARTESIAN_POINT ( 'NONE',  ( 118.0718414775786300, -9.261995988541697145, -16.69588392320189030 ) ) ;
#30348 = CARTESIAN_POINT ( 'NONE',  ( 113.1366214775786432, -7.643976991954077427, -18.09477374809248928 ) ) ;
#30349 = CARTESIAN_POINT ( 'NONE',  ( 114.2711548109119803, -9.988377603198976828, -10.36322818467138340 ) ) ;
#30350 = DIRECTION ( 'NONE',  ( 0.000000000000000000, 0.6004852223388321697, -0.7996358532186279566 ) ) ;
#30351 = CARTESIAN_POINT ( 'NONE',  ( 125.7299414775786346, -10.15424416112533912, -14.75197769757731336 ) ) ;
#30352 = CARTESIAN_POINT ( 'NONE',  ( 118.1852948109119836, -4.153390946401325223, -8.397313243818185668 ) ) ;
#30353 = ORIENTED_EDGE ( 'NONE', *, *, #17211, .T. ) ;
#30354 = ADVANCED_FACE ( 'NONE', ( #20470 ), #7002, .T. ) ;
#30355 = CARTESIAN_POINT ( 'NONE',  ( 121.6881423109119709, -9.959231468620755479, -10.70263013195267199 ) ) ;
#30356 = VECTOR ( 'NONE', #12123, 1000.000000000000000 ) ;
#30357 = CARTESIAN_POINT ( 'NONE',  ( 112.0020881442453344, 0.2603800115204892296, -16.42320221600525088 ) ) ;
#30358 = CARTESIAN_POINT ( 'NONE',  ( 122.0427081442452817, -9.859900752359378018, -12.68260735090039759 ) ) ;
#30359 = ORIENTED_EDGE ( 'NONE', *, *, #23670, .T. ) ;
#30360 = EDGE_CURVE ( 'NONE', #8497, #39217, #44414, .T. ) ;
#30361 = CARTESIAN_POINT ( 'NONE',  ( 121.0630641859119976, -8.321307733199551748, -9.223433127585318303 ) ) ;
#30362 = EDGE_CURVE ( 'NONE', #44507, #34894, #2984, .T. ) ;
#30363 = ADVANCED_FACE ( 'NONE', ( #37556 ), #29249, .T. ) ;
#30364 = CARTESIAN_POINT ( 'NONE',  ( 119.8303681442453126, -10.63000616557722466, -14.87417383870573495 ) ) ;
#30365 = CARTESIAN_POINT ( 'NONE',  ( 113.1912390045248031, 0.8980012041604421569, -15.77991374673208469 ) ) ;
#30366 = CARTESIAN_POINT ( 'NONE',  ( 116.3700414775786527, -4.153390946401321671, -8.397313243818183892 ) ) ;
#30367 = ORIENTED_EDGE ( 'NONE', *, *, #43498, .F. ) ;
#30368 = ORIENTED_EDGE ( 'NONE', *, *, #36779, .T. ) ;
#30369 = CARTESIAN_POINT ( 'NONE',  ( 112.3991748109119868, -8.166667518702817929, -8.995218007635859436 ) ) ;
#30370 = B_SPLINE_CURVE_WITH_KNOTS ( 'NONE', 3,
 ( #30557, #44478, #2282, #5702, #20531, #23043, #2966, #40376, #33503, #41068 ),
 .UNSPECIFIED., .F., .F.,
 ( 4, 3, 3, 4 ),
 ( 0.000000000000000000, 0.0001671877548681309858, 0.0003343755096277739917, 0.0006463528481650629171 ),
 .UNSPECIFIED. ) ;
#30371 = CARTESIAN_POINT ( 'NONE',  ( 121.3052614775786111, -7.643976991954077427, -18.09477374809248928 ) ) ;
#30372 = CARTESIAN_POINT ( 'NONE',  ( 135.3184548109119874, 0.6402711692277546218, -15.78131322003127579 ) ) ;
#30373 = CARTESIAN_POINT ( 'NONE',  ( 62.44280897409132791, -35.50444474346354440, -5.893215200338310922 ) ) ;
#30374 = CARTESIAN_POINT ( 'NONE',  ( 119.6601881442453106, -8.166667518702819706, -8.995218007635861213 ) ) ;
#30375 = CARTESIAN_POINT ( 'NONE',  ( 105.5513952545248060, 0.8980012041604421569, -11.00651665394454071 ) ) ;
#30376 = CARTESIAN_POINT ( 'NONE',  ( 120.5678148109119832, -8.166667518702819706, -8.995218007635861213 ) ) ;
#30378 = CARTESIAN_POINT ( 'NONE',  ( 119.6601881442453106, -1.833838273342659253, -17.42832698103878286 ) ) ;
#30377 = CARTESIAN_POINT ( 'NONE',  ( 114.7249681442453237, 0.2603800115204892296, -16.42320221600525088 ) ) ;
#30379 = CARTESIAN_POINT ( 'NONE',  ( 125.3328548109119964, -0.8288870151387760510, -10.36305467784173118 ) ) ;
#30380 = LINE ( 'NONE', #37196, #7273 ) ;
#30381 = ORIENTED_EDGE ( 'NONE', *, *, #20585, .F. ) ;
#30382 = CARTESIAN_POINT ( 'NONE',  ( 122.0427081442452817, -9.859900752359378018, -12.68260735090039759 ) ) ;
#30383 = CARTESIAN_POINT ( 'NONE',  ( 126.2184548109119788, -4.863998795839242995, -13.39321520033831447 ) ) ;
#30384 = CARTESIAN_POINT ( 'NONE',  ( 121.0067200565388958, -8.485573535863895955, -17.53172993199661178 ) ) ;
#30385 = CARTESIAN_POINT ( 'NONE',  ( 110.3436608795247764, -8.938348069036489818, -9.318865927141430916 ) ) ;
#30386 = CARTESIAN_POINT ( 'NONE',  ( 112.0799890045248475, -9.868328341294098749, -11.32035403202665869 ) ) ;
#30387 = CARTESIAN_POINT ( 'NONE',  ( 107.7044421295247929, 0.8980012041604618078, -13.39321520033831447 ) ) ;
#30388 = VECTOR ( 'NONE', #11468, 1000.000000000000000 ) ;
#30389 = CARTESIAN_POINT ( 'NONE',  ( 123.3474214775786209, -9.988377603198976828, -10.36322818467138340 ) ) ;
#30390 = CARTESIAN_POINT ( 'NONE',  ( 124.6521348109119884, -7.894159318335828068, -9.358103419637847864 ) ) ;
#30391 = EDGE_LOOP ( 'NONE', ( #6434, #42080, #22118, #34276 ) ) ;
#30392 = CARTESIAN_POINT ( 'NONE',  ( 123.5743281442453139, -7.893985811506177619, -18.51759400769804742 ) ) ;
#30393 = CARTESIAN_POINT ( 'NONE',  ( 112.1722681442453222, -8.899110576539710493, -16.42337572283490132 ) ) ;
#30394 = CARTESIAN_POINT ( 'NONE',  ( 61.27778620743471549, -25.99489077589588604, -13.39321520033831447 ) ) ;
#30395 = CARTESIAN_POINT ( 'NONE',  ( 118.3554748109119998, 0.2603800115204892296, -16.42320221600525088 ) ) ;
#30396 = CARTESIAN_POINT ( 'NONE',  ( 122.8368814775786291, -1.561330072975668948, -17.79121239304076951 ) ) ;
#30397 = CARTESIAN_POINT ( 'NONE',  ( 111.2184548109119788, -8.862178061932382889, -16.39564131203247399 ) ) ;
#30398 = CARTESIAN_POINT ( 'NONE',  ( 123.5743281442453139, -2.084020599724406786, -8.691656652584148546 ) ) ;
#30399 = CARTESIAN_POINT ( 'NONE',  ( 124.9069617844024975, -8.274459215933877232, -17.13193711621141802 ) ) ;
#30400 = LINE ( 'NONE', #41359, #32795 ) ;
#30401 = ORIENTED_EDGE ( 'NONE', *, *, #12622, .T. ) ;
#30402 = CARTESIAN_POINT ( 'NONE',  ( -3.075987277002964593, -7.207016596002466358, -7.393215200338315363 ) ) ;
#30403 = DIRECTION ( 'NONE',  ( 0.000000000000000000, -0.9242245927363029745, -0.3818493186865925537 ) ) ;
#30404 = CARTESIAN_POINT ( 'NONE',  ( 123.8012348109119642, -9.565557343593413364, -10.61323700422348004 ) ) ;
#30405 = CARTESIAN_POINT ( 'NONE',  ( 106.6626452545248611, -9.868328341294098749, -15.46607636864997204 ) ) ;
#30406 = CARTESIAN_POINT ( 'NONE',  ( 109.9269421295247753, -9.868328341294093420, -13.39321520033831447 ) ) ;
#30407 = CARTESIAN_POINT ( 'NONE',  ( 118.9227414775786542, 0.4262465694468514643, -12.03445270309931736 ) ) ;
#30408 = CARTESIAN_POINT ( 'NONE',  ( 69.79880589660244539, -25.73400820227583807, -5.787280954910595909 ) ) ;
#30409 = CARTESIAN_POINT ( 'NONE',  ( 117.5045748109119756, -9.859900752359374465, -12.68260735090039404 ) ) ;
#30410 = CARTESIAN_POINT ( 'NONE',  ( 123.4608748109119745, -10.63000616557722466, -14.87417383870573495 ) ) ;
#30411 = VERTEX_POINT ( 'NONE', #16829 ) ;
#30412 = AXIS2_PLACEMENT_3D ( 'NONE', #29086, #36363, #19051 ) ;
#30413 = CARTESIAN_POINT ( 'NONE',  ( 123.8579614775786126, -9.859900752359378018, -12.68260735090039759 ) ) ;
#30414 = CARTESIAN_POINT ( 'NONE',  ( 118.7525614775786380, -8.166667518702819706, -8.995218007635861213 ) ) ;
#30415 = CARTESIAN_POINT ( 'NONE',  ( 124.9357681442453014, -1.834011780172310813, -8.268836392978581529 ) ) ;
#30416 = CARTESIAN_POINT ( 'NONE',  ( 125.0492214775786266, -3.505236298600246325, -18.68346056562440793 ) ) ;
#30417 = VERTEX_POINT ( 'NONE', #3354 ) ;
#30418 = DIRECTION ( 'NONE',  ( -1.000000000000000000, 0.000000000000000000, 3.317300593186674996E-33 ) ) ;
#30419 = CARTESIAN_POINT ( 'NONE',  ( 125.3895814775786448, -7.893985811506177619, -18.51759400769804742 ) ) ;
#30420 = CARTESIAN_POINT ( 'NONE',  ( 113.1933481442453058, -5.574606645277164318, -18.38911715685844683 ) ) ;
#30421 = VECTOR ( 'NONE', #41382, 1000.000000000000227 ) ;
#30422 = CARTESIAN_POINT ( 'NONE',  ( 123.5743281442453139, -7.893985811506177619, -18.51759400769804742 ) ) ;
#30423 = ADVANCED_FACE ( 'NONE', ( #30722 ), #34012, .T. ) ;
#30424 = CARTESIAN_POINT ( 'NONE',  ( 108.8156921295247912, 0.8980012041604618078, -13.39321520033831447 ) ) ;
#30425 = CARTESIAN_POINT ( 'NONE',  ( 122.9382985609119743, -0.08252387247370887580, -11.91645802438286417 ) ) ;
#30426 = ORIENTED_EDGE ( 'NONE', *, *, #23727, .T. ) ;
#30427 = CARTESIAN_POINT ( 'NONE',  ( 27.57768543387103222, -14.97172645945875935, -17.89321520033831447 ) ) ;
#30428 = CARTESIAN_POINT ( 'NONE',  ( 107.4266296295248821, -4.863998795839590272, -8.388885654883775800 ) ) ;
#30429 = CARTESIAN_POINT ( 'NONE',  ( 72.54180985774836188, -61.58539327607277869, -37.10777877198333385 ) ) ;
#30430 = CARTESIAN_POINT ( 'NONE',  ( 119.0361948109119652, -2.084020599724406786, -8.691656652584148546 ) ) ;
#30431 = CARTESIAN_POINT ( 'NONE',  ( 112.4559014775786778, -0.1624402480850797581, -16.17319339645315424 ) ) ;
#30432 = CARTESIAN_POINT ( 'NONE',  ( 125.2761281442452912, 0.4262465694468504651, -12.03445270309929604 ) ) ;
#30433 = EDGE_LOOP ( 'NONE', ( #43146, #21991, #31909, #1228 ) ) ;
#30434 = CARTESIAN_POINT ( 'NONE',  ( 88.73939138327467901, -26.60966817898065884, -11.90521360603286816 ) ) ;
#30435 = CARTESIAN_POINT ( 'NONE',  ( 120.1707281442453166, -9.565557343593413364, -10.61323700422348004 ) ) ;
#30436 = CARTESIAN_POINT ( 'NONE',  ( 116.5080644685026812, 0.6938714319018670640, -14.64321520033829671 ) ) ;
#30437 = CARTESIAN_POINT ( 'NONE',  ( 67.90958954586700713, -0.5136061671847661492, -10.39321520033831625 ) ) ;
#30438 = CARTESIAN_POINT ( 'NONE',  ( 111.8886348109120092, -6.222761293078241884, -8.102969835052219238 ) ) ;
#30440 = CARTESIAN_POINT ( 'NONE',  ( 123.4608748109119745, -10.63000616557722466, -14.87417383870573495 ) ) ;
#30439 = CARTESIAN_POINT ( 'NONE',  ( 68.07789357685331311, -68.58957386525776201, -38.44539312525988350 ) ) ;
#30441 = CARTESIAN_POINT ( 'NONE',  ( 112.1155414775786454, 0.9020085738987339008, -11.91225656197089222 ) ) ;
#30442 = ORIENTED_EDGE ( 'NONE', *, *, #7480, .T. ) ;
#30443 = CARTESIAN_POINT ( 'NONE',  ( 113.7038881442453402, -3.383040157471821630, -19.15922257007629170 ) ) ;
#30444 = CARTESIAN_POINT ( 'NONE',  ( 113.6623870589982346, -1.063912429576153063, -17.20460841810474761 ) ) ;
#30445 = CARTESIAN_POINT ( 'NONE',  ( 114.9275671295247889, -10.62599879583958540, -13.39321520033831447 ) ) ;
#30446 = CARTESIAN_POINT ( 'NONE',  ( 124.5386814775786206, -4.153390946401325223, -8.397313243818185668 ) ) ;
#30447 = CARTESIAN_POINT ( 'NONE',  ( 120.9081748109119872, -4.153390946401325223, -8.397313243818185668 ) ) ;
#30448 = DIRECTION ( 'NONE',  ( 0.000000000000000000, 0.000000000000000000, -1.000000000000000000 ) ) ;
#30449 = CARTESIAN_POINT ( 'NONE',  ( 113.1912390045248031, -9.868328341294098749, -11.32035403202665869 ) ) ;
#30450 = DIRECTION ( 'NONE',  ( 1.000000000000000000, 0.000000000000000000, -0.000000000000000000 ) ) ;
#30451 = CARTESIAN_POINT ( 'NONE',  ( 88.46631044337289040, -25.23119213852205789, -15.24166438581092109 ) ) ;
#30452 = CARTESIAN_POINT ( 'NONE',  ( 113.6471614775786492, -4.153390946401321671, -8.397313243818183892 ) ) ;
#30453 = CARTESIAN_POINT ( 'NONE',  ( 109.6491296295247793, -4.863998795839590272, -19.15521520033831493 ) ) ;
#30454 = CARTESIAN_POINT ( 'NONE',  ( 125.4584548109119737, -4.863998795839242995, -13.39321520033831447 ) ) ;
#30455 = CARTESIAN_POINT ( 'NONE',  ( 114.9275671295247889, -10.62599879583958540, -13.39321520033831447 ) ) ;
#30456 = CARTESIAN_POINT ( 'NONE',  ( 124.5386814775786206, -5.638512984488999180, -18.83840828888717311 ) ) ;
#30457 = CARTESIAN_POINT ( 'NONE',  ( 123.4041481442452834, -10.30919188438810075, -12.61870101168855918 ) ) ;
#30458 = DIRECTION ( 'NONE',  ( 0.1352586133457950590, 0.9908103287288504424, 0.000000000000000000 ) ) ;
#30459 = CARTESIAN_POINT ( 'NONE',  ( 121.8725281442453223, -3.383040157471821630, -19.15922257007629170 ) ) ;
#30460 = CARTESIAN_POINT ( 'NONE',  ( 112.7395348109119766, -5.638512984488999180, -18.83840828888717311 ) ) ;
#30461 = VERTEX_POINT ( 'NONE', #12167 ) ;
#30462 = CARTESIAN_POINT ( 'NONE',  ( 115.0086014775786509, -5.574606645277164318, -18.38911715685844683 ) ) ;
#30463 = CARTESIAN_POINT ( 'NONE',  ( 125.7299414775786346, 0.9020085738987339008, -11.91225656197089222 ) ) ;
#30464 = CARTESIAN_POINT ( 'NONE',  ( 122.4397948109119767, -9.988377603198976828, -10.36322818467138340 ) ) ;
#30465 = CARTESIAN_POINT ( 'NONE',  ( 114.2144281442453178, -8.166667518702817929, -8.995218007635859436 ) ) ;
#30466 = CARTESIAN_POINT ( 'NONE',  ( 113.3068014775786594, -1.833838273342658809, -17.42832698103878286 ) ) ;
#30467 = ORIENTED_EDGE ( 'NONE', *, *, #31477, .F. ) ;
#30468 = CARTESIAN_POINT ( 'NONE',  ( 116.9373081442452929, -1.833838273342659253, -17.42832698103878286 ) ) ;
#30469 = CARTESIAN_POINT ( 'NONE',  ( 105.8292077545248446, -7.250697342233347165, -7.631215200338321125 ) ) ;
#30470 = CARTESIAN_POINT ( 'NONE',  ( 110.4131140045248287, 0.1403307496149616695, -15.46607636864997204 ) ) ;
#30471 = EDGE_CURVE ( 'NONE', #36514, #37423, #123, .T. ) ;
#30472 = CARTESIAN_POINT ( 'NONE',  ( 123.9714148109119805, -8.899110576539710493, -16.42337572283490132 ) ) ;
#30473 = CARTESIAN_POINT ( 'NONE',  ( 124.1916298109119765, -2.529232162390850913, -8.971805383624186447 ) ) ;
#30474 = CARTESIAN_POINT ( 'NONE',  ( 113.3995983795247895, -0.7896495226426338832, -9.318865927141430916 ) ) ;
#30475 = ORIENTED_EDGE ( 'NONE', *, *, #22817, .F. ) ;
#30476 = DIRECTION ( 'NONE',  ( 0.000000000000000000, 0.6004852223388321697, -0.7996358532186279566 ) ) ;
#30477 = CARTESIAN_POINT ( 'NONE',  ( 126.1270281442452870, -10.30919188438810075, -12.61870101168855918 ) ) ;
#30478 = DIRECTION ( 'NONE',  ( 0.4649787261689617424, 0.8853218534579895271, 0.000000000000000000 ) ) ;
#30479 = CARTESIAN_POINT ( 'NONE',  ( 112.5693548109119888, -10.63000616557722466, -14.87417383870573495 ) ) ;
#30480 = CARTESIAN_POINT ( 'NONE',  ( 122.3826735609119680, 0.6414057260225851653, -11.69287257290601723 ) ) ;
#30481 = CARTESIAN_POINT ( 'NONE',  ( 113.8627504229301763, 0.1075849324168598464, -14.64321520033831447 ) ) ;
#30482 = CARTESIAN_POINT ( 'NONE',  ( 106.0375671295248310, 0.1403307496149613920, -13.39321520033831447 ) ) ;
#30483 = CARTESIAN_POINT ( 'NONE',  ( 115.4385020163423263, -1.087735405160632718, -17.17288456429612253 ) ) ;
#30484 = CARTESIAN_POINT ( 'NONE',  ( 118.5823814775786360, -1.834011780172310813, -8.268836392978581529 ) ) ;
#30485 = CARTESIAN_POINT ( 'NONE',  ( 88.35093386163799778, -25.99489077589524300, -13.39321520033831447 ) ) ;
#30486 = FACE_OUTER_BOUND ( 'NONE', #27332, .T. ) ;
#30487 = EDGE_CURVE ( 'NONE', #1042, #10767, #43399, .T. ) ;
#30488 = CARTESIAN_POINT ( 'NONE',  ( 123.7717360609119766, -3.387241619883525789, -18.17469012370376191 ) ) ;
#30489 = CARTESIAN_POINT ( 'NONE',  ( 121.3052614775786111, -7.643976991954077427, -18.09477374809248928 ) ) ;
#30490 = CARTESIAN_POINT ( 'NONE',  ( 119.7434548109119703, -0.05003288430990287389, -11.46608162719201829 ) ) ;
#30491 = VERTEX_POINT ( 'NONE', #16494 ) ;
#30492 = CARTESIAN_POINT ( 'NONE',  ( 123.7445081442452874, -1.561330072975668948, -17.79121239304076951 ) ) ;
#30493 = CARTESIAN_POINT ( 'NONE',  ( 120.9649014775786355, -3.383040157471821630, -19.15922257007629170 ) ) ;
#30494 = DIRECTION ( 'NONE',  ( 0.9659258262890689783, 0.2588190451025185190, 0.000000000000000000 ) ) ;
#30495 = CARTESIAN_POINT ( 'NONE',  ( 112.7962614775786676, -6.222761293078241884, -8.102969835052219238 ) ) ;
#30496 = CARTESIAN_POINT ( 'NONE',  ( 123.3474214775786209, -9.988377603198976828, -10.36322818467138340 ) ) ;
#30497 = CARTESIAN_POINT ( 'NONE',  ( 110.1353015045248469, -2.477300249445798297, -7.631215200338321125 ) ) ;
#30498 = DIRECTION ( 'NONE',  ( 0.000000000000000000, -0.9242245927363040847, -0.3818493186865897226 ) ) ;
#30499 = CARTESIAN_POINT ( 'NONE',  ( 124.9868051361382868, -12.36944789948101331, -14.53642012793133986 ) ) ;
#30500 = CARTESIAN_POINT ( 'NONE',  ( 117.3911214775786505, -7.894159318335828068, -9.358103419637847864 ) ) ;
#30501 = CARTESIAN_POINT ( 'NONE',  ( 118.2987481442453088, -7.894159318335828068, -9.358103419637847864 ) ) ;
#30502 = LINE ( 'NONE', #22986, #18956 ) ;
#30503 = CARTESIAN_POINT ( 'NONE',  ( 112.7745202545247878, 0.1403307496149616695, -11.32035403202665336 ) ) ;
#30504 = VERTEX_POINT ( 'NONE', #36982 ) ;
#30505 = CARTESIAN_POINT ( 'NONE',  ( 109.2294421145928567, -0.5977367109841295045, -16.12358707770981425 ) ) ;
#30506 = CARTESIAN_POINT ( 'NONE',  ( 114.3278814775786429, -10.30919188438810075, -12.61870101168855918 ) ) ;
#30507 = DIRECTION ( 'NONE',  ( -0.9908103287288504424, 0.1352586133457950313, 0.000000000000000000 ) ) ;
#30508 = CARTESIAN_POINT ( 'NONE',  ( 119.6045485609119794, -0.08252387247370887580, -11.91645802438286417 ) ) ;
#30509 = CARTESIAN_POINT ( 'NONE',  ( 122.4521266859119635, -9.033780868592240054, -16.85052413769862056 ) ) ;
#30510 = ORIENTED_EDGE ( 'NONE', *, *, #22620, .T. ) ;
#30511 = DIRECTION ( 'NONE',  ( 0.9908103287288504424, -0.1352586133457950590, 0.000000000000000000 ) ) ;
#30512 = CARTESIAN_POINT ( 'NONE',  ( 87.02785693856107230, -25.99489077589524300, -13.39321520033831447 ) ) ;
#30513 = VERTEX_POINT ( 'NONE', #3245 ) ;
#30514 = CARTESIAN_POINT ( 'NONE',  ( 116.7671281442453335, -1.834011780172310813, -8.268836392978581529 ) ) ;
#30515 = CARTESIAN_POINT ( 'NONE',  ( 122.7801548109119665, -6.222761293078241884, -8.102969835052219238 ) ) ;
#30516 = AXIS2_PLACEMENT_3D ( 'NONE', #8809, #12468, #25918 ) ;
#30517 = CARTESIAN_POINT ( 'NONE',  ( 119.7736414775786358, 0.1319031606808879209, -14.10382304977623669 ) ) ;
#30518 =( LENGTH_UNIT ( ) NAMED_UNIT ( * ) SI_UNIT ( .MILLI., .METRE. ) );
#30519 = DIRECTION ( 'NONE',  ( 0.000000000000000000, 0.000000000000000000, 1.000000000000000000 ) ) ;
#30520 = CARTESIAN_POINT ( 'NONE',  ( 121.8725281442453223, -3.383040157471821630, -19.15922257007629170 ) ) ;
#30521 = CARTESIAN_POINT ( 'NONE',  ( 118.8660148109119774, -10.30919188438810075, -12.61870101168855918 ) ) ;
#30522 = CARTESIAN_POINT ( 'NONE',  ( 113.6774108795247997, -1.325403438956436419, -16.93181055722141792 ) ) ;
#30523 = CARTESIAN_POINT ( 'NONE',  ( 113.9307948109119764, -10.15424416112533912, -14.75197769757731336 ) ) ;
#30524 = DIRECTION ( 'NONE',  ( 1.000000000000000000, 0.000000000000000000, -0.000000000000000000 ) ) ;
#30525 = VERTEX_POINT ( 'NONE', #37211 ) ;
#30526 = CARTESIAN_POINT ( 'NONE',  ( 117.0507614775786465, -10.30919188438810075, -12.61870101168855918 ) ) ;
#30527 = CARTESIAN_POINT ( 'NONE',  ( 114.7249681442453237, -9.565557343593413364, -10.61323700422348004 ) ) ;
#30528 = FACE_OUTER_BOUND ( 'NONE', #20324, .T. ) ;
#30529 = CARTESIAN_POINT ( 'NONE',  ( 112.4559014775786494, -9.988377603198976828, -10.36322818467138340 ) ) ;
#30530 = ORIENTED_EDGE ( 'NONE', *, *, #4240, .T. ) ;
#30531 = CARTESIAN_POINT ( 'NONE',  ( 121.5888948109119809, -10.30919188438810075, -12.61870101168855918 ) ) ;
#30532 = CARTESIAN_POINT ( 'NONE',  ( 138.2184548109119930, 0.7167481258041168424, -11.18974888642104659 ) ) ;
#30533 = CARTESIAN_POINT ( 'NONE',  ( 112.7962614775786676, -6.222761293078241884, -8.102969835052219238 ) ) ;
#30534 = CARTESIAN_POINT ( 'NONE',  ( 66.50565249108366572, -35.53029877516337365, -7.393215200338315363 ) ) ;
#30535 = CARTESIAN_POINT ( 'NONE',  ( 114.5547881442453217, -4.153390946401321671, -8.397313243818183892 ) ) ;
#30536 = CARTESIAN_POINT ( 'NONE',  ( 123.5807492164245360, -4.317385761257377830, -15.37007627435306389 ) ) ;
#30537 = CARTESIAN_POINT ( 'NONE',  ( 117.6180281442453150, -8.899110576539710493, -16.42337572283490132 ) ) ;
#30538 = CIRCLE ( 'NONE', #15999, 6.479565957685756494 ) ;
#30539 = DIRECTION ( 'NONE',  ( 0.000000000000000000, 0.9284778069183720062, 0.3713878862591650232 ) ) ;
#30540 = CARTESIAN_POINT ( 'NONE',  ( 114.0442481442453300, -7.643976991954077427, -18.09477374809248928 ) ) ;
#30541 = CARTESIAN_POINT ( 'NONE',  ( 115.1220548109119761, -8.166667518702817929, -8.995218007635861213 ) ) ;
#30542 = CARTESIAN_POINT ( 'NONE',  ( 121.8965016859119856, -0.6942167230862511529, -9.935906262978006609 ) ) ;
#30543 = VECTOR ( 'NONE', #14910, 1000.000000000000000 ) ;
#30544 = CARTESIAN_POINT ( 'NONE',  ( 112.2857214775786474, -4.089484607189486809, -7.948022111789456723 ) ) ;
#30545 = CARTESIAN_POINT ( 'NONE',  ( 114.8951481442453115, -8.899110576539710493, -16.42337572283490132 ) ) ;
#30546 = CARTESIAN_POINT ( 'NONE',  ( 123.4041481442452834, -10.30919188438810075, -12.61870101168855918 ) ) ;
#30547 = CARTESIAN_POINT ( 'NONE',  ( 115.8595014775786609, -7.643976991954077427, -18.09477374809248928 ) ) ;
#30548 = ORIENTED_EDGE ( 'NONE', *, *, #42966, .F. ) ;
#30549 = CARTESIAN_POINT ( 'NONE',  ( 112.4559014775786494, -9.988377603198976828, -10.36322818467138340 ) ) ;
#30550 = CARTESIAN_POINT ( 'NONE',  ( 105.6903015045248253, -2.477300249445798297, -7.631215200338321125 ) ) ;
#30551 = CARTESIAN_POINT ( 'NONE',  ( 107.4266296295248821, -4.863998795839590272, -8.388885654883775800 ) ) ;
#30552 = CARTESIAN_POINT ( 'NONE',  ( 67.30914723170953096, -55.09414448979863010, -36.13498279219247422 ) ) ;
#30553 = CARTESIAN_POINT ( 'NONE',  ( 109.3018640045248304, -10.62599879583958540, -11.00651665394454071 ) ) ;
#30554 = CARTESIAN_POINT ( 'NONE',  ( 117.3343948109119737, -3.383040157471821630, -19.15922257007629170 ) ) ;
#30555 = ORIENTED_EDGE ( 'NONE', *, *, #40924, .T. ) ;
#30556 = CARTESIAN_POINT ( 'NONE',  ( 88.93653725331050452, -10.83229915613791761, -18.64321520033831803 ) ) ;
#30557 = CARTESIAN_POINT ( 'NONE',  ( 120.5468302440515203, -2.467220198592778413, -17.83387418641524391 ) ) ;
#30558 = CARTESIAN_POINT ( 'NONE',  ( 116.7671281442453335, -7.643976991954077427, -18.09477374809248928 ) ) ;
#30559 =( BOUNDED_SURFACE ( )  B_SPLINE_SURFACE ( 1, 2, ( 
 ( #37750, #26591, #17019, #44608, #37518, #44833, #12922, #43923, #16565, #26818, #30689, #6520, #44157, #40730, #33863, #22937, #6290, #20211, #30460, #13372, #19745, #41191, #19975, #13143, #5825, #30235, #9265, #9486, #27276, #20435, #34319, #36830, #27046, #3093, #40504, #30911, #23400, #37285, #5600, #6054, #37054, #2633, #9718, #33400, #2174, #40964, #23632, #33631, #2405, #18122, #10395, #20876, #20660, #38407, #3753, #42079, #14477, #21541, #35201, #34536, #14033, #17675, #17237, #6750, #3536, #17451, #10618, #24520, #3315, #31571, #14253, #28170, #3976, #38859, #7178, #17898, #340, #10838, #34965, #45053, #24734, #41857, #38623, #27947, #32017, #21317, #42298, #13590, #11061, #24305, #27500, #7399, #31795, #4204, #31129, #41420, #10175, #13813, #24081, #21088, #24963, #567, #28386, #7627, #35428, #37974, #27724, #41640, #38192, #31346, #120, #6968, #34753, #18796, #43195, #8754, #32685, #4878, #19245, #25859, #1676, #8088, #36555, #35880, #8310, #15599, #36107, #11732, #25419, #22436, #8534, #39988, #28616, #1455, #5329, #780, #36329, #4650, #5099, #19014, #18350, #18572, #32464, #32900, #21990, #15375, #22211, #1013, #11286, #29279, #35661, #21767, #32242, #14929, #4433, #28840, #42751, #11515, #1239, #39764, #29502, #43417, #14702, #11960, #12183, #39320, #26084, #15151, #29057, #22659, #42965, #25645, #42525, #25194, #39092, #7861, #39548, #6001, #26769, #9899, #37699, #29957, #40450, #40220, #12869, #23343, #16511, #34043, #41139, #9663, #8985, #33577, #37227, #36777, #26312, #23121, #36998, #30186, #44104, #22883, #19924, #33810, #2581, #23582, #13315, #40679, #37465, #30410, #44331, #9430, #19465, #13091, #16284, #26989, #2352, #6471, #40909, #16740, #33128, #30635, #43872, #1897, #6238, #20160, #23811, #5548, #15825, #29724, #33348, #43638, #2811, #44551, #27222, #12412, #2122, #16051, #12644, #26540, #9212, #5769, #19690, #24249, #31076, #38569, #38353, #17623, #28331, #7129, #24461, #38803, #288, #21264, #27672, #11008, #10344, #27893, #35145 ),
 ( #31741, #6913, #17404, #3924, #45003, #41370, #42021, #17186, #34268, #21040, #3042, #10785, #31293, #10126, #17844, #67, #24907, #20382, #13979, #13763, #24682, #28116, #14421, #16964, #10565, #30858, #44781, #7347, #38141, #510, #42243, #37920, #20822, #34701, #13540, #41587, #34913, #41807, #20607, #27448, #3704, #24030, #6696, #34482, #3261, #3488, #31516, #14199, #22382, #36278, #21486, #42915, #5045, #21713, #18960, #21932, #42692, #32850, #35824, #42469, #29006, #36053, #35371, #29226, #1183, #25586, #15097, #29445, #12129, #4372, #14874, #14647, #32410, #11677, #4820, #8478, #15540, #43133, #28562, #8025, #39488, #11232, #724, #11461, #25365, #4598, #18519, #25140, #8253, #22159, #18743, #11903, #1619, #32634, #25804, #1400, #15316, #39714, #39034, #43360, #26032, #7573, #4149, #18067, #31958, #7805, #35600, #18291, #32186, #958, #28786, #39261, #30573, #33069, #44493, #8698, #1841, #22603, #23060, #23523, #26710, #30131, #30352, #9607, #9154, #2525, #40392, #37410, #12583, #43818, #5490, #13032, #12808, #37170, #2754, #40620, #44044, #13258, #19868, #40852, #2073, #39937, #29902, #2298, #6180, #9377, #16452, #20100, #33985, #23286, #36946, #26488, #5716, #19634, #16679, #5945, #12355, #26930, #36503, #33518, #16227, #5272, #19410, #15770, #44277, #36721, #19190, #33757, #29673, #43585, #26255, #40165, #8927, #22829, #33297, #15996, #10286, #3207, #11, #38514, #13486, #38082, #41312, #7291, #10507, #24632, #35086, #20323, #44726, #34646, #34207, #30801, #21208, #10072, #37859, #17350, #24408, #23973, #24191, #27832, #3432, #6860, #10733, #27388, #17788, #228, #38297, #451, #13708, #6635, #31240, #27615, #31460, #3866, #44949, #41528, #13923, #23751, #7076, #20986, #41743, #34859, #20547, #41966, #20767, #3647, #34426, #17132, #6415, #31682, #27162, #16909, #41084, #31019, #17566, #14142, #28057, #9840, #37641, #2981, #4767, #42190, #14367, #11849, #18904, #25531, #25082, #21431, #32793, #32358, #21654, #24853, #673, #22329, #7743, #28281, #10950 ) ),
 .UNSPECIFIED., .F., .F., .F. ) 
 B_SPLINE_SURFACE_WITH_KNOTS ( ( 2, 2 ),
 ( 3, 2, 2, 2, 2, 2, 2, 2, 2, 2, 2, 2, 2, 2, 2, 2, 2, 2, 2, 2, 2, 2, 2, 2, 2, 2, 2, 2, 2, 2, 2, 2, 2, 2, 2, 2, 2, 2, 2, 2, 2, 2, 2, 2, 2, 2, 2, 2, 2, 2, 2, 2, 2, 2, 2, 2, 2, 2, 2, 2, 2, 2, 2, 2, 2, 2, 2, 2, 2, 2, 2, 2, 2, 2, 2, 2, 2, 2, 2, 2, 2, 2, 2, 2, 2, 2, 2, 2, 2, 2, 2, 2, 2, 2, 2, 2, 2, 2, 2, 2, 2, 2, 2, 2, 2, 2, 2, 2, 2, 2, 2, 2, 2, 2, 2, 2, 2, 2, 2, 2, 2, 2, 2, 2, 2, 2, 2, 2, 3 ),
 ( 0.000000000000000000, 1.000000000000000000 ),
 ( 0.000000000000000000, 0.007812500000000000000, 0.01562500000000000000, 0.02343750000000000000, 0.03125000000000000000, 0.03906250000000000000, 0.04687500000000000000, 0.05468750000000000000, 0.06250000000000000000, 0.07031250000000000000, 0.07812500000000000000, 0.08593750000000000000, 0.09375000000000000000, 0.1015625000000000000, 0.1093750000000000000, 0.1171875000000000000, 0.1250000000000000000, 0.1328125000000000000, 0.1406250000000000000, 0.1484375000000000000, 0.1562500000000000000, 0.1640625000000000000, 0.1718750000000000000, 0.1796875000000000000, 0.1875000000000000000, 0.1953125000000000000, 0.2031250000000000000, 0.2109375000000000000, 0.2187500000000000000, 0.2265625000000000000, 0.2343750000000000000, 0.2421875000000000000, 0.2500000000000000000, 0.2578125000000000000, 0.2656250000000000000, 0.2734375000000000000, 0.2812500000000000000, 0.2890625000000000000, 0.2968750000000000000, 0.3046875000000000000, 0.3125000000000000000, 0.3203125000000000000, 0.3281250000000000000, 0.3359375000000000000, 0.3437500000000000000, 0.3515625000000000000, 0.3593750000000000000, 0.3671875000000000000, 0.3750000000000000000, 0.3828125000000000000, 0.3906250000000000000, 0.3984375000000000000, 0.4062500000000000000, 0.4140625000000000000, 0.4218750000000000000, 0.4296875000000000000, 0.4375000000000000000, 0.4453125000000000000, 0.4531250000000000000, 0.4609375000000000000, 0.4687500000000000000, 0.4765625000000000000, 0.4843750000000000000, 0.4921875000000000000, 0.5000000000000000000, 0.5078125000000000000, 0.5156250000000000000, 0.5234375000000000000, 0.5312500000000000000, 0.5390625000000000000, 0.5468750000000000000, 0.5546875000000000000, 0.5625000000000000000, 0.5703125000000000000, 0.5781250000000000000, 0.5859375000000000000, 0.5937500000000000000, 0.6015625000000000000, 0.6093750000000000000, 0.6171875000000000000, 0.6250000000000000000, 0.6328125000000000000, 0.6406250000000000000, 0.6484375000000000000, 0.6562500000000000000, 0.6640625000000000000, 0.6718750000000000000, 0.6796875000000000000, 0.6875000000000000000, 0.6953125000000000000, 0.7031250000000000000, 0.7109375000000000000, 0.7187500000000000000, 0.7265625000000000000, 0.7343750000000000000, 0.7421875000000000000, 0.7500000000000000000, 0.7578125000000000000, 0.7656250000000000000, 0.7734375000000000000, 0.7812500000000000000, 0.7890625000000000000, 0.7968750000000000000, 0.8046875000000000000, 0.8125000000000000000, 0.8203125000000000000, 0.8281250000000000000, 0.8359375000000000000, 0.8437500000000000000, 0.8515625000000000000, 0.8593750000000000000, 0.8671875000000000000, 0.8750000000000000000, 0.8828125000000000000, 0.8906250000000000000, 0.8984375000000000000, 0.9062500000000000000, 0.9140625000000000000, 0.9218750000000000000, 0.9296875000000000000, 0.9375000000000000000, 0.9453125000000000000, 0.9531250000000000000, 0.9609375000000000000, 0.9687500000000000000, 0.9765625000000000000, 0.9843750000000000000, 0.9921875000000000000, 1.000000000000000000 ),
 .UNSPECIFIED. ) 
 GEOMETRIC_REPRESENTATION_ITEM ( )  RATIONAL_B_SPLINE_SURFACE ( (
 ( 1.000000000000000000, 0.9238795325112869605, 1.000000000000000000, 0.9238795325112869605, 1.000000000000000000, 0.9238795325112869605, 1.000000000000000000, 0.9238795325112869605, 1.000000000000000000, 0.9238795325112869605, 1.000000000000000000, 0.9238795325112869605, 1.000000000000000000, 0.9238795325112869605, 1.000000000000000000, 0.9238795325112869605, 1.000000000000000000, 0.9238795325112869605, 1.000000000000000000, 0.9238795325112869605, 1.000000000000000000, 0.9238795325112869605, 1.000000000000000000, 0.9238795325112869605, 1.000000000000000000, 0.9238795325112869605, 1.000000000000000000, 0.9238795325112869605, 1.000000000000000000, 0.9238795325112869605, 1.000000000000000000, 0.9238795325112869605, 1.000000000000000000, 0.9238795325112869605, 1.000000000000000000, 0.9238795325112869605, 1.000000000000000000, 0.9238795325112869605, 1.000000000000000000, 0.9238795325112869605, 1.000000000000000000, 0.9238795325112869605, 1.000000000000000000, 0.9238795325112869605, 1.000000000000000000, 0.9238795325112869605, 1.000000000000000000, 0.9238795325112869605, 1.000000000000000000, 0.9238795325112869605, 1.000000000000000000, 0.9238795325112869605, 1.000000000000000000, 0.9238795325112869605, 1.000000000000000000, 0.9238795325112869605, 1.000000000000000000, 0.9238795325112869605, 1.000000000000000000, 0.9238795325112869605, 1.000000000000000000, 0.9238795325112869605, 1.000000000000000000, 0.9238795325112869605, 1.000000000000000000, 0.9238795325112869605, 1.000000000000000000, 0.9238795325112869605, 1.000000000000000000, 0.9238795325112869605, 1.000000000000000000, 0.9238795325112869605, 1.000000000000000000, 0.9238795325112869605, 1.000000000000000000, 0.9238795325112869605, 1.000000000000000000, 0.9238795325112869605, 1.000000000000000000, 0.9238795325112869605, 1.000000000000000000, 0.9238795325112869605, 1.000000000000000000, 0.9238795325112869605, 1.000000000000000000, 0.9238795325112869605, 1.000000000000000000, 0.9238795325112869605, 1.000000000000000000, 0.9238795325112869605, 1.000000000000000000, 0.9238795325112869605, 1.000000000000000000, 0.9238795325112869605, 1.000000000000000000, 0.9238795325112869605, 1.000000000000000000, 0.9238795325112869605, 1.000000000000000000, 0.9238795325112869605, 1.000000000000000000, 0.9238795325112869605, 1.000000000000000000, 0.9238795325112869605, 1.000000000000000000, 0.9238795325112869605, 1.000000000000000000, 0.9238795325112869605, 1.000000000000000000, 0.9238795325112869605, 1.000000000000000000, 0.9238795325112869605, 1.000000000000000000, 0.9238795325112869605, 1.000000000000000000, 0.9238795325112869605, 1.000000000000000000, 0.9238795325112869605, 1.000000000000000000, 0.9238795325112869605, 1.000000000000000000, 0.9238795325112869605, 1.000000000000000000, 0.9238795325112869605, 1.000000000000000000, 0.9238795325112869605, 1.000000000000000000, 0.9238795325112869605, 1.000000000000000000, 0.9238795325112869605, 1.000000000000000000, 0.9238795325112869605, 1.000000000000000000, 0.9238795325112869605, 1.000000000000000000, 0.9238795325112869605, 1.000000000000000000, 0.9238795325112869605, 1.000000000000000000, 0.9238795325112869605, 1.000000000000000000, 0.9238795325112869605, 1.000000000000000000, 0.9238795325112869605, 1.000000000000000000, 0.9238795325112869605, 1.000000000000000000, 0.9238795325112869605, 1.000000000000000000, 0.9238795325112869605, 1.000000000000000000, 0.9238795325112869605, 1.000000000000000000, 0.9238795325112869605, 1.000000000000000000, 0.9238795325112869605, 1.000000000000000000, 0.9238795325112869605, 1.000000000000000000, 0.9238795325112869605, 1.000000000000000000, 0.9238795325112869605, 1.000000000000000000, 0.9238795325112869605, 1.000000000000000000, 0.9238795325112869605, 1.000000000000000000, 0.9238795325112869605, 1.000000000000000000, 0.9238795325112869605, 1.000000000000000000, 0.9238795325112869605, 1.000000000000000000, 0.9238795325112869605, 1.000000000000000000, 0.9238795325112869605, 1.000000000000000000, 0.9238795325112869605, 1.000000000000000000, 0.9238795325112869605, 1.000000000000000000, 0.9238795325112869605, 1.000000000000000000, 0.9238795325112869605, 1.000000000000000000, 0.9238795325112869605, 1.000000000000000000, 0.9238795325112869605, 1.000000000000000000, 0.9238795325112869605, 1.000000000000000000, 0.9238795325112869605, 1.000000000000000000, 0.9238795325112869605, 1.000000000000000000, 0.9238795325112869605, 1.000000000000000000, 0.9238795325112869605, 1.000000000000000000, 0.9238795325112869605, 1.000000000000000000, 0.9238795325112869605, 1.000000000000000000, 0.9238795325112869605, 1.000000000000000000, 0.9238795325112869605, 1.000000000000000000, 0.9238795325112869605, 1.000000000000000000, 0.9238795325112869605, 1.000000000000000000, 0.9238795325112869605, 1.000000000000000000, 0.9238795325112869605, 1.000000000000000000, 0.9238795325112869605, 1.000000000000000000, 0.9238795325112869605, 1.000000000000000000, 0.9238795325112869605, 1.000000000000000000, 0.9238795325112869605, 1.000000000000000000, 0.9238795325112869605, 1.000000000000000000, 0.9238795325112869605, 1.000000000000000000, 0.9238795325112869605, 1.000000000000000000, 0.9238795325112869605, 1.000000000000000000, 0.9238795325112869605, 1.000000000000000000, 0.9238795325112869605, 1.000000000000000000, 0.9238795325112869605, 1.000000000000000000, 0.9238795325112869605, 1.000000000000000000, 0.9238795325112869605, 1.000000000000000000, 0.9238795325112869605, 1.000000000000000000, 0.9238795325112869605, 1.000000000000000000, 0.9238795325112869605, 1.000000000000000000, 0.9238795325112869605, 1.000000000000000000, 0.9238795325112869605, 1.000000000000000000, 0.9238795325112869605, 1.000000000000000000, 0.9238795325112869605, 1.000000000000000000, 0.9238795325112869605, 1.000000000000000000),
 ( 1.000000000000000000, 0.9238795325112869605, 1.000000000000000000, 0.9238795325112869605, 1.000000000000000000, 0.9238795325112869605, 1.000000000000000000, 0.9238795325112869605, 1.000000000000000000, 0.9238795325112869605, 1.000000000000000000, 0.9238795325112869605, 1.000000000000000000, 0.9238795325112869605, 1.000000000000000000, 0.9238795325112869605, 1.000000000000000000, 0.9238795325112869605, 1.000000000000000000, 0.9238795325112869605, 1.000000000000000000, 0.9238795325112869605, 1.000000000000000000, 0.9238795325112869605, 1.000000000000000000, 0.9238795325112869605, 1.000000000000000000, 0.9238795325112869605, 1.000000000000000000, 0.9238795325112869605, 1.000000000000000000, 0.9238795325112869605, 1.000000000000000000, 0.9238795325112869605, 1.000000000000000000, 0.9238795325112869605, 1.000000000000000000, 0.9238795325112869605, 1.000000000000000000, 0.9238795325112869605, 1.000000000000000000, 0.9238795325112869605, 1.000000000000000000, 0.9238795325112869605, 1.000000000000000000, 0.9238795325112869605, 1.000000000000000000, 0.9238795325112869605, 1.000000000000000000, 0.9238795325112869605, 1.000000000000000000, 0.9238795325112869605, 1.000000000000000000, 0.9238795325112869605, 1.000000000000000000, 0.9238795325112869605, 1.000000000000000000, 0.9238795325112869605, 1.000000000000000000, 0.9238795325112869605, 1.000000000000000000, 0.9238795325112869605, 1.000000000000000000, 0.9238795325112869605, 1.000000000000000000, 0.9238795325112869605, 1.000000000000000000, 0.9238795325112869605, 1.000000000000000000, 0.9238795325112869605, 1.000000000000000000, 0.9238795325112869605, 1.000000000000000000, 0.9238795325112869605, 1.000000000000000000, 0.9238795325112869605, 1.000000000000000000, 0.9238795325112869605, 1.000000000000000000, 0.9238795325112869605, 1.000000000000000000, 0.9238795325112869605, 1.000000000000000000, 0.9238795325112869605, 1.000000000000000000, 0.9238795325112869605, 1.000000000000000000, 0.9238795325112869605, 1.000000000000000000, 0.9238795325112869605, 1.000000000000000000, 0.9238795325112869605, 1.000000000000000000, 0.9238795325112869605, 1.000000000000000000, 0.9238795325112869605, 1.000000000000000000, 0.9238795325112869605, 1.000000000000000000, 0.9238795325112869605, 1.000000000000000000, 0.9238795325112869605, 1.000000000000000000, 0.9238795325112869605, 1.000000000000000000, 0.9238795325112869605, 1.000000000000000000, 0.9238795325112869605, 1.000000000000000000, 0.9238795325112869605, 1.000000000000000000, 0.9238795325112869605, 1.000000000000000000, 0.9238795325112869605, 1.000000000000000000, 0.9238795325112869605, 1.000000000000000000, 0.9238795325112869605, 1.000000000000000000, 0.9238795325112869605, 1.000000000000000000, 0.9238795325112869605, 1.000000000000000000, 0.9238795325112869605, 1.000000000000000000, 0.9238795325112869605, 1.000000000000000000, 0.9238795325112869605, 1.000000000000000000, 0.9238795325112869605, 1.000000000000000000, 0.9238795325112869605, 1.000000000000000000, 0.9238795325112869605, 1.000000000000000000, 0.9238795325112869605, 1.000000000000000000, 0.9238795325112869605, 1.000000000000000000, 0.9238795325112869605, 1.000000000000000000, 0.9238795325112869605, 1.000000000000000000, 0.9238795325112869605, 1.000000000000000000, 0.9238795325112869605, 1.000000000000000000, 0.9238795325112869605, 1.000000000000000000, 0.9238795325112869605, 1.000000000000000000, 0.9238795325112869605, 1.000000000000000000, 0.9238795325112869605, 1.000000000000000000, 0.9238795325112869605, 1.000000000000000000, 0.9238795325112869605, 1.000000000000000000, 0.9238795325112869605, 1.000000000000000000, 0.9238795325112869605, 1.000000000000000000, 0.9238795325112869605, 1.000000000000000000, 0.9238795325112869605, 1.000000000000000000, 0.9238795325112869605, 1.000000000000000000, 0.9238795325112869605, 1.000000000000000000, 0.9238795325112869605, 1.000000000000000000, 0.9238795325112869605, 1.000000000000000000, 0.9238795325112869605, 1.000000000000000000, 0.9238795325112869605, 1.000000000000000000, 0.9238795325112869605, 1.000000000000000000, 0.9238795325112869605, 1.000000000000000000, 0.9238795325112869605, 1.000000000000000000, 0.9238795325112869605, 1.000000000000000000, 0.9238795325112869605, 1.000000000000000000, 0.9238795325112869605, 1.000000000000000000, 0.9238795325112869605, 1.000000000000000000, 0.9238795325112869605, 1.000000000000000000, 0.9238795325112869605, 1.000000000000000000, 0.9238795325112869605, 1.000000000000000000, 0.9238795325112869605, 1.000000000000000000, 0.9238795325112869605, 1.000000000000000000, 0.9238795325112869605, 1.000000000000000000, 0.9238795325112869605, 1.000000000000000000, 0.9238795325112869605, 1.000000000000000000, 0.9238795325112869605, 1.000000000000000000, 0.9238795325112869605, 1.000000000000000000, 0.9238795325112869605, 1.000000000000000000, 0.9238795325112869605, 1.000000000000000000, 0.9238795325112869605, 1.000000000000000000, 0.9238795325112869605, 1.000000000000000000, 0.9238795325112869605, 1.000000000000000000, 0.9238795325112869605, 1.000000000000000000, 0.9238795325112869605, 1.000000000000000000, 0.9238795325112869605, 1.000000000000000000, 0.9238795325112869605, 1.000000000000000000, 0.9238795325112869605, 1.000000000000000000, 0.9238795325112869605, 1.000000000000000000, 0.9238795325112869605, 1.000000000000000000, 0.9238795325112869605, 1.000000000000000000, 0.9238795325112869605, 1.000000000000000000, 0.9238795325112869605, 1.000000000000000000, 0.9238795325112869605, 1.000000000000000000, 0.9238795325112869605, 1.000000000000000000, 0.9238795325112869605, 1.000000000000000000, 0.9238795325112869605, 1.000000000000000000, 0.9238795325112869605, 1.000000000000000000, 0.9238795325112869605, 1.000000000000000000, 0.9238795325112869605, 1.000000000000000000) ) ) 
 REPRESENTATION_ITEM ( '' )  SURFACE ( )  );
#30560 = ADVANCED_FACE ( 'NONE', ( #5751 ), #44086, .T. ) ;
#30561 = CARTESIAN_POINT ( 'NONE',  ( 123.6328298109119714, -2.173413727453596511, -8.297982527556804655 ) ) ;
#30562 = CARTESIAN_POINT ( 'NONE',  ( 124.3117748109119844, -10.30919188438810075, -12.61870101168855918 ) ) ;
#30563 = CARTESIAN_POINT ( 'NONE',  ( 107.4266296295248821, -4.863998795839590272, -19.15521520033831493 ) ) ;
#30564 = CARTESIAN_POINT ( 'NONE',  ( 124.2916835400977504, -1.223627541775709870, -16.99192386690442902 ) ) ;
#30565 = ORIENTED_EDGE ( 'NONE', *, *, #31406, .F. ) ;
#30566 = CARTESIAN_POINT ( 'NONE',  ( 70.19189222814998175, -65.04786711941002864, -39.22192925581976652 ) ) ;
#30567 = CARTESIAN_POINT ( 'NONE',  ( 123.8579614775786126, -9.859900752359378018, -12.68260735090039759 ) ) ;
#30568 = CARTESIAN_POINT ( 'NONE',  ( 119.8870948109119752, -9.261995988541697145, -16.69588392320189030 ) ) ;
#30569 = CARTESIAN_POINT ( 'NONE',  ( 112.2857214775786474, -5.574606645277164318, -18.38911715685844683 ) ) ;
#30570 = CARTESIAN_POINT ( 'NONE',  ( 115.0086014775786509, -4.089484607189486809, -7.948022111789456723 ) ) ;
#30571 = CARTESIAN_POINT ( 'NONE',  ( 86.34560043013698305, -9.320000780048239619, -8.143215200338314474 ) ) ;
#30572 = CARTESIAN_POINT ( 'NONE',  ( 125.3895814775786448, -2.084020599724406786, -8.691656652584148546 ) ) ;
#30573 = CARTESIAN_POINT ( 'NONE',  ( 117.6180281442453150, -8.899110576539710493, -16.42337572283490132 ) ) ;
#30574 = VERTEX_POINT ( 'NONE', #37448 ) ;
#30575 = CARTESIAN_POINT ( 'NONE',  ( 121.5492360609119800, -6.564341423271550902, -7.887810678476487425 ) ) ;
#30576 = CIRCLE ( 'NONE', #31312, 1.999999999999999112 ) ;
#30577 = CARTESIAN_POINT ( 'NONE',  ( 115.2922348109119781, -10.63000616557722466, -14.87417383870573495 ) ) ;
#30578 = CARTESIAN_POINT ( 'NONE',  ( 122.2128881442453263, -7.643976991954077427, -18.09477374809248928 ) ) ;
#30579 = ORIENTED_EDGE ( 'NONE', *, *, #32648, .F. ) ;
#30580 = CARTESIAN_POINT ( 'NONE',  ( 121.9659548109119811, -2.527210466738041728, -8.967976844669124148 ) ) ;
#30581 = CARTESIAN_POINT ( 'NONE',  ( 136.9115742440200734, -1.268299463231087110, -9.195838862358661103 ) ) ;
#30582 = CARTESIAN_POINT ( 'NONE',  ( 118.1285681442453068, -7.893985811506177619, -18.51759400769804742 ) ) ;
#30583 = CARTESIAN_POINT ( 'NONE',  ( 110.4131140045248287, -10.62599879583958717, -11.00651665394454604 ) ) ;
#30584 = CARTESIAN_POINT ( 'NONE',  ( 114.8951481442453115, -8.899110576539710493, -16.42337572283490132 ) ) ;
#30585 = EDGE_CURVE ( 'NONE', #18037, #4544, #6672, .T. ) ;
#30586 = ORIENTED_EDGE ( 'NONE', *, *, #37559, .F. ) ;
#30587 = ORIENTED_EDGE ( 'NONE', *, *, #26449, .F. ) ;
#30588 = VECTOR ( 'NONE', #6796, 1000.000000000000000 ) ;
#30589 = CARTESIAN_POINT ( 'NONE',  ( 112.4559014775786494, -9.988377603198976828, -10.36322818467138340 ) ) ;
#30590 = CARTESIAN_POINT ( 'NONE',  ( 125.3328548109119964, -0.8288870151387760510, -10.36305467784173118 ) ) ;
#30591 = CIRCLE ( 'NONE', #38805, 8.000000000000001776 ) ;
#30592 = ADVANCED_FACE ( 'NONE', ( #33793 ), #30842, .F. ) ;
#30593 = FACE_OUTER_BOUND ( 'NONE', #7137, .T. ) ;
#30594 = EDGE_CURVE ( 'NONE', #39376, #4486, #20365, .T. ) ;
#30595 = CARTESIAN_POINT ( 'NONE',  ( 122.6099748109119929, -9.261995988541697145, -16.69588392320189030 ) ) ;
#30596 = CARTESIAN_POINT ( 'NONE',  ( 138.2184548109119930, 2.066246953222917959, -14.37896053134723040 ) ) ;
#30597 = FACE_OUTER_BOUND ( 'NONE', #27616, .T. ) ;
#30598 = CARTESIAN_POINT ( 'NONE',  ( 121.0216281442452981, -1.561330072975668948, -17.79121239304076951 ) ) ;
#30600 = CARTESIAN_POINT ( 'NONE',  ( 118.0718414775786442, -0.8288870151387760510, -10.36305467784173118 ) ) ;
#30599 = CARTESIAN_POINT ( 'NONE',  ( 117.2776681442452968, -5.638512984488999180, -18.83840828888717311 ) ) ;
#30601 = DIRECTION ( 'NONE',  ( -0.000000000000000000, -0.9284778069183720062, -0.3713878862591650232 ) ) ;
#30602 = CARTESIAN_POINT ( 'NONE',  ( 112.5693548109119888, -10.63000616557722466, -14.87417383870573495 ) ) ;
#30603 = VERTEX_POINT ( 'NONE', #40892 ) ;
#30604 = CARTESIAN_POINT ( 'NONE',  ( 124.8223148109119762, -10.15424416112533912, -14.75197769757731336 ) ) ;
#30605 = FACE_OUTER_BOUND ( 'NONE', #29857, .T. ) ;
#30606 = EDGE_CURVE ( 'NONE', #3191, #27343, #27907, .T. ) ;
#30607 = CARTESIAN_POINT ( 'NONE',  ( 121.2778147965036339, -8.305800998871424312, -17.19128988610634678 ) ) ;
#30608 = CARTESIAN_POINT ( 'NONE',  ( 108.4684265045247997, -7.250697342233347165, -19.15521520033831138 ) ) ;
#30609 = CARTESIAN_POINT ( 'NONE',  ( 112.4967077545247633, -2.791137627527939813, -18.39754474579286025 ) ) ;
#30610 = CARTESIAN_POINT ( 'NONE',  ( 107.5655358795247736, -0.7896495226426338832, -17.46756447353520159 ) ) ;
#30611 = AXIS2_PLACEMENT_3D ( 'NONE', #10052, #2962, #6396 ) ;
#30612 = CARTESIAN_POINT ( 'NONE',  ( 121.4187148109119789, -6.344957434206665248, -7.627207830600338134 ) ) ;
#30613 = CARTESIAN_POINT ( 'NONE',  ( 122.6099748109119929, -0.8288870151387760510, -10.36305467784173118 ) ) ;
#30614 = ORIENTED_EDGE ( 'NONE', *, *, #35896, .F. ) ;
#30615 = ADVANCED_FACE ( 'NONE', ( #33559 ), #9645, .F. ) ;
#30616 = CARTESIAN_POINT ( 'NONE',  ( 123.2906948109119867, -8.166667518702819706, -8.995218007635861213 ) ) ;
#30617 = CARTESIAN_POINT ( 'NONE',  ( 114.1009748109119784, -5.574606645277164318, -18.38911715685844683 ) ) ;
#30618 = CARTESIAN_POINT ( 'NONE',  ( 90.04708369096697140, -25.79823837677164988, -13.86919086559751157 ) ) ;
#30619 = CARTESIAN_POINT ( 'NONE',  ( 120.8514481442452961, -7.893985811506177619, -18.51759400769804742 ) ) ;
#30620 = EDGE_CURVE ( 'NONE', #26284, #37865, #25610, .T. ) ;
#30621 = ADVANCED_FACE ( 'NONE', ( #27432 ), #41890, .T. ) ;
#30622 = CARTESIAN_POINT ( 'NONE',  ( 119.4332814775786318, -0.4660016031367893996, -10.09054647747474043 ) ) ;
#30623 = CARTESIAN_POINT ( 'NONE',  ( 119.6740016859119748, -0.6942167230862511529, -9.935906262978006609 ) ) ;
#30624 = CARTESIAN_POINT ( 'NONE',  ( 112.5126281442453120, -10.30919188438810075, -12.61870101168855918 ) ) ;
#30625 = CARTESIAN_POINT ( 'NONE',  ( 123.2855641859119942, -8.321307733199551748, -9.223433127585318303 ) ) ;
#30626 = ORIENTED_EDGE ( 'NONE', *, *, #9988, .F. ) ;
#30627 = CARTESIAN_POINT ( 'NONE',  ( 124.6329298793804981, -2.191907684172563986, -18.20049396185734025 ) ) ;
#30628 = CARTESIAN_POINT ( 'NONE',  ( 112.9664414775786412, -9.859900752359374465, -12.68260735090039404 ) ) ;
#30629 = CARTESIAN_POINT ( 'NONE',  ( 125.1626748109119802, -0.1624402480850797581, -16.17319339645315424 ) ) ;
#30630 = CARTESIAN_POINT ( 'NONE',  ( 108.8156921295247912, -9.868328341294093420, -13.39321520033831447 ) ) ;
#30631 = CARTESIAN_POINT ( 'NONE',  ( 112.7745202545247878, 0.1403307496149616695, -11.32035403202665336 ) ) ;
#30632 = AXIS2_PLACEMENT_3D ( 'NONE', #42433, #11197, #32150 ) ;
#30633 = CARTESIAN_POINT ( 'NONE',  ( 121.1918081442452859, -10.15424416112533912, -14.75197769757731336 ) ) ;
#30634 = CARTESIAN_POINT ( 'NONE',  ( 114.4980614775786734, -2.084020599724406786, -8.691656652584148546 ) ) ;
#30635 = CARTESIAN_POINT ( 'NONE',  ( 124.1415948109119540, -6.344957434206665248, -7.627207830600338134 ) ) ;
#30636 = ORIENTED_EDGE ( 'NONE', *, *, #35560, .T. ) ;
#30637 = CARTESIAN_POINT ( 'NONE',  ( 120.5110881442453206, -3.505236298600246325, -18.68346056562440793 ) ) ;
#30638 = CARTESIAN_POINT ( 'NONE',  ( 119.0361948109119652, -7.893985811506177619, -18.51759400769804742 ) ) ;
#30639 = CARTESIAN_POINT ( 'NONE',  ( 123.5743281442453139, -7.893985811506177619, -18.51759400769804742 ) ) ;
#30640 = CARTESIAN_POINT ( 'NONE',  ( 125.2761281442453054, 0.4262465694468514643, -12.03445270309931736 ) ) ;
#30641 = ORIENTED_EDGE ( 'NONE', *, *, #23359, .T. ) ;
#30642 = CYLINDRICAL_SURFACE ( 'NONE', #40550, 8.000000000000001776 ) ;
#30643 = CARTESIAN_POINT ( 'NONE',  ( 122.8936081442453059, 0.2603800115204892296, -16.42320221600525088 ) ) ;
#30644 = AXIS2_PLACEMENT_3D ( 'NONE', #44093, #37454, #33799 ) ;
#30645 = CARTESIAN_POINT ( 'NONE',  ( 115.0653281442453277, -3.505236298600246325, -18.68346056562440793 ) ) ;
#30646 =( BOUNDED_CURVE ( )  B_SPLINE_CURVE ( 3, ( #26472, #40837, #19619, #20084 ),
 .UNSPECIFIED., .F., .F. ) 
 B_SPLINE_CURVE_WITH_KNOTS ( ( 4, 4 ),
 ( 1.534323482254100091, 1.570796326794904996 ),
 .UNSPECIFIED. ) 
 CURVE ( )  GEOMETRIC_REPRESENTATION_ITEM ( )  RATIONAL_B_SPLINE_CURVE ( ( 1.000000000000000000, 0.9998891473731379431, 0.9998891473731379431, 1.000000000000000000 ) ) 
 REPRESENTATION_ITEM ( '' )  );
#30647 = CARTESIAN_POINT ( 'NONE',  ( 125.5030348109119558, -3.383040157471821630, -19.15922257007629170 ) ) ;
#30648 = DIRECTION ( 'NONE',  ( 0.000000000000000000, 0.000000000000000000, 1.000000000000000000 ) ) ;
#30649 = CARTESIAN_POINT ( 'NONE',  ( 121.8270485609119760, -0.08252387247370887580, -11.91645802438286417 ) ) ;
#30650 = ORIENTED_EDGE ( 'NONE', *, *, #39832, .T. ) ;
#30651 = CARTESIAN_POINT ( 'NONE',  ( 59.41474631770697812, -13.68180984308303039, -7.393215200338313586 ) ) ;
#30652 = CARTESIAN_POINT ( 'NONE',  ( 61.41196271890139258, -3.923926642757838756, -7.421452497510491852 ) ) ;
#30653 = EDGE_CURVE ( 'NONE', #25917, #13764, #16902, .T. ) ;
#30654 = CARTESIAN_POINT ( 'NONE',  ( 116.2471765045247594, -7.250697342233347165, -19.15521520033831138 ) ) ;
#30655 = CIRCLE ( 'NONE', #5115, 2.999999999999999556 ) ;
#30656 = DIRECTION ( 'NONE',  ( 0.1352586133457950590, 0.9908103287288504424, 0.000000000000000000 ) ) ;
#30657 = CARTESIAN_POINT ( 'NONE',  ( 123.9146881442452894, -10.15424416112533912, -14.75197769757731336 ) ) ;
#30658 = CARTESIAN_POINT ( 'NONE',  ( 115.2922348109119781, 0.4262465694468514643, -12.03445270309931736 ) ) ;
#30659 = CARTESIAN_POINT ( 'NONE',  ( 127.3434826497349377, 0.2239902821118424925, -11.13838800870225043 ) ) ;
#30660 = ORIENTED_EDGE ( 'NONE', *, *, #33918, .T. ) ;
#30661 = LINE ( 'NONE', #40935, #6944 ) ;
#30662 = CARTESIAN_POINT ( 'NONE',  ( 121.4187148109119789, -3.505236298600246325, -18.68346056562440793 ) ) ;
#30663 = CARTESIAN_POINT ( 'NONE',  ( 114.2711548109119803, -0.1624402480850797581, -16.17319339645315424 ) ) ;
#30664 = CARTESIAN_POINT ( 'NONE',  ( 111.3780948109119890, -5.574606645277164318, -18.38911715685844683 ) ) ;
#30666 = CARTESIAN_POINT ( 'NONE',  ( 125.4463081442452932, -5.638512984488999180, -18.83840828888717311 ) ) ;
#30665 = CARTESIAN_POINT ( 'NONE',  ( 113.8604010812576774, -0.01829820670803256055, -12.14321520033831625 ) ) ;
#30667 = CARTESIAN_POINT ( 'NONE',  ( 112.8529881442453302, -1.561330072975668060, -17.79121239304076596 ) ) ;
#30668 = ORIENTED_EDGE ( 'NONE', *, *, #38003, .T. ) ;
#30669 = CARTESIAN_POINT ( 'NONE',  ( 112.5693548109119888, -10.63000616557722466, -14.87417383870573495 ) ) ;
#30670 = CARTESIAN_POINT ( 'NONE',  ( 126.3509913982080946, 0.07182886583579818629, -14.53637278171945546 ) ) ;
#30671 = CARTESIAN_POINT ( 'NONE',  ( 115.9693640045247776, -10.62599879583958717, -11.00651665394454604 ) ) ;
#30672 = EDGE_CURVE ( 'NONE', #42235, #2538, #6051, .T. ) ;
#30673 = CARTESIAN_POINT ( 'NONE',  ( 123.9146881442452894, -10.15424416112533912, -14.75197769757731336 ) ) ;
#30674 = CARTESIAN_POINT ( 'NONE',  ( 121.8725281442453223, -6.222761293078241884, -8.102969835052219238 ) ) ;
#30675 = CARTESIAN_POINT ( 'NONE',  ( 122.6009548109119720, -1.204716393658298523, -20.50726132761981901 ) ) ;
#30676 = CARTESIAN_POINT ( 'NONE',  ( 115.4831921295247952, -9.868328341294093420, -13.39321520033831447 ) ) ;
#30677 = CARTESIAN_POINT ( 'NONE',  ( 111.9653064975817927, -2.215723800389698184, -18.16877924232191788 ) ) ;
#30678 = EDGE_CURVE ( 'NONE', #20119, #41097, #21955, .T. ) ;
#30679 = CARTESIAN_POINT ( 'NONE',  ( 119.8823610609119754, -6.340755971794695078, -8.611740276972781771 ) ) ;
#30680 = CONICAL_SURFACE ( 'NONE', #38651, 1.610000000000000986, 0.9599310885968765916 ) ;
#30681 = CARTESIAN_POINT ( 'NONE',  ( 138.2184548109119930, -10.46144976836963814, -17.59661175671013922 ) ) ;
#30682 = FACE_OUTER_BOUND ( 'NONE', #11025, .T. ) ;
#30683 = DIRECTION ( 'NONE',  ( -1.000000000000000000, 0.000000000000000000, -0.000000000000000000 ) ) ;
#30684 = CARTESIAN_POINT ( 'NONE',  ( 113.4690515045247992, -2.477300249445798297, -7.631215200338321125 ) ) ;
#30685 = CARTESIAN_POINT ( 'NONE',  ( 125.6732148109119862, 0.5811942927096110934, -14.16772938898807510 ) ) ;
#30686 = CARTESIAN_POINT ( 'NONE',  ( 123.6310548109119765, -5.638512984488999180, -18.83840828888717311 ) ) ;
#30687 = EDGE_CURVE ( 'NONE', #20884, #42739, #18417, .T. ) ;
#30688 = CARTESIAN_POINT ( 'NONE',  ( 119.9438214775786378, -7.893985811506177619, -18.51759400769804742 ) ) ;
#30689 = CARTESIAN_POINT ( 'NONE',  ( 112.2857214775786474, -4.089484607189486809, -7.948022111789456723 ) ) ;
#30690 = EDGE_LOOP ( 'NONE', ( #42818, #30368, #30014, #39205 ) ) ;
#30691 = CARTESIAN_POINT ( 'NONE',  ( 113.2500748109119968, -3.505236298600246325, -18.68346056562440793 ) ) ;
#30692 = CARTESIAN_POINT ( 'NONE',  ( 111.4915481442453142, -1.833838273342658365, -17.42832698103878286 ) ) ;
#30693 = CONICAL_SURFACE ( 'NONE', #8812, 2.999999999999999556, 0.9599310885968830309 ) ;
#30694 = CARTESIAN_POINT ( 'NONE',  ( 123.4041481442452834, -10.30919188438810075, -12.61870101168855918 ) ) ;
#30695 = CARTESIAN_POINT ( 'NONE',  ( 115.2355081442453155, -10.30919188438810075, -12.61870101168855918 ) ) ;
#30696 = CARTESIAN_POINT ( 'NONE',  ( 112.6828081442453282, -2.084020599724406786, -8.691656652584148546 ) ) ;
#30697 = VERTEX_POINT ( 'NONE', #7114 ) ;
#30698 = CARTESIAN_POINT ( 'NONE',  ( 117.7882081442453170, -3.505236298600246325, -18.68346056562440793 ) ) ;
#30699 = CARTESIAN_POINT ( 'NONE',  ( 105.9681140045248355, -10.62599879583958717, -11.00651665394454604 ) ) ;
#30700 = CARTESIAN_POINT ( 'NONE',  ( 123.4041481442452834, 0.1319031606808879209, -14.10382304977623669 ) ) ;
#30701 = CARTESIAN_POINT ( 'NONE',  ( 80.91184012100937650, -3.933054092416038650, -10.89321520033831447 ) ) ;
#30702 = CARTESIAN_POINT ( 'NONE',  ( 112.2883483795247770, -0.7896495226426338832, -9.318865927141430916 ) ) ;
#30703 = ORIENTED_EDGE ( 'NONE', *, *, #36407, .T. ) ;
#30704 = CARTESIAN_POINT ( 'NONE',  ( 69.36136150295220659, -101.1685209014307674, -50.56525720990386219 ) ) ;
#30705 = DIRECTION ( 'NONE',  ( 0.000000000000000000, 0.000000000000000000, 1.000000000000000000 ) ) ;
#30706 = DIRECTION ( 'NONE',  ( -0.9908103287288504424, 0.1352586133457950590, 0.000000000000000000 ) ) ;
#30707 = CARTESIAN_POINT ( 'NONE',  ( 112.2289948109119848, -1.834011780172310813, -8.268836392978581529 ) ) ;
#30708 = CARTESIAN_POINT ( 'NONE',  ( 116.4217710891409610, 2.238304050683879609, -6.396164327732187793 ) ) ;
#30709 = CARTESIAN_POINT ( 'NONE',  ( 124.6573089231390128, -8.937933314682689812, -16.35309209503746786 ) ) ;
#30710 = CARTESIAN_POINT ( 'NONE',  ( 109.0240515045248202, -6.936859964151250502, -18.39754474579286025 ) ) ;
#30711 = ADVANCED_FACE ( 'NONE', ( #28316, #710 ), #38123, .F. ) ;
#30712 = DIRECTION ( 'NONE',  ( 0.000000000000000000, 0.000000000000000000, 1.000000000000000000 ) ) ;
#30713 = CARTESIAN_POINT ( 'NONE',  ( 117.1074881442453233, -10.63000616557722466, -14.87417383870573495 ) ) ;
#30714 = CARTESIAN_POINT ( 'NONE',  ( 137.2687954574917910, -6.421912352659795431, -18.40503953683662175 ) ) ;
#30715 = VECTOR ( 'NONE', #21698, 1000.000000000000000 ) ;
#30716 = CARTESIAN_POINT ( 'NONE',  ( 125.4584548109119737, 3.382738713931011443, -10.84621265594315176 ) ) ;
#30717 = CARTESIAN_POINT ( 'NONE',  ( 124.8223148109119762, 0.9020085738987339008, -11.91225656197089222 ) ) ;
#30718 = CARTESIAN_POINT ( 'NONE',  ( 121.9859814775786333, -9.565557343593413364, -10.61323700422348004 ) ) ;
#30719 = ORIENTED_EDGE ( 'NONE', *, *, #30672, .F. ) ;
#30720 = CARTESIAN_POINT ( 'NONE',  ( 126.0703014775786102, -9.988377603198980381, -10.36322818467138518 ) ) ;
#30721 = CARTESIAN_POINT ( 'NONE',  ( 120.7379948109119709, -10.63000616557722466, -14.87417383870573495 ) ) ;
#30722 = FACE_OUTER_BOUND ( 'NONE', #1602, .T. ) ;
#30723 = CARTESIAN_POINT ( 'NONE',  ( 115.9162281442453235, -5.574606645277164318, -18.38911715685844683 ) ) ;
#30724 = CARTESIAN_POINT ( 'NONE',  ( 124.5386814775786206, -5.638512984488999180, -18.83840828888717311 ) ) ;
#30725 = CARTESIAN_POINT ( 'NONE',  ( 112.5661608795247872, -8.938348069036489818, -9.318865927141430916 ) ) ;
#30726 = CARTESIAN_POINT ( 'NONE',  ( 62.22678445075433018, -36.72958069525633817, -5.531797115907686191 ) ) ;
#30727 = CARTESIAN_POINT ( 'NONE',  ( 116.0388171295248014, -10.62599879583958540, -13.39321520033831447 ) ) ;
#30728 = CARTESIAN_POINT ( 'NONE',  ( 115.5758681442453053, -7.894159318335828068, -9.358103419637847864 ) ) ;
#30729 = CARTESIAN_POINT ( 'NONE',  ( 116.5969481442453031, -9.859900752359374465, -12.68260735090039404 ) ) ;
#30730 = EDGE_CURVE ( 'NONE', #13043, #4906, #34685, .T. ) ;
#30731 = CARTESIAN_POINT ( 'NONE',  ( 90.72400676789006013, -25.99489077589524300, -13.39321520033831625 ) ) ;
#30732 = CARTESIAN_POINT ( 'NONE',  ( 113.4690515045247992, -6.936859964151250502, -18.39754474579286025 ) ) ;
#30733 = ORIENTED_EDGE ( 'NONE', *, *, #14510, .F. ) ;
#30734 = DIRECTION ( 'NONE',  ( -0.000000000000000000, -0.9284778069183721172, -0.3713878862591650232 ) ) ;
#30735 = CARTESIAN_POINT ( 'NONE',  ( 114.4980614775786592, -7.893985811506177619, -18.51759400769804742 ) ) ;
#30736 = DIRECTION ( 'NONE',  ( 0.000000000000000000, -0.3818493186865927203, 0.9242245927363029745 ) ) ;
#30737 = CARTESIAN_POINT ( 'NONE',  ( 123.4939235609119663, -9.645473719204776586, -14.86997237629376656 ) ) ;
#30738 = CARTESIAN_POINT ( 'NONE',  ( 122.1048610609119720, -6.340755971794695078, -8.611740276972781771 ) ) ;
#30739 = ORIENTED_EDGE ( 'NONE', *, *, #4911, .F. ) ;
#30740 = DIRECTION ( 'NONE',  ( 0.000000000000000000, -0.9242245927363005320, -0.3818493186865984379 ) ) ;
#30741 = CARTESIAN_POINT ( 'NONE',  ( 116.8309807853375588, -11.70023447154984453, -21.43868405042244163 ) ) ;
#30742 = ORIENTED_EDGE ( 'NONE', *, *, #40253, .T. ) ;
#30743 = CARTESIAN_POINT ( 'NONE',  ( 123.4608748109119745, -10.63000616557722466, -14.87417383870573495 ) ) ;
#30744 = CARTESIAN_POINT ( 'NONE',  ( 113.1366214775786432, -1.834011780172310813, -8.268836392978581529 ) ) ;
#30745 = CARTESIAN_POINT ( 'NONE',  ( 120.0572748109119772, -6.222761293078241884, -8.102969835052219238 ) ) ;
#30746 =( NAMED_UNIT ( * ) SI_UNIT ( $, .STERADIAN. ) SOLID_ANGLE_UNIT ( ) );
#30747 = CARTESIAN_POINT ( 'NONE',  ( 92.26512299712632625, -23.76310523276723785, -6.893215200338315363 ) ) ;
#30748 = CARTESIAN_POINT ( 'NONE',  ( 120.9081748109119872, -5.638512984488999180, -18.83840828888717311 ) ) ;
#30749 = CARTESIAN_POINT ( 'NONE',  ( 117.7314814775786260, -4.089484607189486809, -7.948022111789456723 ) ) ;
#30750 = CARTESIAN_POINT ( 'NONE',  ( 116.5944421295247793, 0.8980012041604618078, -13.39321520033831447 ) ) ;
#30751 = AXIS2_PLACEMENT_3D ( 'NONE', #4297, #38068, #28490 ) ;
#30752 = CARTESIAN_POINT ( 'NONE',  ( 112.6260814775786514, -0.8288870151387760510, -10.36305467784173118 ) ) ;
#30753 = CARTESIAN_POINT ( 'NONE',  ( 88.46631044337289040, -27.84333996136784961, -14.15691383771150136 ) ) ;
#30754 = ORIENTED_EDGE ( 'NONE', *, *, #27562, .T. ) ;
#30755 = CARTESIAN_POINT ( 'NONE',  ( 117.3911214775786505, -1.561330072975668504, -17.79121239304076951 ) ) ;
#30756 = CARTESIAN_POINT ( 'NONE',  ( 120.8547048109119686, -7.554583864224885481, -18.48844787311982785 ) ) ;
#30757 = CARTESIAN_POINT ( 'NONE',  ( 115.0086014775786509, -4.089484607189486809, -7.948022111789456723 ) ) ;
#30758 = EDGE_LOOP ( 'NONE', ( #26546, #43835, #15728, #8078 ) ) ;
#30759 = CARTESIAN_POINT ( 'NONE',  ( 120.6245414775786458, -9.988377603198976828, -10.36322818467138340 ) ) ;
#30760 = CYLINDRICAL_SURFACE ( 'NONE', #31085, 1.299999999999995604 ) ;
#30761 = CARTESIAN_POINT ( 'NONE',  ( 113.7038881442453402, -6.222761293078241884, -8.102969835052219238 ) ) ;
#30762 = PLANE ( 'NONE',  #17834 ) ;
#30763 = CARTESIAN_POINT ( 'NONE',  ( 117.1074881442453233, 0.4262465694468514643, -12.03445270309931736 ) ) ;
#30764 = CARTESIAN_POINT ( 'NONE',  ( 78.69189222814998175, -48.76310523276723785, -23.89321520033831803 ) ) ;
#30765 = AXIS2_PLACEMENT_3D ( 'NONE', #44491, #10729, #6859 ) ;
#30766 = CARTESIAN_POINT ( 'NONE',  ( 116.1998614775786507, 0.4262465694468514643, -12.03445270309931736 ) ) ;
#30767 = FACE_OUTER_BOUND ( 'NONE', #30391, .T. ) ;
#30768 = CARTESIAN_POINT ( 'NONE',  ( 115.2922348109119781, 0.4262465694468514643, -12.03445270309931736 ) ) ;
#30769 = CARTESIAN_POINT ( 'NONE',  ( 116.3133148109119759, -7.893985811506177619, -18.51759400769804742 ) ) ;
#30770 = CARTESIAN_POINT ( 'NONE',  ( 123.1466579359119891, -5.444069387712269226, -19.60292469916370450 ) ) ;
#30771 = CARTESIAN_POINT ( 'NONE',  ( 114.3846081442453197, -10.63000616557722466, -14.87417383870573495 ) ) ;
#30772 = CARTESIAN_POINT ( 'NONE',  ( 114.4980614775786734, -2.084020599724406786, -8.691656652584148546 ) ) ;
#30773 = CARTESIAN_POINT ( 'NONE',  ( 112.1155414775786454, -10.15424416112533912, -14.75197769757731336 ) ) ;
#30774 = PRESENTATION_LAYER_ASSIGNMENT (  '', '', ( #13317 ) ) ;
#30775 = CARTESIAN_POINT ( 'NONE',  ( 115.6893214775786447, -9.859900752359374465, -12.68260735090039404 ) ) ;
#30776 = ORIENTED_EDGE ( 'NONE', *, *, #17831, .T. ) ;
#30777 = CARTESIAN_POINT ( 'NONE',  ( 114.4413348109119823, -9.261995988541697145, -16.69588392320189030 ) ) ;
#30778 = CARTESIAN_POINT ( 'NONE',  ( 106.9404577545248145, -7.250697342233347165, -7.631215200338321125 ) ) ;
#30779 = CARTESIAN_POINT ( 'NONE',  ( 107.3571765045248299, -2.791137627527939813, -8.388885654883777576 ) ) ;
#30780 = AXIS2_PLACEMENT_3D ( 'NONE', #33937, #16180, #9334 ) ;
#30781 = CARTESIAN_POINT ( 'NONE',  ( 96.54708369096698561, -25.64989040597826175, -15.57695047384496156 ) ) ;
#30782 = EDGE_CURVE ( 'NONE', #26522, #20212, #37237, .T. ) ;
#30783 = CARTESIAN_POINT ( 'NONE',  ( 83.44708369096697709, -25.23119213852205789, -15.24166438581092109 ) ) ;
#30784 = CARTESIAN_POINT ( 'NONE',  ( 118.2420214775786320, -3.383040157471821630, -19.15922257007629170 ) ) ;
#30785 = ORIENTED_EDGE ( 'NONE', *, *, #17538, .T. ) ;
#30786 = CARTESIAN_POINT ( 'NONE',  ( 116.4555358795247884, -8.402594152722633325, -9.854619843455179051 ) ) ;
#30787 = CARTESIAN_POINT ( 'NONE',  ( 124.8790414775786246, -0.4660016031367893996, -10.09054647747473865 ) ) ;
#30788 = CARTESIAN_POINT ( 'NONE',  ( 119.2063748109119814, -7.894159318335828068, -9.358103419637847864 ) ) ;
#30789 = CARTESIAN_POINT ( 'NONE',  ( 124.4819548109119722, -2.084020599724378364, -8.691656652584169862 ) ) ;
#30790 = CARTESIAN_POINT ( 'NONE',  ( 125.1059481442452750, -8.166667518702819706, -8.995218007635861213 ) ) ;
#30791 = CARTESIAN_POINT ( 'NONE',  ( 115.3442858795247759, -8.402594152722688392, -9.854619843455216355 ) ) ;
#30792 = CARTESIAN_POINT ( 'NONE',  ( 124.4365102882354819, -1.135392229370316919, -17.10942237759952533 ) ) ;
#30793 = VERTEX_POINT ( 'NONE', #38786 ) ;
#30794 = CARTESIAN_POINT ( 'NONE',  ( 112.9664414775786412, 0.5811942927096154232, -14.16772938898807155 ) ) ;
#30795 = CARTESIAN_POINT ( 'NONE',  ( 121.7590748109119687, -2.084020599724406786, -8.691656652584148546 ) ) ;
#30796 = CARTESIAN_POINT ( 'NONE',  ( 118.6391081442452986, -4.089484607189486809, -7.948022111789456723 ) ) ;
#30797 = CARTESIAN_POINT ( 'NONE',  ( 116.7671281442453335, -7.643976991954077427, -18.09477374809248928 ) ) ;
#30798 = CARTESIAN_POINT ( 'NONE',  ( 119.6034614775786196, -6.344957434206665248, -7.627207830600338134 ) ) ;
#30799 = CARTESIAN_POINT ( 'NONE',  ( 70.19189222814998175, -67.83330054016514055, -40.33609291459782753 ) ) ;
#30800 = DIRECTION ( 'NONE',  ( -1.000000000000000000, 0.000000000000000000, 0.000000000000000000 ) ) ;
#30801 = CARTESIAN_POINT ( 'NONE',  ( 122.0994348109119443, -10.15424416112533912, -14.75197769757731336 ) ) ;
#30802 = ORIENTED_EDGE ( 'NONE', *, *, #37729, .T. ) ;
#30803 = LINE ( 'NONE', #3870, #20527 ) ;
#30804 = AXIS2_PLACEMENT_3D ( 'NONE', #21527, #4638, #31333 ) ;
#30805 = CARTESIAN_POINT ( 'NONE',  ( 118.6958348109119754, -6.344957434206665248, -7.627207830600338134 ) ) ;
#30806 = B_SPLINE_CURVE_WITH_KNOTS ( 'NONE', 3,
 ( #18807, #22900, #36794, #43208, #15392, #5563, #33366, #29295, #43888, #33594, #39779, #29972, #22450, #26555, #2369 ),
 .UNSPECIFIED., .F., .F.,
 ( 4, 2, 2, 1, 1, 1, 2, 2, 4 ),
 ( 0.000000000000000000, 0.2500000000002625677, 0.3750000000004022338, 0.4375000000004654055, 0.4687500000004892753, 0.4843750000005023759, 0.4921875000005089817, 0.5000000000005155876, 1.000000000000000000 ),
 .UNSPECIFIED. ) ;
#30807 = CARTESIAN_POINT ( 'NONE',  ( 125.1626748109119802, -0.1624402480850797581, -16.17319339645315424 ) ) ;
#30808 = VERTEX_POINT ( 'NONE', #7557 ) ;
#30809 = CARTESIAN_POINT ( 'NONE',  ( 121.2019704359119743, -10.25716656981731489, -12.88942061488890545 ) ) ;
#30810 = DIRECTION ( 'NONE',  ( -0.7871354856660202071, 0.6167752151498580027, 0.002461946824133919541 ) ) ;
#30811 = CARTESIAN_POINT ( 'NONE',  ( 119.3198281442452924, 0.5811942927096110934, -14.16772938898807510 ) ) ;
#30812 = CARTESIAN_POINT ( 'NONE',  ( 108.3989733795248753, -8.938348069036489818, -17.46756447353520159 ) ) ;
#30813 = CARTESIAN_POINT ( 'NONE',  ( 118.0718414775786442, -0.8288870151387760510, -10.36305467784173118 ) ) ;
#30814 = ORIENTED_EDGE ( 'NONE', *, *, #4404, .T. ) ;
#30815 = AXIS2_PLACEMENT_3D ( 'NONE', #35442, #29067, #1024 ) ;
#30816 = ORIENTED_EDGE ( 'NONE', *, *, #19032, .F. ) ;
#30817 = CARTESIAN_POINT ( 'NONE',  ( 124.2550481442452792, -0.1624402480850797581, -16.17319339645315424 ) ) ;
#30818 = CARTESIAN_POINT ( 'NONE',  ( 125.5597614775786326, -7.894159318335828068, -9.358103419637847864 ) ) ;
#30819 = FACE_OUTER_BOUND ( 'NONE', #24306, .T. ) ;
#30820 = CARTESIAN_POINT ( 'NONE',  ( 123.9584548109119737, -4.863998795839242995, -13.39321520033831447 ) ) ;
#30821 = CARTESIAN_POINT ( 'NONE',  ( 120.2274548109119934, 0.5811942927096110934, -14.16772938898807510 ) ) ;
#30822 = CARTESIAN_POINT ( 'NONE',  ( 111.7184548109119788, -9.244942279156937559, -16.71734234406761388 ) ) ;
#30823 = LINE ( 'NONE', #27413, #20797 ) ;
#30824 = CARTESIAN_POINT ( 'NONE',  ( 119.3198281442452924, 0.5811942927096110934, -14.16772938898807510 ) ) ;
#30826 = CARTESIAN_POINT ( 'NONE',  ( 121.0216281442452981, -7.894159318335828068, -9.358103419637847864 ) ) ;
#30825 = CARTESIAN_POINT ( 'NONE',  ( 118.7525614775786380, -8.166667518702819706, -8.995218007635861213 ) ) ;
#30827 =( BOUNDED_SURFACE ( )  B_SPLINE_SURFACE ( 1, 2, ( 
 ( #41811, #18069, #13765, #27674, #27450, #41373, #42245, #20824, #11010, #17625, #28118, #31519, #6700, #24032, #38806, #7575, #69, #42025, #7349, #37923, #41589, #24254, #38143, #6917, #34704, #28564, #7808, #8480, #22384, #8027, #726, #32188, #8700, #14876, #39265, #29230, #18962, #32636, #42471, #43136, #42694, #29448, #21717, #43363, #36280, #18293, #11464, #18521, #39492, #1402, #14649, #11234, #39939, #19194, #15542, #26034, #25367, #11906, #32852, #28789, #12131, #25807, #15318, #21935, #25143 ),
 ( #11681, #35826, #5047, #1623, #960, #4600, #22161, #25588, #36055, #32413, #36505, #39036, #35602, #18745, #42917, #4375, #22605, #1186, #15099, #8255, #29008, #4822, #39716, #5275, #44495, #26713, #30575, #26257, #30355, #29904, #1844, #5947, #15772, #40167, #40854, #9609, #40395, #33072, #19412, #41086, #2075, #26490, #16455, #6183, #19870, #29675, #44281, #43821, #16683, #8930, #13260, #23526, #5492, #12586, #5718, #40622, #33759, #43587, #12357, #27165, #6418, #2757, #9844, #9159, #13034 ) ),
 .UNSPECIFIED., .F., .F., .T. ) 
 B_SPLINE_SURFACE_WITH_KNOTS ( ( 2, 2 ),
 ( 3, 2, 2, 2, 2, 2, 2, 2, 2, 2, 2, 2, 2, 2, 2, 2, 2, 2, 2, 2, 2, 2, 2, 2, 2, 2, 2, 2, 2, 2, 2, 2, 3 ),
 ( 0.000000000000000000, 1.000000000000000000 ),
 ( 0.000000000000000000, 0.03125000000000000000, 0.06250000000000000000, 0.09375000000000000000, 0.1250000000000000000, 0.1562500000000000000, 0.1875000000000000000, 0.2187500000000000000, 0.2500000000000000000, 0.2812500000000000000, 0.3125000000000000000, 0.3437500000000000000, 0.3750000000000000000, 0.4062500000000000000, 0.4375000000000000000, 0.4687500000000000000, 0.5000000000000000000, 0.5312500000000000000, 0.5625000000000000000, 0.5937500000000000000, 0.6250000000000000000, 0.6562500000000000000, 0.6875000000000000000, 0.7187500000000000000, 0.7500000000000000000, 0.7812500000000000000, 0.8125000000000000000, 0.8437500000000000000, 0.8750000000000000000, 0.9062500000000000000, 0.9375000000000000000, 0.9687500000000000000, 1.000000000000000000 ),
 .UNSPECIFIED. ) 
 GEOMETRIC_REPRESENTATION_ITEM ( )  RATIONAL_B_SPLINE_SURFACE ( (
 ( 1.000000000000000000, 0.9238795325112869605, 1.000000000000000000, 0.9238795325112869605, 1.000000000000000000, 0.9238795325112869605, 1.000000000000000000, 0.9238795325112869605, 1.000000000000000000, 0.9238795325112869605, 1.000000000000000000, 0.9238795325112869605, 1.000000000000000000, 0.9238795325112869605, 1.000000000000000000, 0.9238795325112869605, 1.000000000000000000, 0.9238795325112869605, 1.000000000000000000, 0.9238795325112869605, 1.000000000000000000, 0.9238795325112869605, 1.000000000000000000, 0.9238795325112869605, 1.000000000000000000, 0.9238795325112869605, 1.000000000000000000, 0.9238795325112869605, 1.000000000000000000, 0.9238795325112869605, 1.000000000000000000, 0.9238795325112869605, 1.000000000000000000, 0.9238795325112869605, 1.000000000000000000, 0.9238795325112869605, 1.000000000000000000, 0.9238795325112869605, 1.000000000000000000, 0.9238795325112869605, 1.000000000000000000, 0.9238795325112869605, 1.000000000000000000, 0.9238795325112869605, 1.000000000000000000, 0.9238795325112869605, 1.000000000000000000, 0.9238795325112869605, 1.000000000000000000, 0.9238795325112869605, 1.000000000000000000, 0.9238795325112869605, 1.000000000000000000, 0.9238795325112869605, 1.000000000000000000, 0.9238795325112869605, 1.000000000000000000, 0.9238795325112869605, 1.000000000000000000, 0.9238795325112869605, 1.000000000000000000, 0.9238795325112869605, 1.000000000000000000, 0.9238795325112869605, 1.000000000000000000),
 ( 1.000000000000000000, 0.9238795325112869605, 1.000000000000000000, 0.9238795325112869605, 1.000000000000000000, 0.9238795325112869605, 1.000000000000000000, 0.9238795325112869605, 1.000000000000000000, 0.9238795325112869605, 1.000000000000000000, 0.9238795325112869605, 1.000000000000000000, 0.9238795325112869605, 1.000000000000000000, 0.9238795325112869605, 1.000000000000000000, 0.9238795325112869605, 1.000000000000000000, 0.9238795325112869605, 1.000000000000000000, 0.9238795325112869605, 1.000000000000000000, 0.9238795325112869605, 1.000000000000000000, 0.9238795325112869605, 1.000000000000000000, 0.9238795325112869605, 1.000000000000000000, 0.9238795325112869605, 1.000000000000000000, 0.9238795325112869605, 1.000000000000000000, 0.9238795325112869605, 1.000000000000000000, 0.9238795325112869605, 1.000000000000000000, 0.9238795325112869605, 1.000000000000000000, 0.9238795325112869605, 1.000000000000000000, 0.9238795325112869605, 1.000000000000000000, 0.9238795325112869605, 1.000000000000000000, 0.9238795325112869605, 1.000000000000000000, 0.9238795325112869605, 1.000000000000000000, 0.9238795325112869605, 1.000000000000000000, 0.9238795325112869605, 1.000000000000000000, 0.9238795325112869605, 1.000000000000000000, 0.9238795325112869605, 1.000000000000000000, 0.9238795325112869605, 1.000000000000000000, 0.9238795325112869605, 1.000000000000000000, 0.9238795325112869605, 1.000000000000000000, 0.9238795325112869605, 1.000000000000000000) ) ) 
 REPRESENTATION_ITEM ( '' )  SURFACE ( )  );
#30828 = CARTESIAN_POINT ( 'NONE',  ( 109.2294421295247844, -9.051693226400931991, -21.89321520033831447 ) ) ;
#30829 = CARTESIAN_POINT ( 'NONE',  ( 117.6180281442453150, -0.4660016031367893996, -10.09054647747474043 ) ) ;
#30830 = ORIENTED_EDGE ( 'NONE', *, *, #19307, .T. ) ;
#30831 = CARTESIAN_POINT ( 'NONE',  ( 123.7445081442452874, -7.894159318335828068, -9.358103419637847864 ) ) ;
#30832 = CARTESIAN_POINT ( 'NONE',  ( 116.0831764669098760, -0.01868118798763890309, -12.14321520033834290 ) ) ;
#30833 = CARTESIAN_POINT ( 'NONE',  ( 110.5520202545248054, -10.62599879583958717, -15.77991374673208469 ) ) ;
#30834 = CARTESIAN_POINT ( 'NONE',  ( 113.6774108795247997, -1.325403438956436419, -16.93181055722141792 ) ) ;
#30835 = CARTESIAN_POINT ( 'NONE',  ( 115.8304577545247582, -2.791137627527939813, -18.39754474579286025 ) ) ;
#30836 = CARTESIAN_POINT ( 'NONE',  ( 121.1350814775786233, 0.5811942927096110934, -14.16772938898807510 ) ) ;
#30837 = CARTESIAN_POINT ( 'NONE',  ( 123.5176014775786228, -0.8288870151387760510, -10.36305467784173118 ) ) ;
#30838 = ORIENTED_EDGE ( 'NONE', *, *, #14986, .T. ) ;
#30839 = CARTESIAN_POINT ( 'NONE',  ( 123.3474214775786209, -9.988377603198976828, -10.36322818467138340 ) ) ;
#30840 = CARTESIAN_POINT ( 'NONE',  ( 112.5661608795247872, -8.938348069036489818, -9.318865927141430916 ) ) ;
#30841 = CARTESIAN_POINT ( 'NONE',  ( 113.1366214775786432, -7.643976991954077427, -18.09477374809248928 ) ) ;
#30842 = PLANE ( 'NONE',  #13956 ) ;
#30843 = CARTESIAN_POINT ( 'NONE',  ( 124.8223148109119762, 0.9020085738987339008, -11.91225656197089222 ) ) ;
#30844 = CARTESIAN_POINT ( 'NONE',  ( 119.8303681442453126, -10.63000616557722466, -14.87417383870573495 ) ) ;
#30845 = CARTESIAN_POINT ( 'NONE',  ( 120.0907204359119760, -10.25716656981731489, -12.88942061488890545 ) ) ;
#30846 = CARTESIAN_POINT ( 'NONE',  ( 112.8529881442453302, -1.561330072975668060, -17.79121239304076596 ) ) ;
#30847 = LINE ( 'NONE', #16500, #24810 ) ;
#30848 = CARTESIAN_POINT ( 'NONE',  ( 106.2459265045248173, -7.250697342233347165, -19.15521520033831138 ) ) ;
#30849 = ORIENTED_EDGE ( 'NONE', *, *, #24771, .T. ) ;
#30850 = VECTOR ( 'NONE', #42141, 1000.000000000000000 ) ;
#30851 = CARTESIAN_POINT ( 'NONE',  ( 124.7895009388149248, -2.287189184988705826, -18.07361239780448159 ) ) ;
#30852 = CARTESIAN_POINT ( 'NONE',  ( 113.4769814775786330, 0.4262465694468514643, -12.03445270309931736 ) ) ;
#30853 = CARTESIAN_POINT ( 'NONE',  ( 124.0281414775786146, -7.643976991954077427, -18.09477374809248928 ) ) ;
#30854 = CARTESIAN_POINT ( 'NONE',  ( 108.2600671295247992, 0.1403307496149613920, -13.39321520033831447 ) ) ;
#30855 = CARTESIAN_POINT ( 'NONE',  ( 106.5931921295248372, -9.868328341294093420, -13.39321520033831447 ) ) ;
#30856 = CARTESIAN_POINT ( 'NONE',  ( 122.8368814775786291, -7.894159318335828068, -9.358103419637847864 ) ) ;
#30857 = CARTESIAN_POINT ( 'NONE',  ( 115.2355081442453155, 0.1319031606808879209, -14.10382304977623669 ) ) ;
#30858 = CARTESIAN_POINT ( 'NONE',  ( 112.6828081442453282, -2.084020599724406786, -8.691656652584148546 ) ) ;
#30859 = VERTEX_POINT ( 'NONE', #7789 ) ;
#30860 = ADVANCED_FACE ( 'NONE', ( #39019, #34897 ), #25123, .F. ) ;
#30861 = CARTESIAN_POINT ( 'NONE',  ( 120.9081748109119872, -4.153390946401325223, -8.397313243818185668 ) ) ;
#30862 = CARTESIAN_POINT ( 'NONE',  ( 117.9583881442453048, -10.30919188438810075, -12.61870101168855918 ) ) ;
#30863 = LINE ( 'NONE', #17408, #22978 ) ;
#30864 = ORIENTED_EDGE ( 'NONE', *, *, #24838, .F. ) ;
#30865 = CARTESIAN_POINT ( 'NONE',  ( 120.8547048109119686, -2.527210466738041283, -8.967976844669125924 ) ) ;
#30866 = CIRCLE ( 'NONE', #7581, 5.000000000000004441 ) ;
#30867 = ORIENTED_EDGE ( 'NONE', *, *, #13050, .F. ) ;
#30868 = CARTESIAN_POINT ( 'NONE',  ( 115.4056881442453459, -2.084020599724406786, -8.691656652584148546 ) ) ;
#30869 = CARTESIAN_POINT ( 'NONE',  ( 113.7038881442453402, -6.222761293078241884, -8.102969835052219238 ) ) ;
#30870 = EDGE_CURVE ( 'NONE', #4363, #34274, #14180, .T. ) ;
#30871 = CARTESIAN_POINT ( 'NONE',  ( 128.2184548109119930, -7.252096815532139473, -18.89748516540533529 ) ) ;
#30872 = EDGE_CURVE ( 'NONE', #34542, #22604, #21472, .T. ) ;
#30873 = EDGE_CURVE ( 'NONE', #14918, #16653, #20806, .T. ) ;
#30874 = CARTESIAN_POINT ( 'NONE',  ( 122.5910329359119970, -5.367793381288652910, -18.78638297431638904 ) ) ;
#30875 = VERTEX_POINT ( 'NONE', #13964 ) ;
#30876 = DIRECTION ( 'NONE',  ( 0.9609149988134843001, -0.1028163501681632064, 0.2570431154366505933 ) ) ;
#30877 = CARTESIAN_POINT ( 'NONE',  ( 67.30914723170953096, -52.30871106904351819, -35.02081913341498165 ) ) ;
#30878 = CARTESIAN_POINT ( 'NONE',  ( 114.1635827545248389, -2.477300249445798297, -19.15521520033831138 ) ) ;
#30879 = DIRECTION ( 'NONE',  ( 0.000000000000000000, -0.9242245927363029745, -0.3818493186865927758 ) ) ;
#30880 = CARTESIAN_POINT ( 'NONE',  ( 124.7655881442452852, -9.859900752359378018, -12.68260735090039759 ) ) ;
#30881 = CARTESIAN_POINT ( 'NONE',  ( 113.3068014775786594, -1.833838273342658809, -17.42832698103878286 ) ) ;
#30882 = CARTESIAN_POINT ( 'NONE',  ( 125.5030348109119558, -6.222761293078236555, -8.102969835052215686 ) ) ;
#30883 = ORIENTED_EDGE ( 'NONE', *, *, #11364, .T. ) ;
#30884 = DIRECTION ( 'NONE',  ( -1.000000000000000000, 0.000000000000000000, -0.000000000000000000 ) ) ;
#30885 = CARTESIAN_POINT ( 'NONE',  ( 70.19189222814998175, -56.33107134722149567, -35.73524133214168330 ) ) ;
#30886 = CARTESIAN_POINT ( 'NONE',  ( 111.9228860982116913, 0.3867979994853637526, -12.14321520033831625 ) ) ;
#30887 = CARTESIAN_POINT ( 'NONE',  ( 112.0126281442453120, -9.814174330883659536, -12.68911139247490105 ) ) ;
#30889 = DIRECTION ( 'NONE',  ( 0.000000000000000000, 0.000000000000000000, -1.000000000000000000 ) ) ;
#30888 = CARTESIAN_POINT ( 'NONE',  ( 65.54186577906706646, -36.42801838861263519, -5.470407532193676481 ) ) ;
#30890 = CARTESIAN_POINT ( 'NONE',  ( 124.7655881442452852, -9.859900752359378018, -12.68260735090039759 ) ) ;
#30891 = ORIENTED_EDGE ( 'NONE', *, *, #33209, .F. ) ;
#30892 = CARTESIAN_POINT ( 'NONE',  ( 115.0653281442453277, -6.344957434206662583, -7.627207830600332805 ) ) ;
#30893 = CARTESIAN_POINT ( 'NONE',  ( 126.9276200068715497, 0.2063212325922000601, -15.11478432700113395 ) ) ;
#30894 = CARTESIAN_POINT ( 'NONE',  ( 116.1082702545247827, -10.62599879583958717, -15.77991374673208469 ) ) ;
#30895 = CARTESIAN_POINT ( 'NONE',  ( 125.6164881442453094, -9.565557343593413364, -10.61323700422348004 ) ) ;
#30896 = CARTESIAN_POINT ( 'NONE',  ( 123.0637881442452937, -8.899110576539710493, -16.42337572283490132 ) ) ;
#30897 = CARTESIAN_POINT ( 'NONE',  ( 125.4584548109119737, -8.963735245270648022, -18.43723750849711962 ) ) ;
#30898 = CARTESIAN_POINT ( 'NONE',  ( 114.9970202545248412, 0.1403307496149616695, -11.32035403202665336 ) ) ;
#30899 = EDGE_CURVE ( 'NONE', #23226, #6624, #27875, .T. ) ;
#30900 = CARTESIAN_POINT ( 'NONE',  ( 111.5243640045248412, -10.62599879583958540, -11.00651665394455492 ) ) ;
#30901 = CARTESIAN_POINT ( 'NONE',  ( 109.2296643047792060, -2.144085356277730448, -17.65426957299811761 ) ) ;
#30902 = CARTESIAN_POINT ( 'NONE',  ( 112.5693548109119888, 0.4262465694468514643, -12.03445270309931736 ) ) ;
#30903 = CARTESIAN_POINT ( 'NONE',  ( 106.8015515045248378, -2.477300249445798297, -7.631215200338321125 ) ) ;
#30904 = CYLINDRICAL_SURFACE ( 'NONE', #29180, 8.000000000000001776 ) ;
#30905 = CARTESIAN_POINT ( 'NONE',  ( 110.4131140045248287, -10.62599879583958717, -11.00651665394454604 ) ) ;
#30906 = CARTESIAN_POINT ( 'NONE',  ( 124.7655881442452852, 0.5811942927096110934, -14.16772938898807510 ) ) ;
#30907 = CARTESIAN_POINT ( 'NONE',  ( 125.2761281442453054, -10.63000616557722466, -14.87417383870573495 ) ) ;
#30908 = CARTESIAN_POINT ( 'NONE',  ( 114.4099712410415748, 0.7607806665037644134, -12.14321520033829316 ) ) ;
#30909 = EDGE_CURVE ( 'NONE', #41111, #14177, #7329, .T. ) ;
#30910 = CARTESIAN_POINT ( 'NONE',  ( 120.8514481442452961, -7.893985811506177619, -18.51759400769804742 ) ) ;
#30911 = CARTESIAN_POINT ( 'NONE',  ( 113.7038881442453402, -3.383040157471821630, -19.15922257007629170 ) ) ;
#30912 = ORIENTED_EDGE ( 'NONE', *, *, #17126, .F. ) ;
#30913 = CARTESIAN_POINT ( 'NONE',  ( 114.2711548109119803, -0.1624402480850797581, -16.17319339645315424 ) ) ;
#30914 = EDGE_CURVE ( 'NONE', #11839, #30808, #12192, .T. ) ;
#30915 = CARTESIAN_POINT ( 'NONE',  ( 125.8433948109119456, -1.834011780172310813, -8.268836392978581529 ) ) ;
#30916 = CARTESIAN_POINT ( 'NONE',  ( 125.2194014775786286, -10.30919188438810075, -12.61870101168855918 ) ) ;
#30917 = CARTESIAN_POINT ( 'NONE',  ( 113.7038881442453402, -3.383040157471821630, -19.15922257007629170 ) ) ;
#30918 = SHAPE_REPRESENTATION ( 'Body4', ( #12375 ), #19397 ) ;
#30919 = CARTESIAN_POINT ( 'NONE',  ( 116.0864081442453113, -0.1624402480850797581, -16.17319339645315424 ) ) ;
#30920 = ORIENTED_EDGE ( 'NONE', *, *, #31239, .T. ) ;
#30921 = CARTESIAN_POINT ( 'NONE',  ( 118.3554748109119998, -9.565557343593413364, -10.61323700422348004 ) ) ;
#30922 = CARTESIAN_POINT ( 'NONE',  ( 125.4463081442452932, -4.153390946401325223, -8.397313243818185668 ) ) ;
#30923 = CARTESIAN_POINT ( 'NONE',  ( 124.1221766859119811, -0.6978242514986119360, -9.938897388174531500 ) ) ;
#30924 = CARTESIAN_POINT ( 'NONE',  ( 114.3024890045248156, 0.8980012041604421569, -15.77991374673208469 ) ) ;
#30925 = ORIENTED_EDGE ( 'NONE', *, *, #18739, .T. ) ;
#30926 = ADVANCED_FACE ( 'NONE', ( #33053 ), #15757, .F. ) ;
#30927 = EDGE_CURVE ( 'NONE', #2865, #44361, #42343, .T. ) ;
#30928 = EDGE_CURVE ( 'NONE', #40557, #39765, #29966, .T. ) ;
#30929 = CIRCLE ( 'NONE', #34523, 2.999999999999999556 ) ;
#30930 = DIRECTION ( 'NONE',  ( 0.07634843047859296572, 0.9970811988817437355, 0.000000000000000000 ) ) ;
#30931 = CARTESIAN_POINT ( 'NONE',  ( 92.26512299712632625, -23.76310523276723785, -21.89321520033831447 ) ) ;
#30932 = DIRECTION ( 'NONE',  ( 1.000000000000000000, 0.000000000000000000, -0.000000000000000000 ) ) ;
#30933 = B_SPLINE_CURVE_WITH_KNOTS ( 'NONE', 3,
 ( #14124, #3417, #31442, #41949, #6845, #20752, #34631, #17333, #31664, #657 ),
 .UNSPECIFIED., .F., .F.,
 ( 4, 3, 3, 4 ),
 ( 0.000000000000000000, 0.0001671877560958089928, 0.0003343755126086520144, 0.0006438490228507220145 ),
 .UNSPECIFIED. ) ;
#30934 = CARTESIAN_POINT ( 'NONE',  ( 116.0286950891469786, 2.331313199634366118, -6.893215200338315363 ) ) ;
#30935 = CARTESIAN_POINT ( 'NONE',  ( 112.7395348109119766, -4.153390946401321671, -8.397313243818183892 ) ) ;
#30936 = CARTESIAN_POINT ( 'NONE',  ( 107.9822546295247889, -4.863998795839590272, -18.39754474579285315 ) ) ;
#30937 = DIRECTION ( 'NONE',  ( 1.000000000000000000, 0.000000000000000000, -0.000000000000000000 ) ) ;
#30938 = CARTESIAN_POINT ( 'NONE',  ( 116.9940348109119839, -9.988377603198976828, -10.36322818467138340 ) ) ;
#30939 = CARTESIAN_POINT ( 'NONE',  ( 136.4340220207345169, -4.240043735563310712, -19.13645151290679536 ) ) ;
#30940 = CARTESIAN_POINT ( 'NONE',  ( 111.2184548109119788, -4.863998795839242995, -13.39321520033831447 ) ) ;
#30941 = FACE_OUTER_BOUND ( 'NONE', #8376, .T. ) ;
#30942 = CARTESIAN_POINT ( 'NONE',  ( 121.4187148109119789, -3.505236298600246325, -18.68346056562440793 ) ) ;
#30943 = ORIENTED_EDGE ( 'NONE', *, *, #26428, .F. ) ;
#30944 = CARTESIAN_POINT ( 'NONE',  ( 136.5278073584882463, -9.320078359935157764, -9.779958153336949067 ) ) ;
#30945 = CARTESIAN_POINT ( 'NONE',  ( 118.0718414775786300, -9.261995988541697145, -16.69588392320189030 ) ) ;
#30946 = CARTESIAN_POINT ( 'NONE',  ( 69.36136150295220659, -101.1685209014307674, -50.56525720990386219 ) ) ;
#30947 = CARTESIAN_POINT ( 'NONE',  ( 116.0864081442453113, -0.1624402480850797581, -16.17319339645315424 ) ) ;
#30948 = CARTESIAN_POINT ( 'NONE',  ( 114.1009748109119784, -5.574606645277164318, -18.38911715685844683 ) ) ;
#30949 = CARTESIAN_POINT ( 'NONE',  ( 109.5796765045248122, -7.250697342233347165, -19.15521520033831138 ) ) ;
#30950 = CARTESIAN_POINT ( 'NONE',  ( 87.68939540009954214, -25.99489077589524300, -13.39321520033831447 ) ) ;
#30951 = CARTESIAN_POINT ( 'NONE',  ( 115.4137390045248566, 0.8980012041604421569, -15.77991374673208469 ) ) ;
#30952 = CONICAL_SURFACE ( 'NONE', #36753, 2.999999999999999556, 0.9599310885968830309 ) ;
#30953 = CARTESIAN_POINT ( 'NONE',  ( 114.9518748109119883, -7.643976991954077427, -18.09477374809248928 ) ) ;
#30954 = CARTESIAN_POINT ( 'NONE',  ( 120.1140014775786398, -7.894159318335828068, -9.358103419637847864 ) ) ;
#30955 = CARTESIAN_POINT ( 'NONE',  ( 96.21525317080913453, -27.22866758126576059, -11.75569266233354426 ) ) ;
#30956 = CARTESIAN_POINT ( 'NONE',  ( 121.0630641859119976, -0.8832429491016019485, -18.19431474523657855 ) ) ;
#30957 = CARTESIAN_POINT ( 'NONE',  ( 111.2465515045248168, -6.936859964151250502, -18.39754474579286025 ) ) ;
#30958 = FACE_OUTER_BOUND ( 'NONE', #27573, .T. ) ;
#30959 = CARTESIAN_POINT ( 'NONE',  ( 112.2857214775786474, -4.089484607189486809, -7.948022111789456723 ) ) ;
#30960 = CARTESIAN_POINT ( 'NONE',  ( 115.4056881442453459, -7.893985811506177619, -18.51759400769804742 ) ) ;
#30961 = DIRECTION ( 'NONE',  ( -0.6383198453882299450, -0.7697712484781087383, 0.000000000000000000 ) ) ;
#30962 = CARTESIAN_POINT ( 'NONE',  ( 119.8129079359119942, -4.360204210389833968, -8.000047426360245240 ) ) ;
#30963 = ORIENTED_EDGE ( 'NONE', *, *, #3827, .T. ) ;
#30964 = CARTESIAN_POINT ( 'NONE',  ( 123.4728812494079335, -2.843354789049347797, -14.83501475315878260 ) ) ;
#30965 = CONICAL_SURFACE ( 'NONE', #14915, 2.000000000000000444, 0.9599310885968830309 ) ;
#30966 = EDGE_LOOP ( 'NONE', ( #4852, #41015, #15297, #5199, #4682 ) ) ;
#30967 = CARTESIAN_POINT ( 'NONE',  ( 121.7590748109119687, -7.893985811506177619, -18.51759400769804742 ) ) ;
#30968 = CARTESIAN_POINT ( 'NONE',  ( 111.7751814775786556, -7.893985811506177619, -18.51759400769804742 ) ) ;
#30969 = CARTESIAN_POINT ( 'NONE',  ( 117.5613014775786525, -10.15424416112533912, -14.75197769757731336 ) ) ;
#30970 = DIRECTION ( 'NONE',  ( -1.000000000000000000, 0.000000000000000000, 0.000000000000000000 ) ) ;
#30971 = CARTESIAN_POINT ( 'NONE',  ( 122.3830681442452857, -8.166667518702819706, -8.995218007635861213 ) ) ;
#30972 = CARTESIAN_POINT ( 'NONE',  ( 117.7882081442453170, -6.344957434206665248, -7.627207830600338134 ) ) ;
#30973 = ADVANCED_FACE ( 'NONE', ( #1385 ), #1827, .T. ) ;
#30974 = CARTESIAN_POINT ( 'NONE',  ( 106.3153796295248412, -4.863998795839590272, -8.388885654883775800 ) ) ;
#30975 = CARTESIAN_POINT ( 'NONE',  ( 111.5482748109120053, -0.1624402480850797581, -16.17319339645315424 ) ) ;
#30976 = DIRECTION ( 'NONE',  ( 0.000000000000000000, 0.000000000000000000, -1.000000000000000000 ) ) ;
#30977 = VERTEX_POINT ( 'NONE', #5475 ) ;
#30978 = CARTESIAN_POINT ( 'NONE',  ( 119.0929214775786278, -5.638512984488999180, -18.83840828888717311 ) ) ;
#30979 = CARTESIAN_POINT ( 'NONE',  ( -13.56828337869051104, -4.779084862086335761, -17.89321520033831447 ) ) ;
#30980 = CARTESIAN_POINT ( 'NONE',  ( 115.5758681442453053, -1.561330072975668060, -17.79121239304076951 ) ) ;
#30981 = AXIS2_PLACEMENT_3D ( 'NONE', #20788, #3455, #17372 ) ;
#30982 = ORIENTED_EDGE ( 'NONE', *, *, #36698, .F. ) ;
#30983 = CARTESIAN_POINT ( 'NONE',  ( 115.1359265045248605, -7.250697342233347165, -19.15521520033831138 ) ) ;
#30984 = CARTESIAN_POINT ( 'NONE',  ( 111.0762212410415799, 0.7607806665037644134, -12.14321520033829316 ) ) ;
#30985 = DIRECTION ( 'NONE',  ( 0.000000000000000000, 0.000000000000000000, -1.000000000000000000 ) ) ;
#30986 = DIRECTION ( 'NONE',  ( -0.8853218534579893051, 0.4649787261689617979, 0.000000000000000000 ) ) ;
#30987 = CARTESIAN_POINT ( 'NONE',  ( 78.05848382472312608, -57.67750005573411443, -0.9577251715239786245 ) ) ;
#30988 = EDGE_CURVE ( 'NONE', #32530, #33236, #12494, .T. ) ;
#30989 = CARTESIAN_POINT ( 'NONE',  ( 117.2776681442452968, -4.153390946401325223, -8.397313243818185668 ) ) ;
#30990 = CIRCLE ( 'NONE', #3326, 1.587500000000000355 ) ;
#30991 = CARTESIAN_POINT ( 'NONE',  ( 116.9940348109119839, -0.1624402480850797581, -16.17319339645315424 ) ) ;
#30992 = DIRECTION ( 'NONE',  ( -0.9609149988134837450, 0.1028163501681639419, -0.2570431154366518145 ) ) ;
#30993 = CARTESIAN_POINT ( 'NONE',  ( 117.5613014775786525, -10.15424416112533912, -14.75197769757731336 ) ) ;
#30994 = CARTESIAN_POINT ( 'NONE',  ( 123.0077516859119839, -9.665098340737509730, -17.37397104707595474 ) ) ;
#30995 = CARTESIAN_POINT ( 'NONE',  ( 115.9162281442453235, -4.089484607189486809, -7.948022111789456723 ) ) ;
#30996 = CARTESIAN_POINT ( 'NONE',  ( 111.6050014775786536, 0.1319031606808879209, -14.10382304977623669 ) ) ;
#30997 = CARTESIAN_POINT ( 'NONE',  ( 118.0718414775786442, -0.8288870151387760510, -10.36305467784173118 ) ) ;
#30998 = VERTEX_POINT ( 'NONE', #39474 ) ;
#30999 = CARTESIAN_POINT ( 'NONE',  ( 117.2209414775786485, -7.893985811506177619, -18.51759400769804742 ) ) ;
#31000 = CARTESIAN_POINT ( 'NONE',  ( 106.0375671295248310, -10.62599879583958540, -13.39321520033831447 ) ) ;
#31001 = DIRECTION ( 'NONE',  ( 0.000000000000000000, -0.3713878862591665220, 0.9284778069183713400 ) ) ;
#31002 = CARTESIAN_POINT ( 'NONE',  ( 105.2041296295248287, -4.863998795839590272, -8.388885654883775800 ) ) ;
#31003 = CARTESIAN_POINT ( 'NONE',  ( 127.9650921473015330, -4.196254079835942008, -15.53128073880881388 ) ) ;
#31004 = CARTESIAN_POINT ( 'NONE',  ( 121.1350814775786233, 0.5811942927096110934, -14.16772938898807510 ) ) ;
#31005 = ORIENTED_EDGE ( 'NONE', *, *, #34499, .T. ) ;
#31006 = CARTESIAN_POINT ( 'NONE',  ( 87.80477198183443477, -25.23119213852205789, -15.24166438581092109 ) ) ;
#31007 = CARTESIAN_POINT ( 'NONE',  ( 119.4900081442453086, -7.643976991954077427, -18.09477374809248928 ) ) ;
#31008 = CARTESIAN_POINT ( 'NONE',  ( 123.4041481442452834, -10.30919188438810075, -12.61870101168855918 ) ) ;
#31009 = CARTESIAN_POINT ( 'NONE',  ( 107.1488171295247867, -10.62599879583958540, -13.39321520033831447 ) ) ;
#31010 = CARTESIAN_POINT ( 'NONE',  ( 89.26958058349273983, -9.992926966327468463, -13.67320616139556400 ) ) ;
#31011 = VERTEX_POINT ( 'NONE', #29431 ) ;
#31012 = CARTESIAN_POINT ( 'NONE',  ( 111.9453614775786434, -1.561330072975668060, -17.79121239304076596 ) ) ;
#31013 = CARTESIAN_POINT ( 'NONE',  ( 111.8886348109120092, -3.383040157471821630, -19.15922257007629170 ) ) ;
#31014 = CARTESIAN_POINT ( 'NONE',  ( 123.4041481442452834, -10.30919188438810075, -12.61870101168855918 ) ) ;
#31015 = CARTESIAN_POINT ( 'NONE',  ( 115.9162281442453235, -5.574606645277164318, -18.38911715685844683 ) ) ;
#31016 = FACE_OUTER_BOUND ( 'NONE', #20027, .T. ) ;
#31017 = CARTESIAN_POINT ( 'NONE',  ( 118.7525614775786380, -8.166667518702819706, -8.995218007635861213 ) ) ;
#31018 = LINE ( 'NONE', #27386, #5274 ) ;
#31019 = CARTESIAN_POINT ( 'NONE',  ( 124.4819548109119722, -2.084020599724406786, -8.691656652584148546 ) ) ;
#31020 = EDGE_LOOP ( 'NONE', ( #33468, #12467, #5472, #40943 ) ) ;
#31021 = CIRCLE ( 'NONE', #11366, 6.426280380454326036 ) ;
#31022 = CARTESIAN_POINT ( 'NONE',  ( 87.62389663665700823, -12.03403077406018440, -16.89321520033831447 ) ) ;
#31023 = CARTESIAN_POINT ( 'NONE',  ( 117.9016614775786280, -9.988377603198976828, -10.36322818467138340 ) ) ;
#31024 = CARTESIAN_POINT ( 'NONE',  ( 135.5837700375877262, -8.533490405816159807, -18.12891336820539934 ) ) ;
#31025 = ORIENTED_EDGE ( 'NONE', *, *, #2542, .T. ) ;
#31026 = CARTESIAN_POINT ( 'NONE',  ( 120.1601735609119856, 0.6414057260225851653, -11.69287257290600657 ) ) ;
#31027 = CARTESIAN_POINT ( 'NONE',  ( 41.72636039845269096, -11.37347657059392070, -19.39321520033831447 ) ) ;
#31028 = CARTESIAN_POINT ( 'NONE',  ( 121.9292548109119849, -1.561330072975668948, -17.79121239304076951 ) ) ;
#31029 = CARTESIAN_POINT ( 'NONE',  ( 106.9404577545248145, -7.250697342233347165, -7.631215200338321125 ) ) ;
#31030 = CARTESIAN_POINT ( 'NONE',  ( 120.5110881442453206, -3.505236298600246325, -18.68346056562440793 ) ) ;
#31031 = ORIENTED_EDGE ( 'NONE', *, *, #24530, .T. ) ;
#31032 = ORIENTED_EDGE ( 'NONE', *, *, #2823, .T. ) ;
#31033 = CARTESIAN_POINT ( 'NONE',  ( 114.3846081442453197, -10.63000616557722466, -14.87417383870573495 ) ) ;
#31034 = ADVANCED_FACE ( 'NONE', ( #18727 ), #19058, .T. ) ;
#31035 = CIRCLE ( 'NONE', #28182, 6.426280380454326036 ) ;
#31036 = DIRECTION ( 'NONE',  ( 0.000000000000000000, -0.3818493186865927203, 0.9242245927363029745 ) ) ;
#31037 = SURFACE_SIDE_STYLE ('',( #10307 ) ) ;
#31038 = CARTESIAN_POINT ( 'NONE',  ( 63.69189222814998175, -57.16572941273946640, -4.036072343195455936 ) ) ;
#31039 = CARTESIAN_POINT ( 'NONE',  ( 122.7234281442452755, -5.638512984488999180, -18.83840828888717311 ) ) ;
#31040 = DIRECTION ( 'NONE',  ( -0.000000000000000000, -0.9284778069183721172, -0.3713878862591650232 ) ) ;
#31041 = CARTESIAN_POINT ( 'NONE',  ( 69.69189222814998175, -41.76310523276723785, -24.89321520033831447 ) ) ;
#31042 = CARTESIAN_POINT ( 'NONE',  ( 121.5888948109119809, -10.30919188438810075, -12.61870101168855918 ) ) ;
#31044 = CARTESIAN_POINT ( 'NONE',  ( 117.9583881442453048, 0.1319031606808879209, -14.10382304977623669 ) ) ;
#31043 = CARTESIAN_POINT ( 'NONE',  ( 117.9583881442453048, -10.30919188438810075, -12.61870101168855918 ) ) ;
#31045 = DIRECTION ( 'NONE',  ( 0.000000000000000000, 0.000000000000000000, 1.000000000000000000 ) ) ;
#31046 = CARTESIAN_POINT ( 'NONE',  ( 116.1998614775786507, -10.63000616557722466, -14.87417383870573495 ) ) ;
#31047 = EDGE_LOOP ( 'NONE', ( #12893, #16464, #27223, #30285 ) ) ;
#31048 = TOROIDAL_SURFACE ( 'NONE', #3388, 5.500000000000000000, 0.5000000000000000000 ) ;
#31049 = CARTESIAN_POINT ( 'NONE',  ( 111.7184548109119788, -9.261995988541697145, -16.69588392320189030 ) ) ;
#31050 = CARTESIAN_POINT ( 'NONE',  ( 70.19189222814998175, -62.26243369865490251, -38.10776559704283528 ) ) ;
#31051 = CARTESIAN_POINT ( 'NONE',  ( 106.2459265045248173, -7.250697342233347165, -19.15521520033831138 ) ) ;
#31052 = CARTESIAN_POINT ( 'NONE',  ( 108.6767858795247861, -8.402594152722688392, -9.854619843455216355 ) ) ;
#31053 = CARTESIAN_POINT ( 'NONE',  ( 109.5102233795247884, -8.938348069036489818, -17.46756447353520159 ) ) ;
#31054 = ADVANCED_FACE ( 'NONE', ( #15080 ), #825, .T. ) ;
#31055 = CARTESIAN_POINT ( 'NONE',  ( 122.9503348109119827, 0.5811942927096110934, -14.16772938898807510 ) ) ;
#31056 = CARTESIAN_POINT ( 'NONE',  ( 112.0020881442453344, 0.2603800115204892296, -16.42320221600525088 ) ) ;
#31057 = ORIENTED_EDGE ( 'NONE', *, *, #25738, .T. ) ;
#31058 = CARTESIAN_POINT ( 'NONE',  ( 125.7866681442452688, -0.4660016031367893996, -10.09054647747474043 ) ) ;
#31059 = CARTESIAN_POINT ( 'NONE',  ( 111.5243640045248412, -10.62599879583958717, -11.00651665394454604 ) ) ;
#31060 = DIRECTION ( 'NONE',  ( 0.000000000000000000, -0.3818493186865936084, 0.9242245927363024194 ) ) ;
#31061 = CARTESIAN_POINT ( 'NONE',  ( 123.6310548109119765, -5.638512984488999180, -18.83840828888717311 ) ) ;
#31062 = DIRECTION ( 'NONE',  ( 1.000000000000000000, 0.000000000000000000, 0.000000000000000000 ) ) ;
#31063 = DIRECTION ( 'NONE',  ( 0.9609149988134837450, -0.1028163501681639419, 0.2570431154366518145 ) ) ;
#31064 = CARTESIAN_POINT ( 'NONE',  ( 126.2972081442452890, -2.084020599724406786, -8.691656652584148546 ) ) ;
#31065 = DIRECTION ( 'NONE',  ( -0.1352586133457953366, -0.9908103287288504424, 0.000000000000000000 ) ) ;
#31066 = CARTESIAN_POINT ( 'NONE',  ( 113.8857702545248003, 0.1403307496149616695, -11.32035403202665336 ) ) ;
#31067 = ORIENTED_EDGE ( 'NONE', *, *, #31968, .F. ) ;
#31068 = FACE_OUTER_BOUND ( 'NONE', #23979, .T. ) ;
#31069 = CARTESIAN_POINT ( 'NONE',  ( 114.2711548109119803, -0.1624402480850797581, -16.17319339645315424 ) ) ;
#31070 = CARTESIAN_POINT ( 'NONE',  ( 125.7866681442452688, -8.899110576539710493, -16.42337572283490132 ) ) ;
#31071 = AXIS2_PLACEMENT_3D ( 'NONE', #26246, #43127, #8472 ) ;
#31072 = CARTESIAN_POINT ( 'NONE',  ( 106.5931921295248372, -9.868328341294093420, -13.39321520033831447 ) ) ;
#31073 = CARTESIAN_POINT ( 'NONE',  ( 105.1346765045248475, -2.791137627527939813, -8.388885654883777576 ) ) ;
#31074 = CARTESIAN_POINT ( 'NONE',  ( 121.5888948109119809, 0.1319031606808879209, -14.10382304977623669 ) ) ;
#31075 = CARTESIAN_POINT ( 'NONE',  ( 115.4624148109119943, -4.153390946401321671, -8.397313243818183892 ) ) ;
#31076 = CARTESIAN_POINT ( 'NONE',  ( 125.4463081442452932, -5.638512984488999180, -18.83840828888717311 ) ) ;
#31077 = VERTEX_POINT ( 'NONE', #26018 ) ;
#31078 = AXIS2_PLACEMENT_3D ( 'NONE', #25684, #29549, #15419 ) ;
#31079 = CARTESIAN_POINT ( 'NONE',  ( 124.1415948109119540, -3.505236298600246325, -18.68346056562440793 ) ) ;
#31080 = CARTESIAN_POINT ( 'NONE',  ( 118.4122014775786340, 0.5811942927096110934, -14.16772938898807510 ) ) ;
#31081 = FACE_OUTER_BOUND ( 'NONE', #34904, .T. ) ;
#31082 = CARTESIAN_POINT ( 'NONE',  ( 113.1366214775786432, -7.643976991954077427, -18.09477374809248928 ) ) ;
#31083 = EDGE_LOOP ( 'NONE', ( #14648, #31580, #19874, #8363 ) ) ;
#31084 = CARTESIAN_POINT ( 'NONE',  ( 78.29371559379768541, 3.878430683262009016, -4.893215200338310922 ) ) ;
#31085 = AXIS2_PLACEMENT_3D ( 'NONE', #2484, #41043, #37601 ) ;
#31086 = ORIENTED_EDGE ( 'NONE', *, *, #6693, .F. ) ;
#31087 = CARTESIAN_POINT ( 'NONE',  ( 114.2144281442453178, -1.833838273342658809, -17.42832698103878286 ) ) ;
#31088 = CARTESIAN_POINT ( 'NONE',  ( 115.4056881442453459, -2.084020599724406786, -8.691656652584148546 ) ) ;
#31089 =( BOUNDED_SURFACE ( )  B_SPLINE_SURFACE ( 1, 2, ( 
 ( #44241, #17263, #24544, #24758, #38647, #7200, #21564, #21339, #38432, #24328, #3998, #28194, #17697, #38214, #31817, #10640, #35224, #27972, #7418, #28412, #14499, #142, #17473, #20684, #45073, #6774, #17920, #20903, #21113, #34561, #34987, #3773, #31595, #589, #6992, #3344, #42321, #41664, #26896, #364, #40816, #27748, #11083, #24985, #13833, #14275, #4226, #35451, #41878, #34777, #42100, #38879, #10421, #10863, #3560, #7649, #18145, #9572, #23488, #31370, #14056, #32040, #29530, #28861, #807, #11985, #8334, #22683, #25215, #36581, #14725, #39114, #28638, #15171, #15624, #18815, #22233, #22459, #1703, #1260, #39788, #32486, #43445, #4673, #35908, #42773, #5124, #4898, #29304, #40014, #32706, #36129, #5357, #25886, #32927, #39345, #42545, #22013, #12209, #11306, #21790, #25666, #18594, #7882, #1479, #35682, #29077, #4456, #15400, #36353, #19040, #42989, #26107, #8558, #18377, #11756, #39571, #8779, #32265, #43217, #1033, #14950, #11536, #25443, #8112, #33152, #1928, #15854, #29750, #43662, #40244, #9013, #22910, #19273, #12438, #26337, #36803, #28463, #31416, #7037, #14546, #183, #6820, #38473, #409, #44908, #38700, #10688, #35039, #24590, #38927, #21613, #13879, #24369, #24152, #41923, #7249, #14325, #17967, #25035, #7468 ),
 ( #20727, #31866, #20947, #42371, #42148, #10468, #633, #21162, #31640, #35500, #35268, #24808, #11132, #7698, #34607, #17091, #17311, #3820, #21385, #3392, #10908, #30983, #4045, #17744, #41703, #13665, #28239, #27574, #38256, #41486, #28017, #10244, #14100, #38044, #31201, #45123, #17519, #34821, #27790, #3604, #35124, #35354, #38336, #13963, #16946, #21023, #21247, #7328, #20805, #3907, #38552, #34465, #6895, #34684, #24665, #492, #31276, #7113, #30840, #27431, #31499, #6679, #37901, #3244, #17170, #44987, #3472, #10769, #31722, #14405, #44763, #34896, #28315, #31059, #42227, #49, #17387, #10990, #27874, #20587, #3685, #270, #13522, #17825, #10545, #17606, #24445, #38785, #21471, #13746, #24231, #24013, #41788, #14179, #28097, #24892, #7556, #41353, #27654, #42005, #10109, #41569, #10328, #38122, #28547, #39698, #709, #39018, #22144, #4805, #18726, #1384, #14629, #36036, #43117, #39473, #15299, #25567, #35583, #32618, #32394, #29208, #18504, #22587, #11887, #32834, #4130, #1603, #940, #18050, #25789, #8237, #39922, #42451, #8683, #31943, #11217, #25122, #1163, #15523, #8463, #22366, #36262, #18944, #15079, #5029, #4579, #29430, #21916, #8007, #7788, #21697, #43344, #12114, #26017, #4355, #18275, #32171, #14859, #28768, #42674 ) ),
 .UNSPECIFIED., .F., .F., .F. ) 
 B_SPLINE_SURFACE_WITH_KNOTS ( ( 2, 2 ),
 ( 3, 2, 2, 2, 2, 2, 2, 2, 2, 2, 2, 2, 2, 2, 2, 2, 2, 2, 2, 2, 2, 2, 2, 2, 2, 2, 2, 2, 2, 2, 2, 2, 2, 2, 2, 2, 2, 2, 2, 2, 2, 2, 2, 2, 2, 2, 2, 2, 2, 2, 2, 2, 2, 2, 2, 2, 2, 2, 2, 2, 2, 2, 2, 2, 2, 2, 2, 2, 2, 2, 2, 2, 2, 2, 2, 2, 2, 2, 2, 2, 3 ),
 ( 0.000000000000000000, 1.000000000000000000 ),
 ( 0.000000000000000000, 0.01250000000000000069, 0.02500000000000000139, 0.03749999999999999861, 0.05000000000000000278, 0.06250000000000000000, 0.07499999999999999722, 0.08749999999999999445, 0.1000000000000000056, 0.1125000000000000028, 0.1250000000000000000, 0.1375000000000000111, 0.1499999999999999944, 0.1625000000000000056, 0.1749999999999999889, 0.1875000000000000000, 0.2000000000000000111, 0.2124999999999999944, 0.2250000000000000056, 0.2374999999999999889, 0.2500000000000000000, 0.2625000000000000111, 0.2750000000000000222, 0.2874999999999999778, 0.2999999999999999889, 0.3125000000000000000, 0.3250000000000000111, 0.3375000000000000222, 0.3499999999999999778, 0.3624999999999999889, 0.3750000000000000000, 0.3875000000000000111, 0.4000000000000000222, 0.4124999999999999778, 0.4249999999999999889, 0.4375000000000000000, 0.4500000000000000111, 0.4625000000000000222, 0.4749999999999999778, 0.4874999999999999889, 0.5000000000000000000, 0.5124999999999999556, 0.5250000000000000222, 0.5374999999999999778, 0.5500000000000000444, 0.5625000000000000000, 0.5749999999999999556, 0.5875000000000000222, 0.5999999999999999778, 0.6125000000000000444, 0.6250000000000000000, 0.6374999999999999556, 0.6500000000000000222, 0.6624999999999999778, 0.6750000000000000444, 0.6875000000000000000, 0.6999999999999999556, 0.7125000000000000222, 0.7249999999999999778, 0.7375000000000000444, 0.7500000000000000000, 0.7624999999999999556, 0.7750000000000000222, 0.7874999999999999778, 0.8000000000000000444, 0.8125000000000000000, 0.8249999999999999556, 0.8375000000000000222, 0.8499999999999999778, 0.8625000000000000444, 0.8750000000000000000, 0.8874999999999999556, 0.9000000000000000222, 0.9124999999999999778, 0.9250000000000000444, 0.9375000000000000000, 0.9499999999999999556, 0.9625000000000000222, 0.9749999999999999778, 0.9875000000000000444, 1.000000000000000000 ),
 .UNSPECIFIED. ) 
 GEOMETRIC_REPRESENTATION_ITEM ( )  RATIONAL_B_SPLINE_SURFACE ( (
 ( 1.000000000000000000, 0.9238795325112869605, 1.000000000000000000, 0.9238795325112869605, 1.000000000000000000, 0.9238795325112869605, 1.000000000000000000, 0.9238795325112869605, 1.000000000000000000, 0.9238795325112869605, 1.000000000000000000, 0.9238795325112869605, 1.000000000000000000, 0.9238795325112869605, 1.000000000000000000, 0.9238795325112869605, 1.000000000000000000, 0.9238795325112869605, 1.000000000000000000, 0.9238795325112869605, 1.000000000000000000, 0.9238795325112869605, 1.000000000000000000, 0.9238795325112869605, 1.000000000000000000, 0.9238795325112869605, 1.000000000000000000, 0.9238795325112869605, 1.000000000000000000, 0.9238795325112869605, 1.000000000000000000, 0.9238795325112869605, 1.000000000000000000, 0.9238795325112869605, 1.000000000000000000, 0.9238795325112869605, 1.000000000000000000, 0.9238795325112869605, 1.000000000000000000, 0.9238795325112869605, 1.000000000000000000, 0.9238795325112869605, 1.000000000000000000, 0.9238795325112869605, 1.000000000000000000, 0.9238795325112869605, 1.000000000000000000, 0.9238795325112869605, 1.000000000000000000, 0.9238795325112869605, 1.000000000000000000, 0.9238795325112869605, 1.000000000000000000, 0.9238795325112869605, 1.000000000000000000, 0.9238795325112869605, 1.000000000000000000, 0.9238795325112869605, 1.000000000000000000, 0.9238795325112869605, 1.000000000000000000, 0.9238795325112869605, 1.000000000000000000, 0.9238795325112869605, 1.000000000000000000, 0.9238795325112869605, 1.000000000000000000, 0.9238795325112869605, 1.000000000000000000, 0.9238795325112869605, 1.000000000000000000, 0.9238795325112869605, 1.000000000000000000, 0.9238795325112869605, 1.000000000000000000, 0.9238795325112869605, 1.000000000000000000, 0.9238795325112869605, 1.000000000000000000, 0.9238795325112869605, 1.000000000000000000, 0.9238795325112869605, 1.000000000000000000, 0.9238795325112869605, 1.000000000000000000, 0.9238795325112869605, 1.000000000000000000, 0.9238795325112869605, 1.000000000000000000, 0.9238795325112869605, 1.000000000000000000, 0.9238795325112869605, 1.000000000000000000, 0.9238795325112869605, 1.000000000000000000, 0.9238795325112869605, 1.000000000000000000, 0.9238795325112869605, 1.000000000000000000, 0.9238795325112869605, 1.000000000000000000, 0.9238795325112869605, 1.000000000000000000, 0.9238795325112869605, 1.000000000000000000, 0.9238795325112869605, 1.000000000000000000, 0.9238795325112869605, 1.000000000000000000, 0.9238795325112869605, 1.000000000000000000, 0.9238795325112869605, 1.000000000000000000, 0.9238795325112869605, 1.000000000000000000, 0.9238795325112869605, 1.000000000000000000, 0.9238795325112869605, 1.000000000000000000, 0.9238795325112869605, 1.000000000000000000, 0.9238795325112869605, 1.000000000000000000, 0.9238795325112869605, 1.000000000000000000, 0.9238795325112869605, 1.000000000000000000, 0.9238795325112869605, 1.000000000000000000, 0.9238795325112869605, 1.000000000000000000, 0.9238795325112869605, 1.000000000000000000, 0.9238795325112869605, 1.000000000000000000, 0.9238795325112869605, 1.000000000000000000, 0.9238795325112869605, 1.000000000000000000, 0.9238795325112869605, 1.000000000000000000, 0.9238795325112869605, 1.000000000000000000, 0.9238795325112869605, 1.000000000000000000, 0.9238795325112869605, 1.000000000000000000, 0.9238795325112869605, 1.000000000000000000, 0.9238795325112869605, 1.000000000000000000, 0.9238795325112869605, 1.000000000000000000, 0.9238795325112869605, 1.000000000000000000, 0.9238795325112869605, 1.000000000000000000, 0.9238795325112869605, 1.000000000000000000, 0.9238795325112869605, 1.000000000000000000),
 ( 1.000000000000000000, 0.9238795325112869605, 1.000000000000000000, 0.9238795325112869605, 1.000000000000000000, 0.9238795325112869605, 1.000000000000000000, 0.9238795325112869605, 1.000000000000000000, 0.9238795325112869605, 1.000000000000000000, 0.9238795325112869605, 1.000000000000000000, 0.9238795325112869605, 1.000000000000000000, 0.9238795325112869605, 1.000000000000000000, 0.9238795325112869605, 1.000000000000000000, 0.9238795325112869605, 1.000000000000000000, 0.9238795325112869605, 1.000000000000000000, 0.9238795325112869605, 1.000000000000000000, 0.9238795325112869605, 1.000000000000000000, 0.9238795325112869605, 1.000000000000000000, 0.9238795325112869605, 1.000000000000000000, 0.9238795325112869605, 1.000000000000000000, 0.9238795325112869605, 1.000000000000000000, 0.9238795325112869605, 1.000000000000000000, 0.9238795325112869605, 1.000000000000000000, 0.9238795325112869605, 1.000000000000000000, 0.9238795325112869605, 1.000000000000000000, 0.9238795325112869605, 1.000000000000000000, 0.9238795325112869605, 1.000000000000000000, 0.9238795325112869605, 1.000000000000000000, 0.9238795325112869605, 1.000000000000000000, 0.9238795325112869605, 1.000000000000000000, 0.9238795325112869605, 1.000000000000000000, 0.9238795325112869605, 1.000000000000000000, 0.9238795325112869605, 1.000000000000000000, 0.9238795325112869605, 1.000000000000000000, 0.9238795325112869605, 1.000000000000000000, 0.9238795325112869605, 1.000000000000000000, 0.9238795325112869605, 1.000000000000000000, 0.9238795325112869605, 1.000000000000000000, 0.9238795325112869605, 1.000000000000000000, 0.9238795325112869605, 1.000000000000000000, 0.9238795325112869605, 1.000000000000000000, 0.9238795325112869605, 1.000000000000000000, 0.9238795325112869605, 1.000000000000000000, 0.9238795325112869605, 1.000000000000000000, 0.9238795325112869605, 1.000000000000000000, 0.9238795325112869605, 1.000000000000000000, 0.9238795325112869605, 1.000000000000000000, 0.9238795325112869605, 1.000000000000000000, 0.9238795325112869605, 1.000000000000000000, 0.9238795325112869605, 1.000000000000000000, 0.9238795325112869605, 1.000000000000000000, 0.9238795325112869605, 1.000000000000000000, 0.9238795325112869605, 1.000000000000000000, 0.9238795325112869605, 1.000000000000000000, 0.9238795325112869605, 1.000000000000000000, 0.9238795325112869605, 1.000000000000000000, 0.9238795325112869605, 1.000000000000000000, 0.9238795325112869605, 1.000000000000000000, 0.9238795325112869605, 1.000000000000000000, 0.9238795325112869605, 1.000000000000000000, 0.9238795325112869605, 1.000000000000000000, 0.9238795325112869605, 1.000000000000000000, 0.9238795325112869605, 1.000000000000000000, 0.9238795325112869605, 1.000000000000000000, 0.9238795325112869605, 1.000000000000000000, 0.9238795325112869605, 1.000000000000000000, 0.9238795325112869605, 1.000000000000000000, 0.9238795325112869605, 1.000000000000000000, 0.9238795325112869605, 1.000000000000000000, 0.9238795325112869605, 1.000000000000000000, 0.9238795325112869605, 1.000000000000000000, 0.9238795325112869605, 1.000000000000000000, 0.9238795325112869605, 1.000000000000000000, 0.9238795325112869605, 1.000000000000000000, 0.9238795325112869605, 1.000000000000000000, 0.9238795325112869605, 1.000000000000000000, 0.9238795325112869605, 1.000000000000000000, 0.9238795325112869605, 1.000000000000000000, 0.9238795325112869605, 1.000000000000000000, 0.9238795325112869605, 1.000000000000000000, 0.9238795325112869605, 1.000000000000000000, 0.9238795325112869605, 1.000000000000000000, 0.9238795325112869605, 1.000000000000000000, 0.9238795325112869605, 1.000000000000000000) ) ) 
 REPRESENTATION_ITEM ( '' )  SURFACE ( )  );
#31090 = CARTESIAN_POINT ( 'NONE',  ( 128.2184548109119930, -4.863998795839242995, -13.39321520033831447 ) ) ;
#31091 = CARTESIAN_POINT ( 'NONE',  ( 124.1884548109119777, -2.527210466738041728, -8.967976844669124148 ) ) ;
#31092 = VERTEX_POINT ( 'NONE', #28992 ) ;
#31093 = CARTESIAN_POINT ( 'NONE',  ( 59.78685257969296174, -14.81377569729348664, -7.401628058557651713 ) ) ;
#31094 = CARTESIAN_POINT ( 'NONE',  ( 62.62390430415688769, -3.460464904265341701, -7.586702879152205092 ) ) ;
#31095 = CARTESIAN_POINT ( 'NONE',  ( 113.8163171295247764, -10.62599879583958540, -13.39321520033831447 ) ) ;
#31096 = CIRCLE ( 'NONE', #39853, 6.999999999999999112 ) ;
#31097 = CARTESIAN_POINT ( 'NONE',  ( 115.0207045411902413, -0.3595008806742185925, -10.82052240173742064 ) ) ;
#31098 = CARTESIAN_POINT ( 'NONE',  ( 123.6877814775786533, -6.222761293078241884, -8.102969835052219238 ) ) ;
#31099 = CARTESIAN_POINT ( 'NONE',  ( 114.3846081442453197, 0.4262465694468514643, -12.03445270309931736 ) ) ;
#31100 = CARTESIAN_POINT ( 'NONE',  ( 113.7606148109119886, -7.894159318335810305, -9.358103419637835430 ) ) ;
#31101 = ORIENTED_EDGE ( 'NONE', *, *, #8582, .F. ) ;
#31102 = CARTESIAN_POINT ( 'NONE',  ( 71.95541746945981743, -68.51322876793039995, -38.63625753187658063 ) ) ;
#31103 = CARTESIAN_POINT ( 'NONE',  ( 116.3133148109120043, -2.084020599724406786, -8.691656652584148546 ) ) ;
#31104 = CARTESIAN_POINT ( 'NONE',  ( 85.82609049628328535, -26.41178087463453750, -7.893215200339676052 ) ) ;
#31106 = CARTESIAN_POINT ( 'NONE',  ( 125.5597614775786326, -1.561330072975669392, -17.79121239304076951 ) ) ;
#31105 = CARTESIAN_POINT ( 'NONE',  ( 64.43535090723580083, -36.95092036245521427, -5.467054258871676176 ) ) ;
#31107 = CARTESIAN_POINT ( 'NONE',  ( 125.5597614775786326, -7.894159318335828068, -9.358103419637847864 ) ) ;
#31108 = ORIENTED_EDGE ( 'NONE', *, *, #28630, .T. ) ;
#31109 = CARTESIAN_POINT ( 'NONE',  ( 114.3846081442453197, -10.63000616557722466, -14.87417383870573495 ) ) ;
#31110 = DIRECTION ( 'NONE',  ( -0.1352586133457950590, -0.9908103287288504424, 0.000000000000000000 ) ) ;
#31111 = CARTESIAN_POINT ( 'NONE',  ( 115.2053796295247849, -4.863998795839590272, -19.15521520033831493 ) ) ;
#31112 = CARTESIAN_POINT ( 'NONE',  ( 126.1837548109119496, 0.4262465694468514643, -12.03445270309931736 ) ) ;
#31113 = CARTESIAN_POINT ( 'NONE',  ( 126.5241148109119393, -9.565557343593413364, -10.61323700422348004 ) ) ;
#31114 = AXIS2_PLACEMENT_3D ( 'NONE', #9741, #30030, #24100 ) ;
#31115 = CARTESIAN_POINT ( 'NONE',  ( 124.9357681442453014, -7.643976991954077427, -18.09477374809248928 ) ) ;
#31116 = CARTESIAN_POINT ( 'NONE',  ( 61.63318325272354770, -19.46990085680238636, -10.39321520033831625 ) ) ;
#31117 = CARTESIAN_POINT ( 'NONE',  ( 109.7185827545247889, -6.936859964151250502, -8.388885654883777576 ) ) ;
#31118 = CARTESIAN_POINT ( 'NONE',  ( 111.6632702545248605, -10.62599879583958540, -15.77991374673208469 ) ) ;
#31119 = CARTESIAN_POINT ( 'NONE',  ( 73.07463722459043254, -55.71104259080762233, -34.59272409957256400 ) ) ;
#31120 = CARTESIAN_POINT ( 'NONE',  ( 116.3700414775786527, -4.153390946401321671, -8.397313243818183892 ) ) ;
#31121 = DIRECTION ( 'NONE',  ( 0.9609149988134837450, -0.1028163501681639419, 0.2570431154366518145 ) ) ;
#31122 = DIRECTION ( 'NONE',  ( 0.3445294493088594256, 0.9387755102040817867, 0.000000000000000000 ) ) ;
#31123 = CARTESIAN_POINT ( 'NONE',  ( 109.3018640045248304, -10.62599879583958717, -11.00651665394454604 ) ) ;
#31124 = CARTESIAN_POINT ( 'NONE',  ( 125.9001214775786224, -4.089484607189486809, -7.948022111789456723 ) ) ;
#31125 = CARTESIAN_POINT ( 'NONE',  ( 112.2857214775786474, -5.574606645277164318, -18.38911715685844683 ) ) ;
#31126 = CARTESIAN_POINT ( 'NONE',  ( 111.6402504229301940, 0.1075849324168598464, -14.64321520033829671 ) ) ;
#31127 = CARTESIAN_POINT ( 'NONE',  ( 121.4754414775786131, -8.166667518702819706, -8.995218007635861213 ) ) ;
#31128 = EDGE_CURVE ( 'NONE', #44558, #7488, #19776, .T. ) ;
#31129 = CARTESIAN_POINT ( 'NONE',  ( 117.0507614775786465, -10.30919188438810075, -12.61870101168855918 ) ) ;
#31130 = ORIENTED_EDGE ( 'NONE', *, *, #38212, .F. ) ;
#31131 = CARTESIAN_POINT ( 'NONE',  ( 113.5904348109119866, -2.084020599724406786, -8.691656652584148546 ) ) ;
#31132 = CARTESIAN_POINT ( 'NONE',  ( 122.3830681442452857, -8.166667518702819706, -8.995218007635861213 ) ) ;
#31133 = CARTESIAN_POINT ( 'NONE',  ( 114.7816948109119863, 0.5811942927096154232, -14.16772938898807155 ) ) ;
#31134 = CARTESIAN_POINT ( 'NONE',  ( 117.2209414775786485, -2.084020599724406786, -8.691656652584148546 ) ) ;
#31135 = ORIENTED_EDGE ( 'NONE', *, *, #1608, .F. ) ;
#31136 = CARTESIAN_POINT ( 'NONE',  ( 121.8725281442453223, -6.222761293078241884, -8.102969835052219238 ) ) ;
#31137 = CARTESIAN_POINT ( 'NONE',  ( 115.8027748109119841, -0.4660016031367893996, -10.09054647747474043 ) ) ;
#31138 = CARTESIAN_POINT ( 'NONE',  ( 124.8223148109119762, -10.15424416112533912, -14.75197769757731336 ) ) ;
#31139 = CARTESIAN_POINT ( 'NONE',  ( 116.8567633678298705, -0.4761927928726716885, -16.29842386168302681 ) ) ;
#31140 = CARTESIAN_POINT ( 'NONE',  ( 112.5661608795247872, -8.938348069036489818, -9.318865927141430916 ) ) ;
#31141 = EDGE_LOOP ( 'NONE', ( #30920, #28254, #7121, #9678, #18520, #22681 ) ) ;
#31142 = AXIS2_PLACEMENT_3D ( 'NONE', #15402, #25888, #8336 ) ;
#31143 = CARTESIAN_POINT ( 'NONE',  ( 70.19189222814998175, -51.68868231262963775, -33.87830190084585524 ) ) ;
#31144 = CARTESIAN_POINT ( 'NONE',  ( 125.7299414775786346, 0.9020085738987339008, -11.91225656197089222 ) ) ;
#31145 = ADVANCED_FACE ( 'NONE', ( #2059 ), #20508, .F. ) ;
#31146 = CARTESIAN_POINT ( 'NONE',  ( 70.19189222814998175, -63.19092768811421479, -43.86431829041166708 ) ) ;
#31147 = CARTESIAN_POINT ( 'NONE',  ( 116.5402214775786405, 0.2603800115204892296, -16.42320221600525088 ) ) ;
#31148 = CARTESIAN_POINT ( 'NONE',  ( 71.31713442278437753, 2.423123680056944007, -10.89321520033831447 ) ) ;
#31149 = CARTESIAN_POINT ( 'NONE',  ( 113.5904348109119866, -2.084020599724406786, -8.691656652584148546 ) ) ;
#31150 = EDGE_CURVE ( 'NONE', #43799, #2987, #15982, .T. ) ;
#31151 = CARTESIAN_POINT ( 'NONE',  ( 61.13536639111517701, -12.48752525818348502, -17.20977388067641556 ) ) ;
#31152 = CARTESIAN_POINT ( 'NONE',  ( 70.19189222814998175, -59.47700027789979060, -36.99360193826534271 ) ) ;
#31153 = DIRECTION ( 'NONE',  ( 0.8636456077245088236, -0.5040994586965589219, 0.000000000000000000 ) ) ;
#31154 = CARTESIAN_POINT ( 'NONE',  ( 119.1496481442453046, -3.383040157471821630, -19.15922257007629170 ) ) ;
#31155 = CARTESIAN_POINT ( 'NONE',  ( 137.0897189579595192, -6.643744190842751252, -18.48770628774961367 ) ) ;
#31156 = ADVANCED_FACE ( 'NONE', ( #36489 ), #29658, .T. ) ;
#31157 = CARTESIAN_POINT ( 'NONE',  ( 115.8111041094426810, 0.3591747506842615789, -12.14321520033831625 ) ) ;
#31159 = CARTESIAN_POINT ( 'NONE',  ( 118.7525614775786380, -8.166667518702801942, -8.995218007635848778 ) ) ;
#31158 = CIRCLE ( 'NONE', #17345, 2.999999999999999556 ) ;
#31160 = CARTESIAN_POINT ( 'NONE',  ( 121.8158014775786171, -4.153390946401325223, -8.397313243818185668 ) ) ;
#31161 = EDGE_LOOP ( 'NONE', ( #7387, #26441, #25565, #8300 ) ) ;
#31162 = CARTESIAN_POINT ( 'NONE',  ( 125.9568481442452850, -6.344957434206665248, -7.627207830600338134 ) ) ;
#31163 = CARTESIAN_POINT ( 'NONE',  ( 119.4332814775786318, -0.4660016031367893996, -10.09054647747474043 ) ) ;
#31164 = DIRECTION ( 'NONE',  ( 0.000000000000000000, -0.3818493186865936084, 0.9242245927363024194 ) ) ;
#31165 = CARTESIAN_POINT ( 'NONE',  ( 114.1577014775786552, -3.505236298600246325, -18.68346056562440793 ) ) ;
#31166 = EDGE_CURVE ( 'NONE', #44941, #35019, #32619, .T. ) ;
#31167 = CARTESIAN_POINT ( 'NONE',  ( 113.5904348109119866, -2.084020599724406786, -8.691656652584148546 ) ) ;
#31168 = CARTESIAN_POINT ( 'NONE',  ( 112.3578015045248861, -2.477300249445798297, -7.631215200338321125 ) ) ;
#31169 = CARTESIAN_POINT ( 'NONE',  ( 106.4542858795248179, -8.402594152722688392, -9.854619843455216355 ) ) ;
#31170 = CARTESIAN_POINT ( 'NONE',  ( 113.8857702545248003, -10.62599879583958717, -15.77991374673208469 ) ) ;
#31171 = CARTESIAN_POINT ( 'NONE',  ( 120.9081748109119872, -4.153390946401325223, -8.397313243818185668 ) ) ;
#31172 = CARTESIAN_POINT ( 'NONE',  ( 120.3409081442453044, -8.899110576539710493, -16.42337572283490132 ) ) ;
#31173 = CARTESIAN_POINT ( 'NONE',  ( 109.2294421295247844, -8.865838614420134434, -9.247624522711900497 ) ) ;
#31174 = CARTESIAN_POINT ( 'NONE',  ( 122.4521266859119635, -0.06289925094097943703, -9.412459353600674206 ) ) ;
#31175 = CARTESIAN_POINT ( 'NONE',  ( 110.8992858795247827, -8.402594152722688392, -9.854619843455216355 ) ) ;
#31176 = ADVANCED_FACE ( 'NONE', ( #19173 ), #11888, .F. ) ;
#31177 = DIRECTION ( 'NONE',  ( -0.000000000000000000, -0.9284778069183721172, -0.3713878862591650232 ) ) ;
#31178 = CARTESIAN_POINT ( 'NONE',  ( 112.7962614775786676, -3.383040157471821630, -19.15922257007629170 ) ) ;
#31179 = CARTESIAN_POINT ( 'NONE',  ( 114.6115148109119986, -3.383040157471821630, -19.15922257007629170 ) ) ;
#31180 = CARTESIAN_POINT ( 'NONE',  ( 123.0772048109119652, -2.527210466738041728, -8.967976844669124148 ) ) ;
#31181 = EDGE_CURVE ( 'NONE', #39160, #21122, #29209, .T. ) ;
#31182 = EDGE_CURVE ( 'NONE', #44494, #44451, #23959, .T. ) ;
#31183 = ORIENTED_EDGE ( 'NONE', *, *, #37847, .T. ) ;
#31184 = CARTESIAN_POINT ( 'NONE',  ( 113.2987212410415765, 0.7607806665037644134, -12.14321520033829493 ) ) ;
#31185 = ORIENTED_EDGE ( 'NONE', *, *, #5500, .T. ) ;
#31186 = CARTESIAN_POINT ( 'NONE',  ( 123.5176014775786228, -9.261995988541697145, -16.69588392320189030 ) ) ;
#31187 = CARTESIAN_POINT ( 'NONE',  ( 113.4202548109119846, -10.30919188438810075, -12.61870101168855918 ) ) ;
#31188 = CARTESIAN_POINT ( 'NONE',  ( 117.7314814775786260, -5.574606645277164318, -18.38911715685844683 ) ) ;
#31189 = B_SPLINE_CURVE_WITH_KNOTS ( 'NONE', 3,
 ( #41160, #22907, #9010, #6492, #44802, #6262, #5794, #2142, #13561, #27016, #2375, #5568, #26561, #3064, #16305, #36800, #19490, #12663, #19946, #20182, #34067, #12892, #44127, #26790, #9921, #40933 ),
 .UNSPECIFIED., .F., .F.,
 ( 4, 1, 1, 2, 2, 1, 1, 1, 2, 2, 2, 1, 1, 1, 2, 2, 4 ),
 ( 0.000000000000000000, 0.06249999999981883936, 0.09374999999972753739, 0.1093749999996763422, 0.1249999999996251332, 0.1874999999994354793, 0.2187499999993496314, 0.2343749999993062216, 0.2421874999992941757, 0.2499999999992821298, 0.3749999999993258171, 0.4374999999993480215, 0.4687499999993595123, 0.4843749999993777200, 0.4921874999993741118, 0.4999999999993705035, 1.000000000000000000 ),
 .UNSPECIFIED. ) ;
#31190 = CARTESIAN_POINT ( 'NONE',  ( 120.2524138005195482, -8.246127466884534130, -17.07828452773560812 ) ) ;
#31191 = CARTESIAN_POINT ( 'NONE',  ( 121.9859814775786333, 0.2603800115204892296, -16.42320221600525088 ) ) ;
#31192 = CARTESIAN_POINT ( 'NONE',  ( 117.6747548109119919, -1.834011780172310813, -8.268836392978581529 ) ) ;
#31193 = CARTESIAN_POINT ( 'NONE',  ( 107.2182702545248105, 0.1403307496149616695, -11.32035403202665336 ) ) ;
#31194 = CARTESIAN_POINT ( 'NONE',  ( 114.1009748109119784, -5.574606645277164318, -18.38911715685844683 ) ) ;
#31195 = CARTESIAN_POINT ( 'NONE',  ( 124.9924948109119924, -5.574606645277184747, -18.38911715685844328 ) ) ;
#31196 = EDGE_LOOP ( 'NONE', ( #26091, #25673, #41239, #678, #4212, #22467, #8144, #34198, #16334, #6273, #15116, #20075, #16177, #32453, #10508, #33322, #11733 ) ) ;
#31197 = CARTESIAN_POINT ( 'NONE',  ( 117.5045748109119756, 0.5811942927096110934, -14.16772938898807510 ) ) ;
#31198 = DIRECTION ( 'NONE',  ( 0.000000000000000000, 0.3818493186865927203, -0.9242245927363029745 ) ) ;
#31199 = CARTESIAN_POINT ( 'NONE',  ( 114.0442481442453300, -1.834011780172310813, -8.268836392978581529 ) ) ;
#31200 = VERTEX_POINT ( 'NONE', #13245 ) ;
#31201 = CARTESIAN_POINT ( 'NONE',  ( 114.2330358795247776, -0.7896495226426338832, -17.46756447353520159 ) ) ;
#31202 = CARTESIAN_POINT ( 'NONE',  ( -13.56828338283517787, -4.779084856631165223, -8.846726502787863211 ) ) ;
#31203 = CARTESIAN_POINT ( 'NONE',  ( 83.72016463086879412, -25.23119213852205789, -15.24166438581092109 ) ) ;
#31204 = CARTESIAN_POINT ( 'NONE',  ( 90.45092582798827152, -26.75858941326842810, -11.54476601486570964 ) ) ;
#31205 = CARTESIAN_POINT ( 'NONE',  ( 78.69189222814998175, -59.80879295971297438, 0.4535904759388441621 ) ) ;
#31206 = CARTESIAN_POINT ( 'NONE',  ( 115.9162281442453093, -5.574606645277164318, -18.38911715685844683 ) ) ;
#31207 = CARTESIAN_POINT ( 'NONE',  ( 115.9294421295247872, 1.035107641088057973, -14.64321520033831447 ) ) ;
#31208 = CARTESIAN_POINT ( 'NONE',  ( 116.5402214775786405, -9.565557343593413364, -10.61323700422348004 ) ) ;
#31209 = ADVANCED_FACE ( 'NONE', ( #37626 ), #23735, .F. ) ;
#31210 = DIRECTION ( 'NONE',  ( 0.000000000000000000, 0.9284778069183720062, 0.3713878862591650232 ) ) ;
#31211 = CARTESIAN_POINT ( 'NONE',  ( 117.7314814775786260, -5.574606645277164318, -18.38911715685844683 ) ) ;
#31212 = CARTESIAN_POINT ( 'NONE',  ( 122.9382985609119743, -10.36940331770106916, -15.09355782777062061 ) ) ;
#31213 = CARTESIAN_POINT ( 'NONE',  ( 114.2144281442453178, -8.166667518702817929, -8.995218007635859436 ) ) ;
#31214 = CARTESIAN_POINT ( 'NONE',  ( 115.5758681442453053, -7.894159318335828068, -9.358103419637847864 ) ) ;
#31215 = ORIENTED_EDGE ( 'NONE', *, *, #37812, .F. ) ;
#31216 = CARTESIAN_POINT ( 'NONE',  ( 118.4689281442453392, 0.9020085738987339008, -11.91225656197089222 ) ) ;
#31217 = CARTESIAN_POINT ( 'NONE',  ( 105.8292077545248446, -7.250697342233347165, -7.631215200338321125 ) ) ;
#31218 = CARTESIAN_POINT ( 'NONE',  ( 106.5237390045248418, -9.868328341294098749, -11.32035403202665869 ) ) ;
#31219 = CARTESIAN_POINT ( 'NONE',  ( 111.2184548109119788, -1.295815253274133161, -16.89579513612386563 ) ) ;
#31220 = CARTESIAN_POINT ( 'NONE',  ( 112.1721994132789320, -8.900630651041904429, -16.42135045828372597 ) ) ;
#31221 = CARTESIAN_POINT ( 'NONE',  ( 123.1205148109119563, -1.834011780172310813, -8.268836392978581529 ) ) ;
#31222 = VERTEX_POINT ( 'NONE', #43802 ) ;
#31223 = DIRECTION ( 'NONE',  ( 1.000000000000000000, 0.000000000000000000, -0.000000000000000000 ) ) ;
#31224 = CARTESIAN_POINT ( 'NONE',  ( 118.9227414775786542, 0.4262465694468514643, -12.03445270309931736 ) ) ;
#31225 = CARTESIAN_POINT ( 'NONE',  ( 115.7460481442453215, 0.9020085738987339008, -11.91225656197089222 ) ) ;
#31226 = CARTESIAN_POINT ( 'NONE',  ( 9.052690036452151645, -4.182915634381243919, -17.89321520033831447 ) ) ;
#31227 = ADVANCED_FACE ( 'NONE', ( #26916 ), #10056, .T. ) ;
#31228 = CARTESIAN_POINT ( 'NONE',  ( 123.1205148109119563, -1.834011780172310813, -8.268836392978581529 ) ) ;
#31229 = CARTESIAN_POINT ( 'NONE',  ( 112.3578015045248861, -6.936859964151250502, -18.39754474579286025 ) ) ;
#31230 = CARTESIAN_POINT ( 'NONE',  ( 124.6321897909087966, -1.016270020561755860, -17.26805140881366896 ) ) ;
#31231 = EDGE_LOOP ( 'NONE', ( #31848, #32517, #9458, #7209 ) ) ;
#31232 = CARTESIAN_POINT ( 'NONE',  ( 112.3424481442453384, -6.344957434206662583, -7.627207830600332805 ) ) ;
#31233 = CARTESIAN_POINT ( 'NONE',  ( 112.5693548109119888, -10.63000616557722466, -14.87417383870573495 ) ) ;
#31234 = CARTESIAN_POINT ( 'NONE',  ( 124.5954081442453116, -3.383040157471821630, -19.15922257007629170 ) ) ;
#31235 = CARTESIAN_POINT ( 'NONE',  ( 116.5969481442453031, -9.859900752359374465, -12.68260735090039404 ) ) ;
#31236 = DIRECTION ( 'NONE',  ( -0.000000000000000000, -0.9284778069183721172, -0.3713878862591650232 ) ) ;
#31237 = CARTESIAN_POINT ( 'NONE',  ( 119.9438214775786378, -7.893985811506177619, -18.51759400769804742 ) ) ;
#31238 = DIRECTION ( 'NONE',  ( 0.000000000000000000, 0.000000000000000000, -1.000000000000000000 ) ) ;
#31239 = EDGE_CURVE ( 'NONE', #408, #31466, #2510, .T. ) ;
#31240 = CARTESIAN_POINT ( 'NONE',  ( 123.1772414775786189, -5.574606645277164318, -18.38911715685844683 ) ) ;
#31241 = ORIENTED_EDGE ( 'NONE', *, *, #30914, .T. ) ;
#31242 = DIRECTION ( 'NONE',  ( -0.000000000000000000, -0.9284778069183718952, -0.3713878862591649677 ) ) ;
#31243 = CARTESIAN_POINT ( 'NONE',  ( 116.3700414775786527, -5.638512984488999180, -18.83840828888717311 ) ) ;
#31244 = CARTESIAN_POINT ( 'NONE',  ( 136.0617147589325668, -8.510257085082880479, -18.03587336798454288 ) ) ;
#31245 = VERTEX_POINT ( 'NONE', #37842 ) ;
#31246 = CARTESIAN_POINT ( 'NONE',  ( 120.5074391859119913, -8.844754642576884152, -8.592115655440050404 ) ) ;
#31247 = CARTESIAN_POINT ( 'NONE',  ( 135.9373687278093996, -1.210166070096996505, -8.718225154784372322 ) ) ;
#31248 = CARTESIAN_POINT ( 'NONE',  ( 121.7590748109119687, -7.893985811506177619, -18.51759400769804742 ) ) ;
#31249 = CARTESIAN_POINT ( 'NONE',  ( 106.4542858795248179, -0.7896495226426338832, -17.46756447353520159 ) ) ;
#31250 = CARTESIAN_POINT ( 'NONE',  ( 118.8660148109119774, 0.1319031606808879209, -14.10382304977623669 ) ) ;
#31251 = ORIENTED_EDGE ( 'NONE', *, *, #38931, .F. ) ;
#31252 = ORIENTED_EDGE ( 'NONE', *, *, #16397, .T. ) ;
#31253 = CARTESIAN_POINT ( 'NONE',  ( 114.1009748109119784, -4.089484607189486809, -7.948022111789456723 ) ) ;
#31254 = CONICAL_SURFACE ( 'NONE', #31962, 3.499999999999999556, 1.325817663668031887 ) ;
#31255 = CARTESIAN_POINT ( 'NONE',  ( 124.9357681442453014, -7.643976991954077427, -18.09477374809248928 ) ) ;
#31256 = TOROIDAL_SURFACE ( 'NONE', #40007, 18.00000000000000000, 2.000000000000000000 ) ;
#31257 = DIRECTION ( 'NONE',  ( 1.000000000000000000, 0.000000000000000000, 0.000000000000000000 ) ) ;
#31258 = CARTESIAN_POINT ( 'NONE',  ( 120.9081748109119872, -5.638512984488999180, -18.83840828888717311 ) ) ;
#31259 = FACE_OUTER_BOUND ( 'NONE', #29179, .T. ) ;
#31260 = DIRECTION ( 'NONE',  ( 0.9495615000563050190, -0.3135808629537517600, 0.000000000000000000 ) ) ;
#31261 = CARTESIAN_POINT ( 'NONE',  ( 122.7801548109119665, -3.383040157471821630, -19.15922257007629170 ) ) ;
#31263 = CARTESIAN_POINT ( 'NONE',  ( 121.5321681442453183, -0.1624402480850797581, -16.17319339645315424 ) ) ;
#31262 = CARTESIAN_POINT ( 'NONE',  ( 120.1140014775786398, -1.561330072975668504, -17.79121239304076951 ) ) ;
#31264 = CARTESIAN_POINT ( 'NONE',  ( 93.24708369096698846, -25.99489077589524300, -13.39321520033831447 ) ) ;
#31265 = CARTESIAN_POINT ( 'NONE',  ( 116.8238548109119819, -4.089484607189486809, -7.948022111789456723 ) ) ;
#31266 = ORIENTED_EDGE ( 'NONE', *, *, #40378, .T. ) ;
#31267 = EDGE_CURVE ( 'NONE', #20890, #28792, #30646, .T. ) ;
#31268 = CARTESIAN_POINT ( 'NONE',  ( 116.0829010812576882, -0.01829820670803256055, -12.14321520033834290 ) ) ;
#31269 = CARTESIAN_POINT ( 'NONE',  ( 106.6626452545248611, 0.8980012041604421569, -11.00651665394454071 ) ) ;
#31270 = CARTESIAN_POINT ( 'NONE',  ( 109.3018640045248304, 0.1403307496149616695, -15.46607636864997204 ) ) ;
#31271 = CARTESIAN_POINT ( 'NONE',  ( 108.3295202545248657, -10.62599879583958717, -15.77991374673208469 ) ) ;
#31272 = CARTESIAN_POINT ( 'NONE',  ( 124.1983214775786166, -8.166667518702819706, -8.995218007635861213 ) ) ;
#31273 = CARTESIAN_POINT ( 'NONE',  ( 125.5030348109119558, -6.222761293078241884, -8.102969835052219238 ) ) ;
#31274 = ORIENTED_EDGE ( 'NONE', *, *, #2285, .F. ) ;
#31275 = CARTESIAN_POINT ( 'NONE',  ( 123.1205148109119563, -1.834011780172310813, -8.268836392978581529 ) ) ;
#31276 = CARTESIAN_POINT ( 'NONE',  ( 112.7050671295247923, -10.62599879583958540, -13.39321520033831447 ) ) ;
#31277 = CARTESIAN_POINT ( 'NONE',  ( 122.2696148109119889, -5.574606645277198957, -18.38911715685844328 ) ) ;
#31278 = CARTESIAN_POINT ( 'NONE',  ( 122.6667014775786413, -7.893985811506177619, -18.51759400769804742 ) ) ;
#31279 = CARTESIAN_POINT ( 'NONE',  ( 124.1983214775786166, -8.166667518702819706, -8.995218007635861213 ) ) ;
#31280 = CARTESIAN_POINT ( 'NONE',  ( 119.1878298109119783, -7.200787124940443817, -17.81845355600750835 ) ) ;
#31281 = CARTESIAN_POINT ( 'NONE',  ( 111.8319081442453182, -5.638512984488999180, -18.83840828888717311 ) ) ;
#31282 = CARTESIAN_POINT ( 'NONE',  ( 116.3860827545247787, -2.477300249445798297, -19.15521520033831138 ) ) ;
#31283 = CARTESIAN_POINT ( 'NONE',  ( 116.0388171295248014, 0.1403307496149613920, -13.39321520033831447 ) ) ;
#31284 = VERTEX_POINT ( 'NONE', #26693 ) ;
#31285 = DIRECTION ( 'NONE',  ( 0.000000000000000000, -0.9242245927363029745, -0.3818493186865927758 ) ) ;
#31286 = CARTESIAN_POINT ( 'NONE',  ( 116.7671281442453335, -7.643976991954077427, -18.09477374809248928 ) ) ;
#31287 = CARTESIAN_POINT ( 'NONE',  ( 126.4673881442452910, -7.894159318335828068, -9.358103419637847864 ) ) ;
#31288 = AXIS2_PLACEMENT_3D ( 'NONE', #39005, #35341, #696 ) ;
#31289 = CARTESIAN_POINT ( 'NONE',  ( 114.7192077545248594, -7.250697342233347165, -7.631215200338321125 ) ) ;
#31290 = CARTESIAN_POINT ( 'NONE',  ( 107.7738952545248310, -9.868328341294098749, -15.46607636864997204 ) ) ;
#31291 = CARTESIAN_POINT ( 'NONE',  ( 120.4543614775786295, -5.574606645277164318, -18.38911715685844683 ) ) ;
#31292 = CARTESIAN_POINT ( 'NONE',  ( 116.4267681442453153, -6.222761293078241884, -8.102969835052219238 ) ) ;
#31293 = CARTESIAN_POINT ( 'NONE',  ( 111.9453614775786434, -7.894159318335828068, -9.358103419637847864 ) ) ;
#31294 = EDGE_LOOP ( 'NONE', ( #26494, #35764, #41922, #16165 ) ) ;
#31295 = CARTESIAN_POINT ( 'NONE',  ( 124.7088614775786226, -9.565557343593413364, -10.61323700422348004 ) ) ;
#31296 = AXIS2_PLACEMENT_3D ( 'NONE', #15958, #40351, #19595 ) ;
#31297 = CYLINDRICAL_SURFACE ( 'NONE', #32412, 1.999999999999998890 ) ;
#31298 = CARTESIAN_POINT ( 'NONE',  ( 112.6260814775786514, -0.8288870151387760510, -10.36305467784173118 ) ) ;
#31299 = ORIENTED_EDGE ( 'NONE', *, *, #1047, .F. ) ;
#31300 = VECTOR ( 'NONE', #37073, 1000.000000000000227 ) ;
#31301 = DIRECTION ( 'NONE',  ( 0.000000000000000000, 0.000000000000000000, 1.000000000000000000 ) ) ;
#31302 = CARTESIAN_POINT ( 'NONE',  ( 110.4825671295247815, 0.1403307496149613920, -13.39321520033831447 ) ) ;
#31303 = ORIENTED_EDGE ( 'NONE', *, *, #24554, .T. ) ;
#31304 = CARTESIAN_POINT ( 'NONE',  ( 120.2841814775786276, -10.15424416112533912, -14.75197769757731336 ) ) ;
#31305 = CARTESIAN_POINT ( 'NONE',  ( 112.0588148109119828, -9.859900752359374465, -12.68260735090039404 ) ) ;
#31306 = CARTESIAN_POINT ( 'NONE',  ( 67.84197459855160162, -57.36860727972680252, -36.87942510454734446 ) ) ;
#31307 = CARTESIAN_POINT ( 'NONE',  ( 123.4244704359119709, -10.25716656981731489, -12.88942061488890545 ) ) ;
#31308 = ORIENTED_EDGE ( 'NONE', *, *, #25940, .T. ) ;
#31309 = DIRECTION ( 'NONE',  ( -0.9908103287288505534, 0.1352586133457950868, 0.000000000000000000 ) ) ;
#31310 = CARTESIAN_POINT ( 'NONE',  ( 125.1375072647485638, -0.5766298686391078121, -7.327922817638773623 ) ) ;
#31311 = CARTESIAN_POINT ( 'NONE',  ( 113.4690515045247992, -2.477300249445798297, -7.631215200338321125 ) ) ;
#31312 = AXIS2_PLACEMENT_3D ( 'NONE', #29601, #43063, #18215 ) ;
#31313 = LINE ( 'NONE', #23600, #5209 ) ;
#31314 = CARTESIAN_POINT ( 'NONE',  ( 123.0637881442452937, -8.899110576539710493, -16.42337572283490132 ) ) ;
#31315 = CARTESIAN_POINT ( 'NONE',  ( 118.9227414775786542, 0.4262465694468514643, -12.03445270309931736 ) ) ;
#31316 = CARTESIAN_POINT ( 'NONE',  ( 113.9307948109119764, -10.15424416112533912, -14.75197769757731336 ) ) ;
#31317 = VERTEX_POINT ( 'NONE', #27147 ) ;
#31318 = CARTESIAN_POINT ( 'NONE',  ( 66.69189222814998175, -41.76310523276723785, -24.89321520033831447 ) ) ;
#31319 = CARTESIAN_POINT ( 'NONE',  ( 114.5547881442453217, -4.153390946401321671, -8.397313243818183892 ) ) ;
#31320 = CARTESIAN_POINT ( 'NONE',  ( 125.3895814775786448, -2.084020599724406786, -8.691656652584148546 ) ) ;
#31321 = AXIS2_PLACEMENT_3D ( 'NONE', #42125, #31843, #7904 ) ;
#31322 = CARTESIAN_POINT ( 'NONE',  ( 85.06864399163163171, -29.49003633093008858, -10.37873928275900504 ) ) ;
#31323 = LINE ( 'NONE', #34944, #11605 ) ;
#31324 = CARTESIAN_POINT ( 'NONE',  ( 115.3489614775786407, -9.261995988541697145, -16.69588392320189030 ) ) ;
#31325 = EDGE_LOOP ( 'NONE', ( #16910, #6136, #19171, #14357 ) ) ;
#31326 = CONICAL_SURFACE ( 'NONE', #28476, 2.999999999999999556, 0.9599310885968830309 ) ;
#31327 = CARTESIAN_POINT ( 'NONE',  ( 112.2289948109119848, -1.834011780172310813, -8.268836392978581529 ) ) ;
#31328 = CARTESIAN_POINT ( 'NONE',  ( 113.7798197424434363, -0.9924539043446216624, -17.29976612834909133 ) ) ;
#31329 = CARTESIAN_POINT ( 'NONE',  ( 112.4967077545247633, -7.250697342233347165, -7.631215200338321125 ) ) ;
#31330 = CARTESIAN_POINT ( 'NONE',  ( 111.9453614775786434, -1.561330072975668060, -17.79121239304076596 ) ) ;
#31331 = CARTESIAN_POINT ( 'NONE',  ( 114.0442481442453300, -1.834011780172310813, -8.268836392978581529 ) ) ;
#31332 = CARTESIAN_POINT ( 'NONE',  ( 123.3474214775786209, -0.1624402480850797581, -16.17319339645315424 ) ) ;
#31333 = DIRECTION ( 'NONE',  ( 0.9908103287288504424, -0.1352586133457950868, 0.000000000000000000 ) ) ;
#31334 = CARTESIAN_POINT ( 'NONE',  ( 111.1076452545248259, -9.868328341294098749, -15.46607636864997204 ) ) ;
#31335 = CARTESIAN_POINT ( 'NONE',  ( 35.90261398037149121, 14.17005867477686820, -18.19321520033831519 ) ) ;
#31336 = CARTESIAN_POINT ( 'NONE',  ( 109.2292941585266703, -5.295636273138023320, -18.58536345472597517 ) ) ;
#31337 = CARTESIAN_POINT ( 'NONE',  ( 117.9016614775786280, -0.1624402480850797581, -16.17319339645315424 ) ) ;
#31338 = EDGE_CURVE ( 'NONE', #42698, #29255, #25984, .T. ) ;
#31339 = CARTESIAN_POINT ( 'NONE',  ( 106.1764733795248219, -8.938348069036489818, -17.46756447353520159 ) ) ;
#31340 = CARTESIAN_POINT ( 'NONE',  ( 115.6220983795247861, -8.402594152722688392, -16.93181055722141792 ) ) ;
#31341 = CARTESIAN_POINT ( 'NONE',  ( 108.3989733795248753, -8.938348069036489818, -17.46756447353520159 ) ) ;
#31342 = CARTESIAN_POINT ( 'NONE',  ( 95.62170725701132312, -26.92997340575169574, -13.22232672137451104 ) ) ;
#31343 = CARTESIAN_POINT ( 'NONE',  ( 111.5482748109120053, -0.1624402480850797581, -16.17319339645315424 ) ) ;
#31344 = CARTESIAN_POINT ( 'NONE',  ( 120.4994581469517101, -3.929494816604745200, -18.62311481910883870 ) ) ;
#31345 = CARTESIAN_POINT ( 'NONE',  ( 121.0216281442452981, -1.561330072975668948, -17.79121239304076951 ) ) ;
#31346 = CARTESIAN_POINT ( 'NONE',  ( 117.9016614775786280, -9.988377603198976828, -10.36322818467138340 ) ) ;
#31347 = VERTEX_POINT ( 'NONE', #12567 ) ;
#31348 = CARTESIAN_POINT ( 'NONE',  ( 113.5337081442453240, -0.8288870151387760510, -10.36305467784173118 ) ) ;
#31349 = CARTESIAN_POINT ( 'NONE',  ( 122.3263414775786373, -6.344957434206665248, -7.627207830600338134 ) ) ;
#31350 = CIRCLE ( 'NONE', #39366, 2.000000000000000444 ) ;
#31351 = CARTESIAN_POINT ( 'NONE',  ( 117.1074881442453233, -10.63000616557722466, -14.87417383870573495 ) ) ;
#31352 = CARTESIAN_POINT ( 'NONE',  ( 116.4267681442453153, -6.222761293078241884, -8.102969835052219238 ) ) ;
#31353 = VERTEX_POINT ( 'NONE', #16663 ) ;
#31354 = CARTESIAN_POINT ( 'NONE',  ( 119.8303681442453126, 0.4262465694468514643, -12.03445270309931736 ) ) ;
#31355 =( BOUNDED_SURFACE ( )  B_SPLINE_SURFACE ( 1, 2, ( 
 ( #35404, #755, #32218, #35175, #39068, #18775, #28817, #11710, #35855, #3953, #28360, #7838, #42274, #21292, #14906, #1432, #15353, #21744, #11037, #11492, #17875, #21518, #25397, #39294, #4629, #31771, #1215, #8063, #18550, #32442, #15129, #29036, #8288, #42945, #22190, #36086, #32664, #40197, #5745, #26290, #33553, #22863, #37204, #25836, #29260, #5524, #12391, #43171, #36756, #19444, #33327, #15802, #5976, #29936, #26064, #8964, #19902, #30162, #9189, #39968, #22637, #39743, #44081, #8730, #36535, #33787, #40653, #2101, #15576, #19665, #2331, #12161, #12845, #9408, #16028, #2558, #5309, #11940, #26746, #8511, #43850, #22415, #12619, #1875, #23095, #23318, #36308, #26520, #5076, #18993, #29481, #32881, #43617, #1655, #19225, #43394, #16261, #40429, #33105, #36977, #29704, #34891, #31053, #20800, #10104, #6451, #16487, #10538, #37895, #20135, #17165, #3465, #9876, #23786, #6674, #9639, #37675, #24440, #3239, #31271, #41563, #23561, #2790, #16940, #34021, #44310, #20581, #21017, #30387, #20359, #30610, #13517, #13065, #16717, #34245, #3018, #24226, #26964, #34680, #27426, #24008, #6890, #27649, #44528, #13958, #44982, #27869, #37442, #13291, #41347, #38116, #34460, #17382, #13740, #38331, #40885, #6214, #10323, #44758, #27199, #44 ),
 ( #41117, #41783, #7107, #30835, #28763, #486, #42222, #14174, #4574, #14399, #10983, #11655, #15074, #31938, #35119, #25344, #39238, #31717, #18499, #28986, #42446, #39468, #21466, #1158, #35577, #10763, #4124, #21691, #8002, #934, #21242, #22139, #42893, #265, #28541, #704, #28310, #28091, #42000, #35349, #7551, #24887, #3902, #24660, #21910, #25116, #32166, #25561, #8232, #31494, #3680, #4350, #18043, #35804, #7321, #14623, #11212, #38546, #39013, #17601, #42669, #17820, #38780, #18270, #7783, #14854, #11439, #32389, #43340, #32612, #40599, #29202, #36257, #5024, #18721, #30108, #1822, #9357, #40370, #2275, #43112, #36701, #18940, #9133, #8458, #19613, #36031, #36483, #5469, #5251, #11882, #1379, #23037, #16206, #22582, #33048, #1599, #43795, #12561, #19168, #32829, #4800, #8908, #15294, #26013, #25785, #36924, #44024, #12110, #39917, #43565, #39693, #29426, #19389, #5694, #22806, #22362, #33278, #15519, #33497, #8679, #12786, #26466, #15750, #29651, #12334, #26234, #40143, #2052, #26689, #15976, #29879, #2961, #6394, #34626, #6160, #13687, #9820, #13238, #2505, #33965, #17329, #37621, #3187, #10265, #44705, #20079, #27596, #3413, #20302, #27809, #41290, #30330, #41724, #41063, #6841, #31002, #34187, #9586, #44256, #17112 ) ),
 .UNSPECIFIED., .F., .F., .F. ) 
 B_SPLINE_SURFACE_WITH_KNOTS ( ( 2, 2 ),
 ( 3, 2, 2, 2, 2, 2, 2, 2, 2, 2, 2, 2, 2, 2, 2, 2, 2, 2, 2, 2, 2, 2, 2, 2, 2, 2, 2, 2, 2, 2, 2, 2, 2, 2, 2, 2, 2, 2, 2, 2, 2, 2, 2, 2, 2, 2, 2, 2, 2, 2, 2, 2, 2, 2, 2, 2, 2, 2, 2, 2, 2, 2, 2, 2, 2, 2, 2, 2, 2, 2, 2, 2, 2, 2, 2, 2, 2, 2, 2, 2, 3 ),
 ( 0.000000000000000000, 1.000000000000000000 ),
 ( 0.000000000000000000, 0.01250000000000000069, 0.02500000000000000139, 0.03749999999999999861, 0.05000000000000000278, 0.06250000000000000000, 0.07499999999999999722, 0.08749999999999999445, 0.1000000000000000056, 0.1125000000000000028, 0.1250000000000000000, 0.1375000000000000111, 0.1499999999999999944, 0.1625000000000000056, 0.1749999999999999889, 0.1875000000000000000, 0.2000000000000000111, 0.2124999999999999944, 0.2250000000000000056, 0.2374999999999999889, 0.2500000000000000000, 0.2625000000000000111, 0.2750000000000000222, 0.2874999999999999778, 0.2999999999999999889, 0.3125000000000000000, 0.3250000000000000111, 0.3375000000000000222, 0.3499999999999999778, 0.3624999999999999889, 0.3750000000000000000, 0.3875000000000000111, 0.4000000000000000222, 0.4124999999999999778, 0.4249999999999999889, 0.4375000000000000000, 0.4500000000000000111, 0.4625000000000000222, 0.4749999999999999778, 0.4874999999999999889, 0.5000000000000000000, 0.5124999999999999556, 0.5250000000000000222, 0.5374999999999999778, 0.5500000000000000444, 0.5625000000000000000, 0.5749999999999999556, 0.5875000000000000222, 0.5999999999999999778, 0.6125000000000000444, 0.6250000000000000000, 0.6374999999999999556, 0.6500000000000000222, 0.6624999999999999778, 0.6750000000000000444, 0.6875000000000000000, 0.6999999999999999556, 0.7125000000000000222, 0.7249999999999999778, 0.7375000000000000444, 0.7500000000000000000, 0.7624999999999999556, 0.7750000000000000222, 0.7874999999999999778, 0.8000000000000000444, 0.8125000000000000000, 0.8249999999999999556, 0.8375000000000000222, 0.8499999999999999778, 0.8625000000000000444, 0.8750000000000000000, 0.8874999999999999556, 0.9000000000000000222, 0.9124999999999999778, 0.9250000000000000444, 0.9375000000000000000, 0.9499999999999999556, 0.9625000000000000222, 0.9749999999999999778, 0.9875000000000000444, 1.000000000000000000 ),
 .UNSPECIFIED. ) 
 GEOMETRIC_REPRESENTATION_ITEM ( )  RATIONAL_B_SPLINE_SURFACE ( (
 ( 1.000000000000000000, 0.9238795325112869605, 1.000000000000000000, 0.9238795325112869605, 1.000000000000000000, 0.9238795325112869605, 1.000000000000000000, 0.9238795325112869605, 1.000000000000000000, 0.9238795325112869605, 1.000000000000000000, 0.9238795325112869605, 1.000000000000000000, 0.9238795325112869605, 1.000000000000000000, 0.9238795325112869605, 1.000000000000000000, 0.9238795325112869605, 1.000000000000000000, 0.9238795325112869605, 1.000000000000000000, 0.9238795325112869605, 1.000000000000000000, 0.9238795325112869605, 1.000000000000000000, 0.9238795325112869605, 1.000000000000000000, 0.9238795325112869605, 1.000000000000000000, 0.9238795325112869605, 1.000000000000000000, 0.9238795325112869605, 1.000000000000000000, 0.9238795325112869605, 1.000000000000000000, 0.9238795325112869605, 1.000000000000000000, 0.9238795325112869605, 1.000000000000000000, 0.9238795325112869605, 1.000000000000000000, 0.9238795325112869605, 1.000000000000000000, 0.9238795325112869605, 1.000000000000000000, 0.9238795325112869605, 1.000000000000000000, 0.9238795325112869605, 1.000000000000000000, 0.9238795325112869605, 1.000000000000000000, 0.9238795325112869605, 1.000000000000000000, 0.9238795325112869605, 1.000000000000000000, 0.9238795325112869605, 1.000000000000000000, 0.9238795325112869605, 1.000000000000000000, 0.9238795325112869605, 1.000000000000000000, 0.9238795325112869605, 1.000000000000000000, 0.9238795325112869605, 1.000000000000000000, 0.9238795325112869605, 1.000000000000000000, 0.9238795325112869605, 1.000000000000000000, 0.9238795325112869605, 1.000000000000000000, 0.9238795325112869605, 1.000000000000000000, 0.9238795325112869605, 1.000000000000000000, 0.9238795325112869605, 1.000000000000000000, 0.9238795325112869605, 1.000000000000000000, 0.9238795325112869605, 1.000000000000000000, 0.9238795325112869605, 1.000000000000000000, 0.9238795325112869605, 1.000000000000000000, 0.9238795325112869605, 1.000000000000000000, 0.9238795325112869605, 1.000000000000000000, 0.9238795325112869605, 1.000000000000000000, 0.9238795325112869605, 1.000000000000000000, 0.9238795325112869605, 1.000000000000000000, 0.9238795325112869605, 1.000000000000000000, 0.9238795325112869605, 1.000000000000000000, 0.9238795325112869605, 1.000000000000000000, 0.9238795325112869605, 1.000000000000000000, 0.9238795325112869605, 1.000000000000000000, 0.9238795325112869605, 1.000000000000000000, 0.9238795325112869605, 1.000000000000000000, 0.9238795325112869605, 1.000000000000000000, 0.9238795325112869605, 1.000000000000000000, 0.9238795325112869605, 1.000000000000000000, 0.9238795325112869605, 1.000000000000000000, 0.9238795325112869605, 1.000000000000000000, 0.9238795325112869605, 1.000000000000000000, 0.9238795325112869605, 1.000000000000000000, 0.9238795325112869605, 1.000000000000000000, 0.9238795325112869605, 1.000000000000000000, 0.9238795325112869605, 1.000000000000000000, 0.9238795325112869605, 1.000000000000000000, 0.9238795325112869605, 1.000000000000000000, 0.9238795325112869605, 1.000000000000000000, 0.9238795325112869605, 1.000000000000000000, 0.9238795325112869605, 1.000000000000000000, 0.9238795325112869605, 1.000000000000000000, 0.9238795325112869605, 1.000000000000000000, 0.9238795325112869605, 1.000000000000000000, 0.9238795325112869605, 1.000000000000000000, 0.9238795325112869605, 1.000000000000000000, 0.9238795325112869605, 1.000000000000000000, 0.9238795325112869605, 1.000000000000000000, 0.9238795325112869605, 1.000000000000000000, 0.9238795325112869605, 1.000000000000000000, 0.9238795325112869605, 1.000000000000000000, 0.9238795325112869605, 1.000000000000000000),
 ( 1.000000000000000000, 0.9238795325112869605, 1.000000000000000000, 0.9238795325112869605, 1.000000000000000000, 0.9238795325112869605, 1.000000000000000000, 0.9238795325112869605, 1.000000000000000000, 0.9238795325112869605, 1.000000000000000000, 0.9238795325112869605, 1.000000000000000000, 0.9238795325112869605, 1.000000000000000000, 0.9238795325112869605, 1.000000000000000000, 0.9238795325112869605, 1.000000000000000000, 0.9238795325112869605, 1.000000000000000000, 0.9238795325112869605, 1.000000000000000000, 0.9238795325112869605, 1.000000000000000000, 0.9238795325112869605, 1.000000000000000000, 0.9238795325112869605, 1.000000000000000000, 0.9238795325112869605, 1.000000000000000000, 0.9238795325112869605, 1.000000000000000000, 0.9238795325112869605, 1.000000000000000000, 0.9238795325112869605, 1.000000000000000000, 0.9238795325112869605, 1.000000000000000000, 0.9238795325112869605, 1.000000000000000000, 0.9238795325112869605, 1.000000000000000000, 0.9238795325112869605, 1.000000000000000000, 0.9238795325112869605, 1.000000000000000000, 0.9238795325112869605, 1.000000000000000000, 0.9238795325112869605, 1.000000000000000000, 0.9238795325112869605, 1.000000000000000000, 0.9238795325112869605, 1.000000000000000000, 0.9238795325112869605, 1.000000000000000000, 0.9238795325112869605, 1.000000000000000000, 0.9238795325112869605, 1.000000000000000000, 0.9238795325112869605, 1.000000000000000000, 0.9238795325112869605, 1.000000000000000000, 0.9238795325112869605, 1.000000000000000000, 0.9238795325112869605, 1.000000000000000000, 0.9238795325112869605, 1.000000000000000000, 0.9238795325112869605, 1.000000000000000000, 0.9238795325112869605, 1.000000000000000000, 0.9238795325112869605, 1.000000000000000000, 0.9238795325112869605, 1.000000000000000000, 0.9238795325112869605, 1.000000000000000000, 0.9238795325112869605, 1.000000000000000000, 0.9238795325112869605, 1.000000000000000000, 0.9238795325112869605, 1.000000000000000000, 0.9238795325112869605, 1.000000000000000000, 0.9238795325112869605, 1.000000000000000000, 0.9238795325112869605, 1.000000000000000000, 0.9238795325112869605, 1.000000000000000000, 0.9238795325112869605, 1.000000000000000000, 0.9238795325112869605, 1.000000000000000000, 0.9238795325112869605, 1.000000000000000000, 0.9238795325112869605, 1.000000000000000000, 0.9238795325112869605, 1.000000000000000000, 0.9238795325112869605, 1.000000000000000000, 0.9238795325112869605, 1.000000000000000000, 0.9238795325112869605, 1.000000000000000000, 0.9238795325112869605, 1.000000000000000000, 0.9238795325112869605, 1.000000000000000000, 0.9238795325112869605, 1.000000000000000000, 0.9238795325112869605, 1.000000000000000000, 0.9238795325112869605, 1.000000000000000000, 0.9238795325112869605, 1.000000000000000000, 0.9238795325112869605, 1.000000000000000000, 0.9238795325112869605, 1.000000000000000000, 0.9238795325112869605, 1.000000000000000000, 0.9238795325112869605, 1.000000000000000000, 0.9238795325112869605, 1.000000000000000000, 0.9238795325112869605, 1.000000000000000000, 0.9238795325112869605, 1.000000000000000000, 0.9238795325112869605, 1.000000000000000000, 0.9238795325112869605, 1.000000000000000000, 0.9238795325112869605, 1.000000000000000000, 0.9238795325112869605, 1.000000000000000000, 0.9238795325112869605, 1.000000000000000000, 0.9238795325112869605, 1.000000000000000000, 0.9238795325112869605, 1.000000000000000000, 0.9238795325112869605, 1.000000000000000000, 0.9238795325112869605, 1.000000000000000000, 0.9238795325112869605, 1.000000000000000000, 0.9238795325112869605, 1.000000000000000000, 0.9238795325112869605, 1.000000000000000000) ) ) 
 REPRESENTATION_ITEM ( '' )  SURFACE ( )  );
#31356 = AXIS2_PLACEMENT_3D ( 'NONE', #9034, #43242, #38185 ) ;
#31357 = CARTESIAN_POINT ( 'NONE',  ( 116.3133148109119759, -7.893985811506177619, -18.51759400769804742 ) ) ;
#31358 = CARTESIAN_POINT ( 'NONE',  ( 136.9165885681138377, 0.6403260112581466990, -12.97644181253951956 ) ) ;
#31359 = CARTESIAN_POINT ( 'NONE',  ( 114.6497546295247929, -4.863998795839590272, -7.631215200338315796 ) ) ;
#31360 = ORIENTED_EDGE ( 'NONE', *, *, #33165, .F. ) ;
#31361 = CIRCLE ( 'NONE', #39382, 2.445500000000004448 ) ;
#31362 = CARTESIAN_POINT ( 'NONE',  ( 70.19189222814998175, -58.90901798090458641, -36.76641099935233825 ) ) ;
#31363 = LINE ( 'NONE', #13825, #5518 ) ;
#31364 = DIRECTION ( 'NONE',  ( 0.9970811988817434024, -0.07634843047859724008, 0.000000000000000000 ) ) ;
#31365 = CARTESIAN_POINT ( 'NONE',  ( 113.5337081442453240, -9.261995988541697145, -16.69588392320189030 ) ) ;
#31366 = CARTESIAN_POINT ( 'NONE',  ( 64.24243542014160369, -41.01918285936451269, -15.89321520033831447 ) ) ;
#31367 = CARTESIAN_POINT ( 'NONE',  ( 121.9272896737536911, -8.611453504372539314, -17.77011218421760574 ) ) ;
#31368 = CARTESIAN_POINT ( 'NONE',  ( 63.78293339202748058, -12.80721147464382881, -16.09572056279317920 ) ) ;
#31369 = PLANE ( 'NONE',  #11297 ) ;
#31370 = CARTESIAN_POINT ( 'NONE',  ( 113.0523327545247838, -6.936859964151250502, -8.388885654883777576 ) ) ;
#31371 = CARTESIAN_POINT ( 'NONE',  ( 116.4834948109119779, -1.561330072975668504, -17.79121239304076951 ) ) ;
#31372 = DIRECTION ( 'NONE',  ( 1.000000000000000000, 0.000000000000000000, 0.000000000000000000 ) ) ;
#31373 = VECTOR ( 'NONE', #4525, 1000.000000000000000 ) ;
#31374 = CARTESIAN_POINT ( 'NONE',  ( 111.5098340574772777, -2.443475742715324639, -17.86549347949428679 ) ) ;
#31375 = CARTESIAN_POINT ( 'NONE',  ( 118.3661624739652183, 0.3208234527006367798, -15.99825685930877839 ) ) ;
#31376 = CARTESIAN_POINT ( 'NONE',  ( 123.3474214775786209, -0.1624402480850797581, -16.17319339645315424 ) ) ;
#31377 = ORIENTED_EDGE ( 'NONE', *, *, #550, .F. ) ;
#31378 = CARTESIAN_POINT ( 'NONE',  ( 135.3184548109119874, -9.609004340414083245, -9.721032963308941177 ) ) ;
#31379 = CARTESIAN_POINT ( 'NONE',  ( 122.0994348109119443, 0.9020085738987339008, -11.91225656197089222 ) ) ;
#31380 = CARTESIAN_POINT ( 'NONE',  ( 116.7333483795247844, -8.402594152722688392, -16.93181055722141792 ) ) ;
#31381 = CARTESIAN_POINT ( 'NONE',  ( 114.8384214775786489, -10.15424416112533912, -14.75197769757731336 ) ) ;
#31382 = CARTESIAN_POINT ( 'NONE',  ( 126.0703014775786102, -9.988377603198980381, -10.36322818467138518 ) ) ;
#31383 = FACE_OUTER_BOUND ( 'NONE', #18845, .T. ) ;
#31384 = CARTESIAN_POINT ( 'NONE',  ( 114.9275671295247889, -10.62599879583958540, -13.39321520033831447 ) ) ;
#31385 = CARTESIAN_POINT ( 'NONE',  ( 121.0216281442452981, -7.894159318335828068, -9.358103419637847864 ) ) ;
#31386 = AXIS2_PLACEMENT_3D ( 'NONE', #24115, #17054, #23439 ) ;
#31387 = CARTESIAN_POINT ( 'NONE',  ( 121.2485348109119769, -8.899110576539710493, -16.42337572283490132 ) ) ;
#31388 = CARTESIAN_POINT ( 'NONE',  ( 109.2294421309014751, -0.2315968891612809610, -10.77178248650439940 ) ) ;
#31389 = CARTESIAN_POINT ( 'NONE',  ( 122.7299391859119737, -8.844754642576884152, -8.592115655440050404 ) ) ;
#31390 = CARTESIAN_POINT ( 'NONE',  ( 108.0517077545248696, -2.791137627527939813, -18.39754474579286025 ) ) ;
#31391 = VECTOR ( 'NONE', #4556, 1000.000000000000114 ) ;
#31392 = CARTESIAN_POINT ( 'NONE',  ( 70.19189222814998175, -65.04786711941001442, -39.22192925582032785 ) ) ;
#31393 = CARTESIAN_POINT ( 'NONE',  ( 114.8951481442453115, -0.4660016031367893996, -10.09054647747474043 ) ) ;
#31394 = CARTESIAN_POINT ( 'NONE',  ( 114.7249681442453237, 0.2603800115204892296, -16.42320221600525088 ) ) ;
#31395 = CARTESIAN_POINT ( 'NONE',  ( 108.9545983795247821, -0.7896495226426338832, -9.318865927141430916 ) ) ;
#31396 = CARTESIAN_POINT ( 'NONE',  ( 122.3826735609119680, -9.645473719204776586, -14.86997237629376656 ) ) ;
#31397 = ORIENTED_EDGE ( 'NONE', *, *, #3335, .T. ) ;
#31398 = CARTESIAN_POINT ( 'NONE',  ( 117.1030726359456224, -1.179503403430467667, -17.05068175419387089 ) ) ;
#31399 = EDGE_CURVE ( 'NONE', #28588, #33070, #30370, .T. ) ;
#31400 = CARTESIAN_POINT ( 'NONE',  ( 122.3830681442452857, -8.166667518702819706, -8.995218007635861213 ) ) ;
#31401 = CARTESIAN_POINT ( 'NONE',  ( 114.5547881442453217, -5.638512984488999180, -18.83840828888717311 ) ) ;
#31402 = CARTESIAN_POINT ( 'NONE',  ( 118.4689281442453392, -10.15424416112533912, -14.75197769757731336 ) ) ;
#31403 = PRESENTATION_STYLE_ASSIGNMENT (( #17297 ) ) ;
#31404 = CARTESIAN_POINT ( 'NONE',  ( 111.6617281442453304, 0.4262465694468514643, -12.03445270309931736 ) ) ;
#31405 = CARTESIAN_POINT ( 'NONE',  ( 117.0507614775786465, -10.30919188438810075, -12.61870101168855918 ) ) ;
#31406 = EDGE_CURVE ( 'NONE', #39715, #32385, #37154, .T. ) ;
#31407 = CARTESIAN_POINT ( 'NONE',  ( 109.5796765045248122, -2.791137627527939813, -8.388885654883777576 ) ) ;
#31408 = CIRCLE ( 'NONE', #36516, 2.000000000000000444 ) ;
#31409 = CARTESIAN_POINT ( 'NONE',  ( 113.4202548109119846, 0.1319031606808879209, -14.10382304977623669 ) ) ;
#31410 = FACE_OUTER_BOUND ( 'NONE', #29463, .T. ) ;
#31411 = ORIENTED_EDGE ( 'NONE', *, *, #3535, .F. ) ;
#31412 = CARTESIAN_POINT ( 'NONE',  ( 121.3619881442452879, -4.089484607189486809, -7.948022111789456723 ) ) ;
#31413 = CARTESIAN_POINT ( 'NONE',  ( 120.1601735609119856, 0.6414057260225851653, -11.69287257290600657 ) ) ;
#31414 = CARTESIAN_POINT ( 'NONE',  ( 116.5969481442453031, 0.5811942927096154232, -14.16772938898807155 ) ) ;
#31415 = ORIENTED_EDGE ( 'NONE', *, *, #45118, .T. ) ;
#31416 = CARTESIAN_POINT ( 'NONE',  ( 107.5655358795247736, -8.402594152722688392, -9.854619843455216355 ) ) ;
#31417 = VECTOR ( 'NONE', #42006, 1000.000000000000000 ) ;
#31418 = CARTESIAN_POINT ( 'NONE',  ( 124.4819548109119722, -7.893985811506177619, -18.51759400769804742 ) ) ;
#31419 = CARTESIAN_POINT ( 'NONE',  ( 122.6099748109119929, -9.261995988541706026, -16.69588392320187609 ) ) ;
#31420 = CARTESIAN_POINT ( 'NONE',  ( 124.5059548109119731, -5.999156839134619723, -18.26265215102738892 ) ) ;
#31421 = EDGE_CURVE ( 'NONE', #37424, #10224, #12530, .T. ) ;
#31422 = CARTESIAN_POINT ( 'NONE',  ( 124.4871289243369006, -9.531683815157249384, -11.52482648355480599 ) ) ;
#31423 = CARTESIAN_POINT ( 'NONE',  ( 120.6245414775786458, -0.1624402480850797581, -16.17319339645315424 ) ) ;
#31424 = ADVANCED_FACE ( 'NONE', ( #9139 ), #16212, .T. ) ;
#31425 = EDGE_CURVE ( 'NONE', #511, #27420, #5964, .T. ) ;
#31426 = CARTESIAN_POINT ( 'NONE',  ( 120.5110881442453206, -3.505236298600246325, -18.68346056562440793 ) ) ;
#31427 = CARTESIAN_POINT ( 'NONE',  ( 125.2512653913890830, -10.90577519989732558, -9.364198568131605782 ) ) ;
#31428 = CARTESIAN_POINT ( 'NONE',  ( 121.0783548109119749, -9.565557343593413364, -10.61323700422348004 ) ) ;
#31429 = CARTESIAN_POINT ( 'NONE',  ( 122.7299391859119737, -8.844754642576884152, -8.592115655440050404 ) ) ;
#31430 = CARTESIAN_POINT ( 'NONE',  ( 117.5613014775786525, 0.9020085738987339008, -11.91225656197089222 ) ) ;
#31431 = CARTESIAN_POINT ( 'NONE',  ( 123.2339681442453099, -6.344957434206645708, -7.627207830600334582 ) ) ;
#31432 = CARTESIAN_POINT ( 'NONE',  ( 117.6180281442453150, -8.899110576539710493, -16.42337572283490132 ) ) ;
#31433 = ORIENTED_EDGE ( 'NONE', *, *, #21309, .F. ) ;
#31434 = CARTESIAN_POINT ( 'NONE',  ( 116.9940348109119839, -9.988377603198976828, -10.36322818467138340 ) ) ;
#31435 = CARTESIAN_POINT ( 'NONE',  ( 107.7044421295247929, 0.8980012041604618078, -13.39321520033831447 ) ) ;
#31436 = CARTESIAN_POINT ( 'NONE',  ( 115.9162281442453235, -5.574606645277192740, -18.38911715685844328 ) ) ;
#31437 = CARTESIAN_POINT ( 'NONE',  ( 113.9552233795247815, -1.325403438956533675, -9.854619843455175499 ) ) ;
#31438 = AXIS2_PLACEMENT_3D ( 'NONE', #4153, #31961, #14424 ) ;
#31439 = DIRECTION ( 'NONE',  ( -0.000000000000000000, -0.9284778069183721172, -0.3713878862591650232 ) ) ;
#31440 = CARTESIAN_POINT ( 'NONE',  ( 123.2339681442453241, -6.344957434206665248, -7.627207830600338134 ) ) ;
#31441 = ORIENTED_EDGE ( 'NONE', *, *, #16225, .F. ) ;
#31442 = CARTESIAN_POINT ( 'NONE',  ( 118.3578375202278181, -2.239543233855014748, -18.13706010537466895 ) ) ;
#31443 = CARTESIAN_POINT ( 'NONE',  ( 117.6747548109119919, -7.643976991954077427, -18.09477374809248928 ) ) ;
#31444 = DIRECTION ( 'NONE',  ( 0.9609149988134837450, -0.1028163501681639419, 0.2570431154366518145 ) ) ;
#31445 = CARTESIAN_POINT ( 'NONE',  ( 63.69952534844841807, -14.91276996408597810, -16.69749735386625744 ) ) ;
#31446 = CARTESIAN_POINT ( 'NONE',  ( 125.3328548109119964, -9.261995988541697145, -16.69588392320189030 ) ) ;
#31447 = CARTESIAN_POINT ( 'NONE',  ( 111.5243640045248412, 0.1403307496149616695, -15.46607636864997204 ) ) ;
#31448 = CARTESIAN_POINT ( 'NONE',  ( 89.14456494507275863, -10.39963736880928380, -14.05985968316478640 ) ) ;
#31449 = EDGE_CURVE ( 'NONE', #32536, #4879, #30933, .T. ) ;
#31450 = VERTEX_POINT ( 'NONE', #31891 ) ;
#31451 = CARTESIAN_POINT ( 'NONE',  ( 113.4202548109119846, -10.30919188438810075, -12.61870101168855918 ) ) ;
#31452 = CARTESIAN_POINT ( 'NONE',  ( 112.8529881442453302, -1.561330072975668060, -17.79121239304076596 ) ) ;
#31453 = CARTESIAN_POINT ( 'NONE',  ( 123.7445081442452874, -1.561330072975668948, -17.79121239304076951 ) ) ;
#31454 = CARTESIAN_POINT ( 'NONE',  ( 118.0718414775786442, -0.8288870151387760510, -10.36305467784173118 ) ) ;
#31455 = CARTESIAN_POINT ( 'NONE',  ( 82.43378680891619581, -31.75787105231993479, -22.77522651806478748 ) ) ;
#31456 = SURFACE_STYLE_USAGE ( .BOTH. , #35540 ) ;
#31457 = CARTESIAN_POINT ( 'NONE',  ( 117.6180281442453150, -0.4660016031367893996, -10.09054647747474043 ) ) ;
#31458 = CYLINDRICAL_SURFACE ( 'NONE', #18409, 4.999999999999998224 ) ;
#31459 = DIRECTION ( 'NONE',  ( -1.000000000000000000, 0.000000000000000000, 0.000000000000000000 ) ) ;
#31460 = CARTESIAN_POINT ( 'NONE',  ( 123.2906948109119867, -1.833838273342659697, -17.42832698103878286 ) ) ;
#31461 = ORIENTED_EDGE ( 'NONE', *, *, #27585, .T. ) ;
#31462 = EDGE_CURVE ( 'NONE', #13605, #11206, #25064, .T. ) ;
#31463 = LINE ( 'NONE', #34211, #38722 ) ;
#31464 = CARTESIAN_POINT ( 'NONE',  ( 116.5969481442453031, 0.5811942927096154232, -14.16772938898807155 ) ) ;
#31465 = CARTESIAN_POINT ( 'NONE',  ( 136.6675107540889371, -8.468615216776449017, -17.76661867765510650 ) ) ;
#31466 = VERTEX_POINT ( 'NONE', #21413 ) ;
#31467 = CARTESIAN_POINT ( 'NONE',  ( 137.5098831408856768, -0.7887024016652356417, -10.49420813250452866 ) ) ;
#31468 = CARTESIAN_POINT ( 'NONE',  ( 121.3052614775786111, -1.834011780172310813, -8.268836392978581529 ) ) ;
#31469 = CARTESIAN_POINT ( 'NONE',  ( 107.9128015045248219, -2.477300249445798297, -7.631215200338321125 ) ) ;
#31470 = CARTESIAN_POINT ( 'NONE',  ( 121.0783548109119749, -9.565557343593413364, -10.61323700422348004 ) ) ;
#31471 = ORIENTED_EDGE ( 'NONE', *, *, #12029, .F. ) ;
#31472 = VERTEX_POINT ( 'NONE', #35067 ) ;
#31473 = CIRCLE ( 'NONE', #22752, 0.4999999999999999445 ) ;
#31474 = CARTESIAN_POINT ( 'NONE',  ( 113.4769814775786330, -10.63000616557722466, -14.87417383870573495 ) ) ;
#31475 = CARTESIAN_POINT ( 'NONE',  ( 124.5386814775786206, -4.153390946401325223, -8.397313243818185668 ) ) ;
#31476 = CARTESIAN_POINT ( 'NONE',  ( 112.4925368734311206, -1.223627541775731631, -16.99192386690444323 ) ) ;
#31477 = EDGE_CURVE ( 'NONE', #19939, #12295, #13988, .T. ) ;
#31478 = CARTESIAN_POINT ( 'NONE',  ( 113.7798197424434363, -0.9924539043446216624, -17.29976612834909133 ) ) ;
#31479 = CARTESIAN_POINT ( 'NONE',  ( 123.6877814775786533, -3.383040157471821630, -19.15922257007629170 ) ) ;
#31480 = CARTESIAN_POINT ( 'NONE',  ( 85.43169907558235820, -25.38011337280982715, -14.88121679464376257 ) ) ;
#31481 = AXIS2_PLACEMENT_3D ( 'NONE', #8434, #39670, #7979 ) ;
#31482 = CARTESIAN_POINT ( 'NONE',  ( 70.19189222814998175, -51.12070001563444066, -33.65111096193285078 ) ) ;
#31483 = CARTESIAN_POINT ( 'NONE',  ( 125.1626748109119802, -9.988377603198980381, -10.36322818467138518 ) ) ;
#31485 = CARTESIAN_POINT ( 'NONE',  ( 124.9924948109119924, -5.574606645277164318, -18.38911715685844683 ) ) ;
#31484 = CARTESIAN_POINT ( 'NONE',  ( 122.7234281442452755, -5.638512984488999180, -18.83840828888717311 ) ) ;
#31486 = EDGE_CURVE ( 'NONE', #21469, #24351, #29283, .T. ) ;
#31487 = CARTESIAN_POINT ( 'NONE',  ( 120.3976348109119812, -7.643976991954077427, -18.09477374809248928 ) ) ;
#31488 = CARTESIAN_POINT ( 'NONE',  ( 125.6059481442453318, -7.866424907534184996, -9.395035934245763443 ) ) ;
#31489 = CARTESIAN_POINT ( 'NONE',  ( 115.6325948109119821, 0.2603800115204892296, -16.42320221600525088 ) ) ;
#31490 = ORIENTED_EDGE ( 'NONE', *, *, #17797, .F. ) ;
#31491 = LINE ( 'NONE', #34888, #12546 ) ;
#31492 = CARTESIAN_POINT ( 'NONE',  ( 113.5385046295247804, -4.863998795839590272, -18.39754474579285315 ) ) ;
#31493 = CARTESIAN_POINT ( 'NONE',  ( 108.6073327545248048, -6.936859964151250502, -8.388885654883777576 ) ) ;
#31494 = CARTESIAN_POINT ( 'NONE',  ( 112.6356140045247827, 0.1403307496149616695, -15.46607636864997204 ) ) ;
#31495 = CARTESIAN_POINT ( 'NONE',  ( 124.5386814775786206, -5.638512984488999180, -18.83840828888717311 ) ) ;
#31496 = CARTESIAN_POINT ( 'NONE',  ( 112.6260814775786514, -9.261995988541697145, -16.69588392320189030 ) ) ;
#31497 = VERTEX_POINT ( 'NONE', #210 ) ;
#31498 = CARTESIAN_POINT ( 'NONE',  ( 114.4980614775786734, -2.084020599724406786, -8.691656652584148546 ) ) ;
#31499 = CARTESIAN_POINT ( 'NONE',  ( 112.4272546295247821, -4.863998795839590272, -7.631215200338315796 ) ) ;
#31500 = CARTESIAN_POINT ( 'NONE',  ( 122.2128881442452979, -7.643976991954104960, -18.09477374809246442 ) ) ;
#31501 = CARTESIAN_POINT ( 'NONE',  ( 124.0281414775786146, -1.834011780172310813, -8.268836392978581529 ) ) ;
#31502 = CARTESIAN_POINT ( 'NONE',  ( 124.8790414775786246, -0.4660016031367893996, -10.09054647747474043 ) ) ;
#31503 = DIRECTION ( 'NONE',  ( 0.000000000000000000, 0.9284778069183720062, 0.3713878862591650232 ) ) ;
#31504 = CARTESIAN_POINT ( 'NONE',  ( 114.2711548109119803, -9.988377603198976828, -10.36322818467138340 ) ) ;
#31505 = CARTESIAN_POINT ( 'NONE',  ( 115.5526452545247622, 0.8980012041604421569, -11.00651665394454071 ) ) ;
#31506 = CARTESIAN_POINT ( 'NONE',  ( 114.8581140045248361, 0.1403307496149616695, -15.46607636864997204 ) ) ;
#31507 = ORIENTED_EDGE ( 'NONE', *, *, #30017, .F. ) ;
#31508 = CARTESIAN_POINT ( 'NONE',  ( 70.19189222814998175, -60.40547808481815650, -37.36498982452450690 ) ) ;
#31509 = CARTESIAN_POINT ( 'NONE',  ( 116.0296814775786345, -1.833838273342658809, -17.42832698103878286 ) ) ;
#31510 = AXIS2_PLACEMENT_3D ( 'NONE', #765, #14688, #7165 ) ;
#31511 = CARTESIAN_POINT ( 'NONE',  ( 126.5808414775786446, -9.859900752359378018, -12.68260735090039759 ) ) ;
#31512 = CARTESIAN_POINT ( 'NONE',  ( 113.4690515045247992, -2.477300249445798297, -7.631215200338321125 ) ) ;
#31513 = CARTESIAN_POINT ( 'NONE',  ( 107.7044421295247929, -9.868328341294093420, -13.39321520033831447 ) ) ;
#31514 = CARTESIAN_POINT ( 'NONE',  ( 120.0005481442453146, -4.153390946401325223, -8.397313243818185668 ) ) ;
#31515 = CARTESIAN_POINT ( 'NONE',  ( 119.8870948109119752, -0.8288870151387760510, -10.36305467784173118 ) ) ;
#31516 = CARTESIAN_POINT ( 'NONE',  ( 113.8740681442453138, -9.859900752359374465, -12.68260735090039404 ) ) ;
#31517 = ORIENTED_EDGE ( 'NONE', *, *, #42098, .F. ) ;
#31518 = COLOUR_RGB ( '',0.7921568627450980005, 0.8196078431372548767, 0.9333333333333333481 ) ;
#31519 = CARTESIAN_POINT ( 'NONE',  ( 121.0630641859119976, -8.321307733199551748, -9.223433127585318303 ) ) ;
#31520 = VECTOR ( 'NONE', #134, 1000.000000000000227 ) ;
#31521 = CARTESIAN_POINT ( 'NONE',  ( -12.36826994950263625, -4.374949827406447334, -18.19321520033831519 ) ) ;
#31522 = CARTESIAN_POINT ( 'NONE',  ( 113.7038881442453402, -6.222761293078241884, -8.102969835052219238 ) ) ;
#31523 = VERTEX_POINT ( 'NONE', #3630 ) ;
#31524 = DIRECTION ( 'NONE',  ( 0.9609149988134837450, -0.1028163501681639419, 0.2570431154366518145 ) ) ;
#31525 = EDGE_CURVE ( 'NONE', #19842, #37411, #33570, .T. ) ;
#31526 = CARTESIAN_POINT ( 'NONE',  ( 105.6208483795248299, -0.7896495226426338832, -9.318865927141430916 ) ) ;
#31527 = CARTESIAN_POINT ( 'NONE',  ( 108.9545983795247821, -8.402594152722688392, -16.93181055722141792 ) ) ;
#31528 = ORIENTED_EDGE ( 'NONE', *, *, #37844, .T. ) ;
#31529 = CARTESIAN_POINT ( 'NONE',  ( 116.9940348109119839, -0.1624402480850797581, -16.17319339645315424 ) ) ;
#31530 = CARTESIAN_POINT ( 'NONE',  ( 114.2144281442453178, -1.833838273342658809, -17.42832698103878286 ) ) ;
#31531 = CYLINDRICAL_SURFACE ( 'NONE', #3467, 2.999999999999998668 ) ;
#31532 = CARTESIAN_POINT ( 'NONE',  ( 122.2437673109119629, 0.2312338769422704887, -16.08380026872395874 ) ) ;
#31533 = VERTEX_POINT ( 'NONE', #24834 ) ;
#31534 = AXIS2_PLACEMENT_3D ( 'NONE', #1832, #36711, #44035 ) ;
#31535 = CARTESIAN_POINT ( 'NONE',  ( 121.2607668052895491, -1.125321370491285444, -17.12283323191017814 ) ) ;
#31536 = CARTESIAN_POINT ( 'NONE',  ( 124.1685108350147857, -2.421128313536792032, -5.786646012007111040 ) ) ;
#31537 = CARTESIAN_POINT ( 'NONE',  ( 114.9970202545248412, -10.62599879583958717, -15.77991374673208469 ) ) ;
#31538 = ADVANCED_FACE ( 'NONE', ( #21638 ), #37274, .T. ) ;
#31539 = CARTESIAN_POINT ( 'NONE',  ( 113.1366214775786432, -1.834011780172310813, -8.268836392978581529 ) ) ;
#31540 = CARTESIAN_POINT ( 'NONE',  ( 123.1205148109119563, -7.643976991954077427, -18.09477374809248928 ) ) ;
#31541 = CARTESIAN_POINT ( 'NONE',  ( 115.9729548109119861, -3.505236298600246325, -18.68346056562440793 ) ) ;
#31542 = DIRECTION ( 'NONE',  ( -1.000000000000000000, 0.000000000000000000, 0.000000000000000000 ) ) ;
#31543 = ORIENTED_EDGE ( 'NONE', *, *, #45139, .T. ) ;
#31544 = DIRECTION ( 'NONE',  ( 0.000000000000000000, -0.3818493186865936084, 0.9242245927363024194 ) ) ;
#31545 = CARTESIAN_POINT ( 'NONE',  ( 114.7249681442453237, -9.565557343593413364, -10.61323700422348004 ) ) ;
#31546 = CYLINDRICAL_SURFACE ( 'NONE', #29169, 1.999999999999998890 ) ;
#31547 = CIRCLE ( 'NONE', #42501, 2.000000000000000444 ) ;
#31548 = CARTESIAN_POINT ( 'NONE',  ( 85.85157537343363288, -26.34233955809028060, -8.371160363714436059 ) ) ;
#31549 = CARTESIAN_POINT ( 'NONE',  ( 125.7299414775786346, 0.9020085738987339008, -11.91225656197089222 ) ) ;
#31550 = CARTESIAN_POINT ( 'NONE',  ( 116.3133148109119759, -7.893985811506177619, -18.51759400769804742 ) ) ;
#31551 = ORIENTED_EDGE ( 'NONE', *, *, #16681, .F. ) ;
#31552 = CARTESIAN_POINT ( 'NONE',  ( 117.9583881442453048, -10.30919188438810075, -12.61870101168855918 ) ) ;
#31553 = CARTESIAN_POINT ( 'NONE',  ( 114.2144281442453178, -8.166667518702809048, -8.995218007635852331 ) ) ;
#31554 = CARTESIAN_POINT ( 'NONE',  ( 112.2883483795247770, -0.7896495226426338832, -9.318865927141430916 ) ) ;
#31555 = CARTESIAN_POINT ( 'NONE',  ( 111.8886348109120092, -3.383040157471821630, -19.15922257007629170 ) ) ;
#31556 = CARTESIAN_POINT ( 'NONE',  ( 115.1220548109119761, -8.166667518702817929, -8.995218007635861213 ) ) ;
#31557 = CARTESIAN_POINT ( 'NONE',  ( 123.4608748109119745, 0.4262465694468514643, -12.03445270309931736 ) ) ;
#31558 = CARTESIAN_POINT ( 'NONE',  ( 77.44400397045842510, -3.459648945705700473, -7.147228641687434880 ) ) ;
#31559 = CARTESIAN_POINT ( 'NONE',  ( 110.8298327545248299, -6.936859964151250502, -8.388885654883777576 ) ) ;
#31560 = VERTEX_POINT ( 'NONE', #10269 ) ;
#31561 = CARTESIAN_POINT ( 'NONE',  ( 120.3531401386228907, -1.125321370491285444, -17.12283323191017814 ) ) ;
#31562 = CARTESIAN_POINT ( 'NONE',  ( 109.2294420515965783, -4.107973114216393995, -18.49262090093784039 ) ) ;
#31563 = CARTESIAN_POINT ( 'NONE',  ( 115.3489614775786407, -0.8288870151387760510, -10.36305467784173118 ) ) ;
#31564 = CARTESIAN_POINT ( 'NONE',  ( 106.7320983795247855, -0.7896495226426338832, -9.318865927141430916 ) ) ;
#31565 = CARTESIAN_POINT ( 'NONE',  ( 116.5944421295247793, -9.868328341294093420, -13.39321520033831447 ) ) ;
#31566 = CARTESIAN_POINT ( 'NONE',  ( 109.5796765045248122, -7.250697342233347165, -19.15521520033831138 ) ) ;
#31567 = CARTESIAN_POINT ( 'NONE',  ( 121.4964260444391755, -1.267766418764731728, -16.93314635290706605 ) ) ;
#31568 = CARTESIAN_POINT ( 'NONE',  ( 124.5954081442453116, -3.383040157471821630, -19.15922257007629170 ) ) ;
#31569 = CARTESIAN_POINT ( 'NONE',  ( 92.04708369096698561, -25.99489077589524300, -13.39321520033831625 ) ) ;
#31570 = CARTESIAN_POINT ( 'NONE',  ( 125.1626748109119802, -9.988377603198980381, -10.36322818467138518 ) ) ;
#31571 = CARTESIAN_POINT ( 'NONE',  ( 115.6325948109119821, 0.2603800115204892296, -16.42320221600525088 ) ) ;
#31572 = ORIENTED_EDGE ( 'NONE', *, *, #29390, .F. ) ;
#31573 = VECTOR ( 'NONE', #30298, 1000.000000000000114 ) ;
#31574 = CARTESIAN_POINT ( 'NONE',  ( 113.4202548109119846, 0.1319031606808879209, -14.10382304977623669 ) ) ;
#31575 = VECTOR ( 'NONE', #6223, 999.9999999999998863 ) ;
#31576 = CARTESIAN_POINT ( 'NONE',  ( 113.0231681442453322, 0.9020085738987339008, -11.91225656197089222 ) ) ;
#31577 = CARTESIAN_POINT ( 'NONE',  ( 118.9794681442453026, -9.261995988541697145, -16.69588392320189030 ) ) ;
#31578 = B_SPLINE_CURVE_WITH_KNOTS ( 'NONE', 3,
 ( #19147, #37130, #30090, #26215, #5677, #26890, #22787, #2032, #29861, #12541 ),
 .UNSPECIFIED., .F., .F.,
 ( 4, 3, 3, 4 ),
 ( 0.000000000000000000, 0.0001671877548681270013, 0.0003343755096277669986, 0.0006463528481650629171 ),
 .UNSPECIFIED. ) ;
#31579 = CARTESIAN_POINT ( 'NONE',  ( 117.2776681442452968, -4.153390946401325223, -8.397313243818185668 ) ) ;
#31580 = ORIENTED_EDGE ( 'NONE', *, *, #35841, .F. ) ;
#31581 = CARTESIAN_POINT ( 'NONE',  ( 122.7234281442452755, -4.153390946401325223, -8.397313243818185668 ) ) ;
#31582 = AXIS2_PLACEMENT_3D ( 'NONE', #14496, #28191, #11304 ) ;
#31583 = CARTESIAN_POINT ( 'NONE',  ( 118.2987481442453088, -1.561330072975668504, -17.79121239304076951 ) ) ;
#31584 = DIRECTION ( 'NONE',  ( 0.000000000000000000, -1.000000000000000000, 0.000000000000000000 ) ) ;
#31585 = CARTESIAN_POINT ( 'NONE',  ( 108.7462390045248242, 0.8980012041604421569, -15.77991374673208469 ) ) ;
#31586 = FACE_OUTER_BOUND ( 'NONE', #41786, .T. ) ;
#31587 = DIRECTION ( 'NONE',  ( 0.000000000000000000, -0.6004852223388321697, 0.7996358532186280677 ) ) ;
#31588 = FACE_OUTER_BOUND ( 'NONE', #19049, .T. ) ;
#31589 = CARTESIAN_POINT ( 'NONE',  ( 114.0442481442453300, -1.834011780172310813, -8.268836392978581529 ) ) ;
#31590 = ADVANCED_FACE ( 'NONE', ( #39186 ), #8874, .T. ) ;
#31591 = CARTESIAN_POINT ( 'NONE',  ( 137.2865145795256581, -10.09372725149439276, -13.46056636665518091 ) ) ;
#31592 = CARTESIAN_POINT ( 'NONE',  ( 121.6065266009169221, -8.403782945130238602, -17.37684090985456820 ) ) ;
#31593 = CARTESIAN_POINT ( 'NONE',  ( 59.73260846536648927, -12.72599336462991282, -17.39039534737584347 ) ) ;
#31594 = CARTESIAN_POINT ( 'NONE',  ( 128.2184548109119930, -4.863998795839242995, -13.39321520033831447 ) ) ;
#31595 = CARTESIAN_POINT ( 'NONE',  ( 114.9275671295247889, 0.1403307496149613920, -13.39321520033831447 ) ) ;
#31596 = CARTESIAN_POINT ( 'NONE',  ( 113.8173414775786512, -9.565557343593413364, -10.61323700422348004 ) ) ;
#31597 = AXIS2_PLACEMENT_3D ( 'NONE', #13942, #17368, #468 ) ;
#31598 =( NAMED_UNIT ( * ) SI_UNIT ( $, .STERADIAN. ) SOLID_ANGLE_UNIT ( ) );
#31599 = CARTESIAN_POINT ( 'NONE',  ( 90.04708369096697140, -26.19154317501883611, -12.91723953507911915 ) ) ;
#31601 = CARTESIAN_POINT ( 'NONE',  ( 116.4834948109119779, -1.561330072975668504, -17.79121239304076951 ) ) ;
#31600 = DIRECTION ( 'NONE',  ( 0.000000000000000000, -0.3818493186865936084, 0.9242245927363024194 ) ) ;
#31602 = LINE ( 'NONE', #14061, #33605 ) ;
#31603 = CARTESIAN_POINT ( 'NONE',  ( 120.2841814775786276, -10.15424416112533912, -14.75197769757731336 ) ) ;
#31604 = ORIENTED_EDGE ( 'NONE', *, *, #44365, .T. ) ;
#31605 = CARTESIAN_POINT ( 'NONE',  ( 136.6675107540776821, -9.237402273161876565, -9.788598779400610184 ) ) ;
#31606 = CARTESIAN_POINT ( 'NONE',  ( 124.0848681442452772, -4.089484607189486809, -7.948022111789456723 ) ) ;
#31607 = CARTESIAN_POINT ( 'NONE',  ( 115.5526452545247622, -9.868328341294098749, -15.46607636864997204 ) ) ;
#31608 = CARTESIAN_POINT ( 'NONE',  ( 114.9518748109119883, -7.643976991954077427, -18.09477374809248928 ) ) ;
#31609 = CARTESIAN_POINT ( 'NONE',  ( 112.9097148109120070, -9.565557343593413364, -10.61323700422348004 ) ) ;
#31610 = CARTESIAN_POINT ( 'NONE',  ( 96.54708369096698561, -23.81115550238859413, -13.04821483042134389 ) ) ;
#31611 = CARTESIAN_POINT ( 'NONE',  ( 114.0941296295247867, -4.863998795839590272, -19.15521520033831493 ) ) ;
#31612 = CARTESIAN_POINT ( 'NONE',  ( 119.6601881442453106, -1.833838273342659253, -17.42832698103878286 ) ) ;
#31613 = CARTESIAN_POINT ( 'NONE',  ( 121.7590748109119687, -2.084020599724406786, -8.691656652584148546 ) ) ;
#31614 = CARTESIAN_POINT ( 'NONE',  ( 114.3278814775786429, 0.1319031606808870605, -14.10382304977625090 ) ) ;
#31615 = PLANE ( 'NONE',  #11005 ) ;
#31616 = FACE_OUTER_BOUND ( 'NONE', #23270, .T. ) ;
#31617 = CARTESIAN_POINT ( 'NONE',  ( 109.5796765045248122, -2.791137627527939813, -8.388885654883777576 ) ) ;
#31618 = CARTESIAN_POINT ( 'NONE',  ( 116.4579757138558023, 2.222835611391195343, -20.43720749888801080 ) ) ;
#31619 = CARTESIAN_POINT ( 'NONE',  ( 116.7104014775786425, -0.4660016031367893996, -10.09054647747474043 ) ) ;
#31620 = CARTESIAN_POINT ( 'NONE',  ( 115.6893214775786447, 0.5811942927096154232, -14.16772938898807155 ) ) ;
#31621 = CARTESIAN_POINT ( 'NONE',  ( 110.4131140045248287, -10.62599879583958717, -11.00651665394454604 ) ) ;
#31622 =( BOUNDED_SURFACE ( )  B_SPLINE_SURFACE ( 1, 2, ( 
 ( #40848, #19863, #30569, #8923, #15992, #30127, #9603, #16222, #23518, #12804, #27158, #15147, #18568, #44040, #22825, #41080, #16448, #30348, #26926, #2521, #9373, #13255, #6175, #37406, #5712, #23746, #20096, #40388, #2750, #9836, #32460, #36716, #9149, #16673, #44489, #40616, #23055, #37637, #1235, #19406, #36942, #23282, #37166, #5941, #43813, #29669, #43581, #12351, #33752, #33293, #44272, #19630, #13028, #33514, #2294, #13481, #13918, #17127, #21201, #10725, #38078, #3860, #223, #17346, #17782, #14136, #31015, #28052, #41960, #37854, #24625, #24186, #27828, #20542, #31675, #7, #16905, #42183, #31235, #2977, #38508, #30797, #7285, #35079, #41739, #34421, #14361, #41524, #10943, #44722, #10503, #23968, #44945, #3202, #6629, #13703, #445, #3641, #27610, #28274, #24847, #6411, #38293, #20318, #31454, #27384, #10282, #6856, #20763, #34202, #24404, #41307, #10067, #7072, #34642, #3428, #20982, #34855, #17560, #42631, #1341, #25750, #29161, #25304, #43302, #15255, #14812, #11843, #32790, #38739, #667, #28725, #22325, #43075, #4538, #11395, #39656, #8419, #25075, #32125, #15036, #18462, #28947, #35536, #29389, #35307, #4079, #11614, #11171, #32352, #14583, #4761, #39196, #1118, #28501, #42855, #4308, #36221, #4986, #7962, #18899, #32574, #25525, #1562, #15485, #18230, #12071, #7508, #38968, #21423, #21873, #39429, #7737, #18003, #8194, #31901, #42407, #22102, #21647, #893, #35768, #35990, #18683, #33457, #40104, #33921, #15940, #30515, #22544, #16168, #43529, #19354, #8865, #26197, #22766, #19807, #23230, #12298, #44217, #33695, #2692, #12747, #40790, #5885, #33012, #36663, #26424, #5436, #8644, #30071, #44437, #25973, #19577, #29840, #16622, #15711, #33242, #43758, #12524, #2466, #29614, #16390, #40331, #37112, #1786, #26648, #9096, #30290, #40563, #37348, #2015, #22997, #36888, #12978, #5658, #26873, #2236, #39879, #36442, #5210, #43983, #9322, #19129, #9547, #23462, #6121, #20039, #3375, #7232, #45105, #3155, #34806, #13864, #24576, #20266, #10010, #24136 ),
 ( #23919, #30968, #6804, #27777, #27105, #23695, #21149, #31627, #28003, #38461, #37800, #41689, #170, #27334, #35022, #24354, #37581, #14086, #3805, #6576, #20713, #17730, #13204, #41252, #44891, #30744, #17295, #17075, #10451, #34592, #31187, #41027, #16852, #20493, #10229, #13651, #38242, #41909, #9780, #7021, #3592, #6354, #27557, #20932, #34373, #44668, #41470, #34152, #2922, #17503, #31401, #10673, #13430, #38029, #35714, #28446, #395, #28227, #38912, #25698, #7683, #25249, #17952, #21371, #18847, #21597, #4031, #1069, #839, #7912, #11339, #32302, #25019, #42133, #11790, #39147, #4711, #21819, #39379, #35484, #24793, #8146, #14758, #4932, #7451, #35254, #14308, #10893, #31851, #29110, #38686, #28674, #14982, #42577, #621, #14531, #18632, #39605, #32071, #4488, #18410, #28894, #11119, #8366, #42357, #4257, #42806, #18175, #11567, #22049, #35942, #25474, #32519, #1294, #15206, #43022, #22271, #36165, #15432, #44162, #26370, #37058, #12470, #26596, #12246, #12018, #40509, #33185, #37289, #39825, #8593, #32738, #6059, #5157, #16337, #1513, #1960, #2179, #15888, #25921, #29339, #5830, #12926, #19306, #29784, #43696, #33404, #43479, #26822, #29562, #43253, #5604, #22491, #36385, #9269, #23180, #40045, #19074, #32960, #40734, #1736, #26143, #16110, #19751, #19527, #15661, #30011, #8813, #30240, #22715, #9490, #33635, #36614, #5389, #40279, #9044, #43929, #22943, #36835, #23406, #12696, #2410, #124, #16797, #3320, #6972, #34100, #31349, #31132, #30464, #20881, #41860, #13379, #13595, #24524, #19979, #2868, #6524, #37522, #24084, #23868, #20664, #27504, #41423, #10622, #23636, #30694, #17025, #37754, #37979, #3539, #16569, #6753, #10399, #44384, #34324, #17241, #44612, #6295, #27280, #14036, #38411, #41644, #10178, #17454, #34539, #9955, #45056, #41195, #33868, #2637, #20440, #27953, #3097, #44839, #20215, #40969, #13147, #30916, #13816, #27727, #27051, #24309, #9724, #38195, #34756, #24737, #570, #21320, #7402, #35206, #1016, #4436, #38626, #25423, #14932, #15154 ) ),
 .UNSPECIFIED., .F., .F., .T. ) 
 B_SPLINE_SURFACE_WITH_KNOTS ( ( 2, 2 ),
 ( 3, 2, 2, 2, 2, 2, 2, 2, 2, 2, 2, 2, 2, 2, 2, 2, 2, 2, 2, 2, 2, 2, 2, 2, 2, 2, 2, 2, 2, 2, 2, 2, 2, 2, 2, 2, 2, 2, 2, 2, 2, 2, 2, 2, 2, 2, 2, 2, 2, 2, 2, 2, 2, 2, 2, 2, 2, 2, 2, 2, 2, 2, 2, 2, 2, 2, 2, 2, 2, 2, 2, 2, 2, 2, 2, 2, 2, 2, 2, 2, 2, 2, 2, 2, 2, 2, 2, 2, 2, 2, 2, 2, 2, 2, 2, 2, 2, 2, 2, 2, 2, 2, 2, 2, 2, 2, 2, 2, 2, 2, 2, 2, 2, 2, 2, 2, 2, 2, 2, 2, 2, 2, 2, 2, 2, 2, 2, 2, 3 ),
 ( 0.000000000000000000, 1.000000000000000000 ),
 ( 0.000000000000000000, 0.007812500000000000000, 0.01562500000000000000, 0.02343750000000000000, 0.03125000000000000000, 0.03906250000000000000, 0.04687500000000000000, 0.05468750000000000000, 0.06250000000000000000, 0.07031250000000000000, 0.07812500000000000000, 0.08593750000000000000, 0.09375000000000000000, 0.1015625000000000000, 0.1093750000000000000, 0.1171875000000000000, 0.1250000000000000000, 0.1328125000000000000, 0.1406250000000000000, 0.1484375000000000000, 0.1562500000000000000, 0.1640625000000000000, 0.1718750000000000000, 0.1796875000000000000, 0.1875000000000000000, 0.1953125000000000000, 0.2031250000000000000, 0.2109375000000000000, 0.2187500000000000000, 0.2265625000000000000, 0.2343750000000000000, 0.2421875000000000000, 0.2500000000000000000, 0.2578125000000000000, 0.2656250000000000000, 0.2734375000000000000, 0.2812500000000000000, 0.2890625000000000000, 0.2968750000000000000, 0.3046875000000000000, 0.3125000000000000000, 0.3203125000000000000, 0.3281250000000000000, 0.3359375000000000000, 0.3437500000000000000, 0.3515625000000000000, 0.3593750000000000000, 0.3671875000000000000, 0.3750000000000000000, 0.3828125000000000000, 0.3906250000000000000, 0.3984375000000000000, 0.4062500000000000000, 0.4140625000000000000, 0.4218750000000000000, 0.4296875000000000000, 0.4375000000000000000, 0.4453125000000000000, 0.4531250000000000000, 0.4609375000000000000, 0.4687500000000000000, 0.4765625000000000000, 0.4843750000000000000, 0.4921875000000000000, 0.5000000000000000000, 0.5078125000000000000, 0.5156250000000000000, 0.5234375000000000000, 0.5312500000000000000, 0.5390625000000000000, 0.5468750000000000000, 0.5546875000000000000, 0.5625000000000000000, 0.5703125000000000000, 0.5781250000000000000, 0.5859375000000000000, 0.5937500000000000000, 0.6015625000000000000, 0.6093750000000000000, 0.6171875000000000000, 0.6250000000000000000, 0.6328125000000000000, 0.6406250000000000000, 0.6484375000000000000, 0.6562500000000000000, 0.6640625000000000000, 0.6718750000000000000, 0.6796875000000000000, 0.6875000000000000000, 0.6953125000000000000, 0.7031250000000000000, 0.7109375000000000000, 0.7187500000000000000, 0.7265625000000000000, 0.7343750000000000000, 0.7421875000000000000, 0.7500000000000000000, 0.7578125000000000000, 0.7656250000000000000, 0.7734375000000000000, 0.7812500000000000000, 0.7890625000000000000, 0.7968750000000000000, 0.8046875000000000000, 0.8125000000000000000, 0.8203125000000000000, 0.8281250000000000000, 0.8359375000000000000, 0.8437500000000000000, 0.8515625000000000000, 0.8593750000000000000, 0.8671875000000000000, 0.8750000000000000000, 0.8828125000000000000, 0.8906250000000000000, 0.8984375000000000000, 0.9062500000000000000, 0.9140625000000000000, 0.9218750000000000000, 0.9296875000000000000, 0.9375000000000000000, 0.9453125000000000000, 0.9531250000000000000, 0.9609375000000000000, 0.9687500000000000000, 0.9765625000000000000, 0.9843750000000000000, 0.9921875000000000000, 1.000000000000000000 ),
 .UNSPECIFIED. ) 
 GEOMETRIC_REPRESENTATION_ITEM ( )  RATIONAL_B_SPLINE_SURFACE ( (
 ( 1.000000000000000000, 0.9238795325112869605, 1.000000000000000000, 0.9238795325112869605, 1.000000000000000000, 0.9238795325112869605, 1.000000000000000000, 0.9238795325112869605, 1.000000000000000000, 0.9238795325112869605, 1.000000000000000000, 0.9238795325112869605, 1.000000000000000000, 0.9238795325112869605, 1.000000000000000000, 0.9238795325112869605, 1.000000000000000000, 0.9238795325112869605, 1.000000000000000000, 0.9238795325112869605, 1.000000000000000000, 0.9238795325112869605, 1.000000000000000000, 0.9238795325112869605, 1.000000000000000000, 0.9238795325112869605, 1.000000000000000000, 0.9238795325112869605, 1.000000000000000000, 0.9238795325112869605, 1.000000000000000000, 0.9238795325112869605, 1.000000000000000000, 0.9238795325112869605, 1.000000000000000000, 0.9238795325112869605, 1.000000000000000000, 0.9238795325112869605, 1.000000000000000000, 0.9238795325112869605, 1.000000000000000000, 0.9238795325112869605, 1.000000000000000000, 0.9238795325112869605, 1.000000000000000000, 0.9238795325112869605, 1.000000000000000000, 0.9238795325112869605, 1.000000000000000000, 0.9238795325112869605, 1.000000000000000000, 0.9238795325112869605, 1.000000000000000000, 0.9238795325112869605, 1.000000000000000000, 0.9238795325112869605, 1.000000000000000000, 0.9238795325112869605, 1.000000000000000000, 0.9238795325112869605, 1.000000000000000000, 0.9238795325112869605, 1.000000000000000000, 0.9238795325112869605, 1.000000000000000000, 0.9238795325112869605, 1.000000000000000000, 0.9238795325112869605, 1.000000000000000000, 0.9238795325112869605, 1.000000000000000000, 0.9238795325112869605, 1.000000000000000000, 0.9238795325112869605, 1.000000000000000000, 0.9238795325112869605, 1.000000000000000000, 0.9238795325112869605, 1.000000000000000000, 0.9238795325112869605, 1.000000000000000000, 0.9238795325112869605, 1.000000000000000000, 0.9238795325112869605, 1.000000000000000000, 0.9238795325112869605, 1.000000000000000000, 0.9238795325112869605, 1.000000000000000000, 0.9238795325112869605, 1.000000000000000000, 0.9238795325112869605, 1.000000000000000000, 0.9238795325112869605, 1.000000000000000000, 0.9238795325112869605, 1.000000000000000000, 0.9238795325112869605, 1.000000000000000000, 0.9238795325112869605, 1.000000000000000000, 0.9238795325112869605, 1.000000000000000000, 0.9238795325112869605, 1.000000000000000000, 0.9238795325112869605, 1.000000000000000000, 0.9238795325112869605, 1.000000000000000000, 0.9238795325112869605, 1.000000000000000000, 0.9238795325112869605, 1.000000000000000000, 0.9238795325112869605, 1.000000000000000000, 0.9238795325112869605, 1.000000000000000000, 0.9238795325112869605, 1.000000000000000000, 0.9238795325112869605, 1.000000000000000000, 0.9238795325112869605, 1.000000000000000000, 0.9238795325112869605, 1.000000000000000000, 0.9238795325112869605, 1.000000000000000000, 0.9238795325112869605, 1.000000000000000000, 0.9238795325112869605, 1.000000000000000000, 0.9238795325112869605, 1.000000000000000000, 0.9238795325112869605, 1.000000000000000000, 0.9238795325112869605, 1.000000000000000000, 0.9238795325112869605, 1.000000000000000000, 0.9238795325112869605, 1.000000000000000000, 0.9238795325112869605, 1.000000000000000000, 0.9238795325112869605, 1.000000000000000000, 0.9238795325112869605, 1.000000000000000000, 0.9238795325112869605, 1.000000000000000000, 0.9238795325112869605, 1.000000000000000000, 0.9238795325112869605, 1.000000000000000000, 0.9238795325112869605, 1.000000000000000000, 0.9238795325112869605, 1.000000000000000000, 0.9238795325112869605, 1.000000000000000000, 0.9238795325112869605, 1.000000000000000000, 0.9238795325112869605, 1.000000000000000000, 0.9238795325112869605, 1.000000000000000000, 0.9238795325112869605, 1.000000000000000000, 0.9238795325112869605, 1.000000000000000000, 0.9238795325112869605, 1.000000000000000000, 0.9238795325112869605, 1.000000000000000000, 0.9238795325112869605, 1.000000000000000000, 0.9238795325112869605, 1.000000000000000000, 0.9238795325112869605, 1.000000000000000000, 0.9238795325112869605, 1.000000000000000000, 0.9238795325112869605, 1.000000000000000000, 0.9238795325112869605, 1.000000000000000000, 0.9238795325112869605, 1.000000000000000000, 0.9238795325112869605, 1.000000000000000000, 0.9238795325112869605, 1.000000000000000000, 0.9238795325112869605, 1.000000000000000000, 0.9238795325112869605, 1.000000000000000000, 0.9238795325112869605, 1.000000000000000000, 0.9238795325112869605, 1.000000000000000000, 0.9238795325112869605, 1.000000000000000000, 0.9238795325112869605, 1.000000000000000000, 0.9238795325112869605, 1.000000000000000000, 0.9238795325112869605, 1.000000000000000000, 0.9238795325112869605, 1.000000000000000000, 0.9238795325112869605, 1.000000000000000000, 0.9238795325112869605, 1.000000000000000000, 0.9238795325112869605, 1.000000000000000000, 0.9238795325112869605, 1.000000000000000000, 0.9238795325112869605, 1.000000000000000000, 0.9238795325112869605, 1.000000000000000000, 0.9238795325112869605, 1.000000000000000000, 0.9238795325112869605, 1.000000000000000000, 0.9238795325112869605, 1.000000000000000000, 0.9238795325112869605, 1.000000000000000000, 0.9238795325112869605, 1.000000000000000000, 0.9238795325112869605, 1.000000000000000000, 0.9238795325112869605, 1.000000000000000000, 0.9238795325112869605, 1.000000000000000000, 0.9238795325112869605, 1.000000000000000000, 0.9238795325112869605, 1.000000000000000000, 0.9238795325112869605, 1.000000000000000000, 0.9238795325112869605, 1.000000000000000000, 0.9238795325112869605, 1.000000000000000000, 0.9238795325112869605, 1.000000000000000000, 0.9238795325112869605, 1.000000000000000000, 0.9238795325112869605, 1.000000000000000000, 0.9238795325112869605, 1.000000000000000000, 0.9238795325112869605, 1.000000000000000000),
 ( 1.000000000000000000, 0.9238795325112869605, 1.000000000000000000, 0.9238795325112869605, 1.000000000000000000, 0.9238795325112869605, 1.000000000000000000, 0.9238795325112869605, 1.000000000000000000, 0.9238795325112869605, 1.000000000000000000, 0.9238795325112869605, 1.000000000000000000, 0.9238795325112869605, 1.000000000000000000, 0.9238795325112869605, 1.000000000000000000, 0.9238795325112869605, 1.000000000000000000, 0.9238795325112869605, 1.000000000000000000, 0.9238795325112869605, 1.000000000000000000, 0.9238795325112869605, 1.000000000000000000, 0.9238795325112869605, 1.000000000000000000, 0.9238795325112869605, 1.000000000000000000, 0.9238795325112869605, 1.000000000000000000, 0.9238795325112869605, 1.000000000000000000, 0.9238795325112869605, 1.000000000000000000, 0.9238795325112869605, 1.000000000000000000, 0.9238795325112869605, 1.000000000000000000, 0.9238795325112869605, 1.000000000000000000, 0.9238795325112869605, 1.000000000000000000, 0.9238795325112869605, 1.000000000000000000, 0.9238795325112869605, 1.000000000000000000, 0.9238795325112869605, 1.000000000000000000, 0.9238795325112869605, 1.000000000000000000, 0.9238795325112869605, 1.000000000000000000, 0.9238795325112869605, 1.000000000000000000, 0.9238795325112869605, 1.000000000000000000, 0.9238795325112869605, 1.000000000000000000, 0.9238795325112869605, 1.000000000000000000, 0.9238795325112869605, 1.000000000000000000, 0.9238795325112869605, 1.000000000000000000, 0.9238795325112869605, 1.000000000000000000, 0.9238795325112869605, 1.000000000000000000, 0.9238795325112869605, 1.000000000000000000, 0.9238795325112869605, 1.000000000000000000, 0.9238795325112869605, 1.000000000000000000, 0.9238795325112869605, 1.000000000000000000, 0.9238795325112869605, 1.000000000000000000, 0.9238795325112869605, 1.000000000000000000, 0.9238795325112869605, 1.000000000000000000, 0.9238795325112869605, 1.000000000000000000, 0.9238795325112869605, 1.000000000000000000, 0.9238795325112869605, 1.000000000000000000, 0.9238795325112869605, 1.000000000000000000, 0.9238795325112869605, 1.000000000000000000, 0.9238795325112869605, 1.000000000000000000, 0.9238795325112869605, 1.000000000000000000, 0.9238795325112869605, 1.000000000000000000, 0.9238795325112869605, 1.000000000000000000, 0.9238795325112869605, 1.000000000000000000, 0.9238795325112869605, 1.000000000000000000, 0.9238795325112869605, 1.000000000000000000, 0.9238795325112869605, 1.000000000000000000, 0.9238795325112869605, 1.000000000000000000, 0.9238795325112869605, 1.000000000000000000, 0.9238795325112869605, 1.000000000000000000, 0.9238795325112869605, 1.000000000000000000, 0.9238795325112869605, 1.000000000000000000, 0.9238795325112869605, 1.000000000000000000, 0.9238795325112869605, 1.000000000000000000, 0.9238795325112869605, 1.000000000000000000, 0.9238795325112869605, 1.000000000000000000, 0.9238795325112869605, 1.000000000000000000, 0.9238795325112869605, 1.000000000000000000, 0.9238795325112869605, 1.000000000000000000, 0.9238795325112869605, 1.000000000000000000, 0.9238795325112869605, 1.000000000000000000, 0.9238795325112869605, 1.000000000000000000, 0.9238795325112869605, 1.000000000000000000, 0.9238795325112869605, 1.000000000000000000, 0.9238795325112869605, 1.000000000000000000, 0.9238795325112869605, 1.000000000000000000, 0.9238795325112869605, 1.000000000000000000, 0.9238795325112869605, 1.000000000000000000, 0.9238795325112869605, 1.000000000000000000, 0.9238795325112869605, 1.000000000000000000, 0.9238795325112869605, 1.000000000000000000, 0.9238795325112869605, 1.000000000000000000, 0.9238795325112869605, 1.000000000000000000, 0.9238795325112869605, 1.000000000000000000, 0.9238795325112869605, 1.000000000000000000, 0.9238795325112869605, 1.000000000000000000, 0.9238795325112869605, 1.000000000000000000, 0.9238795325112869605, 1.000000000000000000, 0.9238795325112869605, 1.000000000000000000, 0.9238795325112869605, 1.000000000000000000, 0.9238795325112869605, 1.000000000000000000, 0.9238795325112869605, 1.000000000000000000, 0.9238795325112869605, 1.000000000000000000, 0.9238795325112869605, 1.000000000000000000, 0.9238795325112869605, 1.000000000000000000, 0.9238795325112869605, 1.000000000000000000, 0.9238795325112869605, 1.000000000000000000, 0.9238795325112869605, 1.000000000000000000, 0.9238795325112869605, 1.000000000000000000, 0.9238795325112869605, 1.000000000000000000, 0.9238795325112869605, 1.000000000000000000, 0.9238795325112869605, 1.000000000000000000, 0.9238795325112869605, 1.000000000000000000, 0.9238795325112869605, 1.000000000000000000, 0.9238795325112869605, 1.000000000000000000, 0.9238795325112869605, 1.000000000000000000, 0.9238795325112869605, 1.000000000000000000, 0.9238795325112869605, 1.000000000000000000, 0.9238795325112869605, 1.000000000000000000, 0.9238795325112869605, 1.000000000000000000, 0.9238795325112869605, 1.000000000000000000, 0.9238795325112869605, 1.000000000000000000, 0.9238795325112869605, 1.000000000000000000, 0.9238795325112869605, 1.000000000000000000, 0.9238795325112869605, 1.000000000000000000, 0.9238795325112869605, 1.000000000000000000, 0.9238795325112869605, 1.000000000000000000, 0.9238795325112869605, 1.000000000000000000, 0.9238795325112869605, 1.000000000000000000, 0.9238795325112869605, 1.000000000000000000, 0.9238795325112869605, 1.000000000000000000, 0.9238795325112869605, 1.000000000000000000, 0.9238795325112869605, 1.000000000000000000, 0.9238795325112869605, 1.000000000000000000, 0.9238795325112869605, 1.000000000000000000, 0.9238795325112869605, 1.000000000000000000, 0.9238795325112869605, 1.000000000000000000, 0.9238795325112869605, 1.000000000000000000, 0.9238795325112869605, 1.000000000000000000, 0.9238795325112869605, 1.000000000000000000, 0.9238795325112869605, 1.000000000000000000) ) ) 
 REPRESENTATION_ITEM ( '' )  SURFACE ( )  );
#31623 = CARTESIAN_POINT ( 'NONE',  ( 121.7575954359119805, 0.5291689781388270175, -13.89700978578772705 ) ) ;
#31624 = ORIENTED_EDGE ( 'NONE', *, *, #1121, .F. ) ;
#31625 = CARTESIAN_POINT ( 'NONE',  ( 61.94466824697356344, -46.76115691171892053, -10.39321520033831625 ) ) ;
#31626 = CARTESIAN_POINT ( 'NONE',  ( 123.8579614775786126, 0.5811942927096110934, -14.16772938898807510 ) ) ;
#31627 = CARTESIAN_POINT ( 'NONE',  ( 112.1155414775786454, 0.9020085738987339008, -11.91225656197089222 ) ) ;
#31628 = CARTESIAN_POINT ( 'NONE',  ( 123.1772414775786189, -5.574606645277164318, -18.38911715685844683 ) ) ;
#31629 =( NAMED_UNIT ( * ) PLANE_ANGLE_UNIT ( ) SI_UNIT ( $, .RADIAN. ) );
#31630 = CARTESIAN_POINT ( 'NONE',  ( 123.9714148109119805, -0.4660016031367893996, -10.09054647747474043 ) ) ;
#31631 = CARTESIAN_POINT ( 'NONE',  ( 120.7947214775786193, -9.261995988541697145, -16.69588392320189030 ) ) ;
#31632 = CARTESIAN_POINT ( 'NONE',  ( 108.3989733795247759, -1.325403438956436419, -9.854619843455211026 ) ) ;
#31633 = CARTESIAN_POINT ( 'NONE',  ( 116.8238548109119819, -5.574606645277164318, -18.38911715685844683 ) ) ;
#31634 = DIRECTION ( 'NONE',  ( 0.07634843047859296572, 0.9970811988817437355, 0.000000000000000000 ) ) ;
#31635 = ORIENTED_EDGE ( 'NONE', *, *, #9691, .F. ) ;
#31636 = CARTESIAN_POINT ( 'NONE',  ( 120.3409081442453044, -0.4660016031367893996, -10.09054647747474043 ) ) ;
#31637 = LINE ( 'NONE', #37813, #16205 ) ;
#31638 = CARTESIAN_POINT ( 'NONE',  ( 115.2355081442453155, -10.30919188438810075, -12.61870101168855918 ) ) ;
#31639 = VERTEX_POINT ( 'NONE', #18219 ) ;
#31640 = CARTESIAN_POINT ( 'NONE',  ( 116.0388171295248014, -10.62599879583958540, -13.39321520033831447 ) ) ;
#31641 = CARTESIAN_POINT ( 'NONE',  ( 125.6732148109119862, 0.5811942927096110934, -14.16772938898807510 ) ) ;
#31642 = DIRECTION ( 'NONE',  ( 1.000000000000000000, 0.000000000000000000, -0.000000000000000000 ) ) ;
#31643 = CARTESIAN_POINT ( 'NONE',  ( 116.6536748109119941, -10.15424416112533912, -14.75197769757731336 ) ) ;
#31644 = CARTESIAN_POINT ( 'NONE',  ( 124.3999891859120055, -8.318316608003341273, -9.227040655997777563 ) ) ;
#31645 = CARTESIAN_POINT ( 'NONE',  ( 118.1852948109119836, -4.153390946401325223, -8.397313243818185668 ) ) ;
#31646 = DIRECTION ( 'NONE',  ( -0.000000000000000000, -0.9284778069183721172, -0.3713878862591650232 ) ) ;
#31647 = CARTESIAN_POINT ( 'NONE',  ( 122.2696148109119889, -5.574606645277164318, -18.38911715685844683 ) ) ;
#31648 = B_SPLINE_CURVE_WITH_KNOTS ( 'NONE', 3,
 ( #39625, #32758, #39167, #36405, #5175, #28694, #22070, #35962, #4732, #32323, #19093, #1754, #35506, #1312, #11361, #25270, #32541, #22293, #4953, #18866, #15453, #29357, #43272, #11477, #35840, #7823, #32201, #21730, #36068, #18758, #11023, #21502, #21276, #39051, #4391, #42708, #18082, #14662, #32426, #10798, #739, #24695, #11693, #28801, #3938, #29021, #4165, #25602, #39279, #7587, #42932, #35617, #38583, #21949, #31976, #35158, #7361, #14214, #28578, #17859, #31756, #8268, #39507, #42485, #22173, #14438, #28129 ),
 .UNSPECIFIED., .F., .F.,
 ( 4, 3, 3, 3, 3, 3, 3, 3, 3, 3, 3, 3, 3, 3, 3, 3, 3, 3, 3, 3, 3, 3, 4 ),
 ( 2.779028226719264772E-17, 1.132108768669561938E-05, 5.660629526298920192E-05, 0.0002378019964192440395, 0.0003283778960097989935, 0.0005095735978542089914, 0.0006001494977465600227, 0.0007813452071915360847, 0.0008719211078674949950, 0.0009624970091562879077, 0.001143692739419350157, 0.001234268642094720012, 0.001324844545703623934, 0.001506040307844935030, 0.001596616213391234725, 0.001777812005347669932, 0.001868387913206439720, 0.001958963822483724988, 0.002140159663056734936, 0.002230735575091844988, 0.002321311488774285316, 0.002474333065496200044, 0.002627496479460559795 ),
 .UNSPECIFIED. ) ;
#31649 = CIRCLE ( 'NONE', #26594, 0.5000000000000004441 ) ;
#31650 = DIRECTION ( 'NONE',  ( 0.000000000000000000, 0.3818493186865927203, -0.9242245927363029745 ) ) ;
#31651 = CARTESIAN_POINT ( 'NONE',  ( 119.7169148109119874, -0.1624402480850797581, -16.17319339645315424 ) ) ;
#31652 = CARTESIAN_POINT ( 'NONE',  ( 122.1048610609119720, -3.163656168406935087, -18.89861972220014508 ) ) ;
#31653 = CARTESIAN_POINT ( 'NONE',  ( 114.5547881442453217, -5.638512984488999180, -18.83840828888717311 ) ) ;
#31654 = DIRECTION ( 'NONE',  ( 0.9908103287288502203, -0.1352586133457969741, 0.000000000000000000 ) ) ;
#31655 = CARTESIAN_POINT ( 'NONE',  ( 120.5678148109119832, -1.833838273342659253, -17.42832698103878286 ) ) ;
#31656 = ORIENTED_EDGE ( 'NONE', *, *, #25043, .T. ) ;
#31657 = CARTESIAN_POINT ( 'NONE',  ( 117.5045748109119756, 0.5811942927096110934, -14.16772938898807510 ) ) ;
#31658 = CARTESIAN_POINT ( 'NONE',  ( 114.3719421295247827, -9.868328341294093420, -13.39321520033831447 ) ) ;
#31659 = LINE ( 'NONE', #28485, #7358 ) ;
#31660 = CARTESIAN_POINT ( 'NONE',  ( 121.9470836909669913, -25.99489077589524300, -13.39321520033831447 ) ) ;
#31661 = CARTESIAN_POINT ( 'NONE',  ( 121.8270485609119760, -0.08252387247370714107, -11.91645802438286950 ) ) ;
#31662 = CARTESIAN_POINT ( 'NONE',  ( 122.3830681442452857, -8.166667518702819706, -8.995218007635861213 ) ) ;
#31663 = VERTEX_POINT ( 'NONE', #25292 ) ;
#31664 = CARTESIAN_POINT ( 'NONE',  ( 118.6591994150595895, -2.423081321603731908, -17.89265170041263175 ) ) ;
#31665 = CARTESIAN_POINT ( 'NONE',  ( 120.7947214775786193, -0.8288870151387760510, -10.36305467784173118 ) ) ;
#31666 = DIRECTION ( 'NONE',  ( -0.2768435750659253847, -0.3568721902840677473, 0.8921882507333133150 ) ) ;
#31667 = CARTESIAN_POINT ( 'NONE',  ( 60.96715249881023624, -14.49348130257909162, -18.08530754977647703 ) ) ;
#31668 = CARTESIAN_POINT ( 'NONE',  ( 70.19189222814998175, -49.76310523276723785, -29.87698278062876511 ) ) ;
#31669 = CARTESIAN_POINT ( 'NONE',  ( 113.8163171295247764, 0.1403307496149613920, -13.39321520033831447 ) ) ;
#31670 = DIRECTION ( 'NONE',  ( -0.9498278979187092519, -0.3127730236694430399, 0.000000000000000000 ) ) ;
#31671 = EDGE_LOOP ( 'NONE', ( #9110, #36070, #31989, #19392, #42712 ) ) ;
#31672 = CARTESIAN_POINT ( 'NONE',  ( 114.0442481442453300, -1.834011780172310813, -8.268836392978581529 ) ) ;
#31673 = CARTESIAN_POINT ( 'NONE',  ( 125.9568481442452850, -3.505236298600246325, -18.68346056562440793 ) ) ;
#31674 = CARTESIAN_POINT ( 'NONE',  ( 121.7023481442452777, -9.261995988541697145, -16.69588392320189030 ) ) ;
#31675 = CARTESIAN_POINT ( 'NONE',  ( 116.3700414775786527, -4.153390946401321671, -8.397313243818183892 ) ) ;
#31676 = DIRECTION ( 'NONE',  ( 1.000000000000000000, 0.000000000000000000, -0.000000000000000000 ) ) ;
#31677 =( LENGTH_UNIT ( ) NAMED_UNIT ( * ) SI_UNIT ( .MILLI., .METRE. ) );
#31678 = CARTESIAN_POINT ( 'NONE',  ( 121.4754414775786131, -8.166667518702819706, -8.995218007635861213 ) ) ;
#31679 = CARTESIAN_POINT ( 'NONE',  ( 123.4608748109119745, 0.4262465694468626776, -12.03445270309935111 ) ) ;
#31680 = LINE ( 'NONE', #7289, #18653 ) ;
#31681 = DIRECTION ( 'NONE',  ( 0.000000000000000000, -0.3818493186865927203, 0.9242245927363029745 ) ) ;
#31682 = CARTESIAN_POINT ( 'NONE',  ( 124.2550481442452792, -0.1624402480850797581, -16.17319339645315424 ) ) ;
#31683 = ORIENTED_EDGE ( 'NONE', *, *, #11469, .F. ) ;
#31684 = EDGE_CURVE ( 'NONE', #38775, #16972, #882, .T. ) ;
#31685 = VECTOR ( 'NONE', #39565, 1000.000000000000000 ) ;
#31686 = CYLINDRICAL_SURFACE ( 'NONE', #40177, 3.000000000000001776 ) ;
#31687 = CARTESIAN_POINT ( 'NONE',  ( 119.2631014775786298, 0.2603800115204892296, -16.42320221600525088 ) ) ;
#31688 = CARTESIAN_POINT ( 'NONE',  ( 124.4819548109119722, -2.084020599724406786, -8.691656652584148546 ) ) ;
#31689 = VERTEX_POINT ( 'NONE', #28714 ) ;
#31690 = CARTESIAN_POINT ( 'NONE',  ( 136.1673833308536530, 0.5777653812705602077, -11.18378269846704853 ) ) ;
#31691 = CARTESIAN_POINT ( 'NONE',  ( 120.9081748109119872, -5.638512984488999180, -18.83840828888717311 ) ) ;
#31692 = AXIS2_PLACEMENT_3D ( 'NONE', #4377, #25808, #28790 ) ;
#31693 = CARTESIAN_POINT ( 'NONE',  ( 107.7738952545248310, 0.8980012041604421569, -11.00651665394454071 ) ) ;
#31694 = CARTESIAN_POINT ( 'NONE',  ( 119.5467348109119712, -5.574606645277164318, -18.38911715685844683 ) ) ;
#31695 = ORIENTED_EDGE ( 'NONE', *, *, #37297, .F. ) ;
#31696 = CARTESIAN_POINT ( 'NONE',  ( 113.9307948109119906, 0.9020085738987339008, -11.91225656197089222 ) ) ;
#31697 = DIRECTION ( 'NONE',  ( 0.000000000000000000, -0.4669533266896290225, -0.8842819633428516957 ) ) ;
#31698 = CARTESIAN_POINT ( 'NONE',  ( 112.7547603923315762, -1.063912429576153063, -17.20460841810474761 ) ) ;
#31699 = DIRECTION ( 'NONE',  ( 0.000000000000000000, 0.000000000000000000, -1.000000000000000000 ) ) ;
#31700 = CARTESIAN_POINT ( 'NONE',  ( 124.5954081442453116, -3.383040157471821630, -19.15922257007629170 ) ) ;
#31701 = EDGE_CURVE ( 'NONE', #25838, #31560, #27825, .T. ) ;
#31702 = FACE_OUTER_BOUND ( 'NONE', #30690, .T. ) ;
#31703 = CARTESIAN_POINT ( 'NONE',  ( 71.31713442278437753, 2.423123680056944007, -15.89321520033831447 ) ) ;
#31704 = CARTESIAN_POINT ( 'NONE',  ( 123.0070614775786169, 0.9020085738987339008, -11.91225656197089222 ) ) ;
#31706 = CARTESIAN_POINT ( 'NONE',  ( 123.4041481442452834, 0.1319031606808879209, -14.10382304977623669 ) ) ;
#31705 = CARTESIAN_POINT ( 'NONE',  ( 123.5176014775786228, -9.261995988541697145, -16.69588392320189030 ) ) ;
#31707 = CARTESIAN_POINT ( 'NONE',  ( 119.9438214775786378, -2.084020599724406786, -8.691656652584148546 ) ) ;
#31708 = CARTESIAN_POINT ( 'NONE',  ( 70.98136983621358809, -24.64626890834123785, -5.214987668974215396 ) ) ;
#31709 = CARTESIAN_POINT ( 'NONE',  ( 115.5758681442453053, -1.561330072975668060, -17.79121239304076951 ) ) ;
#31710 = ADVANCED_FACE ( 'NONE', ( #30605 ), #16255, .T. ) ;
#31711 = ORIENTED_EDGE ( 'NONE', *, *, #42676, .F. ) ;
#31712 = CARTESIAN_POINT ( 'NONE',  ( 112.7050671295247923, -10.62599879583958540, -13.39321520033831980 ) ) ;
#31713 = EDGE_CURVE ( 'NONE', #36520, #39978, #16483, .T. ) ;
#31714 = CARTESIAN_POINT ( 'NONE',  ( 125.1521348109119742, -1.861572684144302992, -17.39139446643087084 ) ) ;
#31715 = CARTESIAN_POINT ( 'NONE',  ( 114.0941296295247867, -4.863998795839590272, -8.388885654883775800 ) ) ;
#31716 = CARTESIAN_POINT ( 'NONE',  ( 107.2182702545248105, 0.1403307496149616695, -11.32035403202665336 ) ) ;
#31717 = CARTESIAN_POINT ( 'NONE',  ( 114.8581140045248361, 0.1403307496149616695, -15.46607636864997204 ) ) ;
#31718 = CARTESIAN_POINT ( 'NONE',  ( 125.7299414775786346, 0.9020085738987339008, -11.91225656197089222 ) ) ;
#31719 = CARTESIAN_POINT ( 'NONE',  ( 112.6828081442453282, -7.893985811506177619, -18.51759400769804742 ) ) ;
#31720 = ORIENTED_EDGE ( 'NONE', *, *, #43308, .F. ) ;
#31721 = CARTESIAN_POINT ( 'NONE',  ( 114.4413348109119823, -0.8288870151387760510, -10.36305467784173118 ) ) ;
#31722 = CARTESIAN_POINT ( 'NONE',  ( 111.8716296295247901, -4.863998795839590272, -19.15521520033831493 ) ) ;
#31723 = CARTESIAN_POINT ( 'NONE',  ( 125.2194014775786286, -10.30919188438810075, -12.61870101168855918 ) ) ;
#31724 = CARTESIAN_POINT ( 'NONE',  ( 125.9001214775786224, -4.089484607189486809, -7.948022111789456723 ) ) ;
#31726 = AXIS2_PLACEMENT_3D ( 'NONE', #9680, #17418, #31309 ) ;
#31725 = DIRECTION ( 'NONE',  ( 0.8636456077245088236, -0.5040994586965589219, 0.000000000000000000 ) ) ;
#31727 = CARTESIAN_POINT ( 'NONE',  ( 115.4624148109119943, -5.638512984488999180, -18.83840828888717311 ) ) ;
#31728 = ADVANCED_FACE ( 'NONE', ( #40648 ), #26355, .F. ) ;
#31729 = CARTESIAN_POINT ( 'NONE',  ( 116.1777233795247781, -8.938348069036489818, -17.46756447353520159 ) ) ;
#31730 = CARTESIAN_POINT ( 'NONE',  ( 112.0105358795248804, -8.402594152722688392, -9.854619843455216355 ) ) ;
#31731 = ORIENTED_EDGE ( 'NONE', *, *, #17584, .T. ) ;
#31732 = DIRECTION ( 'NONE',  ( 0.8949343913984424415, 0.4123869368673875324, 0.1703803081152070742 ) ) ;
#31733 = CARTESIAN_POINT ( 'NONE',  ( 114.1009748109119784, -5.574606645277164318, -18.38911715685844683 ) ) ;
#31734 = CARTESIAN_POINT ( 'NONE',  ( 111.8886348109120092, -3.383040157471821630, -19.15922257007629170 ) ) ;
#31735 = CIRCLE ( 'NONE', #23014, 2.445500000000004448 ) ;
#31736 = CARTESIAN_POINT ( 'NONE',  ( 115.8304577545247582, -7.250697342233347165, -7.631215200338321125 ) ) ;
#31737 = CYLINDRICAL_SURFACE ( 'NONE', #810, 5.000000000000000888 ) ;
#31738 = EDGE_CURVE ( 'NONE', #17999, #34005, #35076, .T. ) ;
#31739 = CARTESIAN_POINT ( 'NONE',  ( 124.1415948109119540, -3.505236298600246325, -18.68346056562440793 ) ) ;
#31740 = CARTESIAN_POINT ( 'NONE',  ( 120.0005481442453146, -4.153390946401325223, -8.397313243818185668 ) ) ;
#31741 = CARTESIAN_POINT ( 'NONE',  ( 111.2646414775786496, -8.899110576539710493, -16.42337572283490132 ) ) ;
#31742 = VERTEX_POINT ( 'NONE', #28030 ) ;
#31743 = ADVANCED_FACE ( 'NONE', ( #44305 ), #30158, .T. ) ;
#31744 = EDGE_CURVE ( 'NONE', #27865, #9168, #44076, .T. ) ;
#31745 = CARTESIAN_POINT ( 'NONE',  ( 125.2194014775786286, 0.1319031606808879209, -14.10382304977623669 ) ) ;
#31746 = CIRCLE ( 'NONE', #35374, 6.426280380454326924 ) ;
#31747 = FACE_OUTER_BOUND ( 'NONE', #8941, .T. ) ;
#31748 = CARTESIAN_POINT ( 'NONE',  ( 112.3424481442453384, -3.505236298600246325, -18.68346056562440793 ) ) ;
#31749 = EDGE_LOOP ( 'NONE', ( #37764, #5826, #42693, #44964 ) ) ;
#31750 = CARTESIAN_POINT ( 'NONE',  ( 126.2333338125929458, -8.954712395367375066, -16.28134568519805470 ) ) ;
#31751 = DIRECTION ( 'NONE',  ( 0.2588190451025191297, -0.9659258262890686453, 0.000000000000000000 ) ) ;
#31752 = CARTESIAN_POINT ( 'NONE',  ( 109.5796765045248122, -2.791137627527939813, -8.388885654883777576 ) ) ;
#31753 = ORIENTED_EDGE ( 'NONE', *, *, #26771, .F. ) ;
#31754 = CARTESIAN_POINT ( 'NONE',  ( 117.3911214775786505, -7.894159318335828068, -9.358103419637847864 ) ) ;
#31755 = CARTESIAN_POINT ( 'NONE',  ( 112.8529881442453160, -7.894159318335828068, -9.358103419637847864 ) ) ;
#31756 = CARTESIAN_POINT ( 'NONE',  ( 124.5867640960332068, -9.779101121451267531, -14.32922897161243903 ) ) ;
#31757 = VECTOR ( 'NONE', #14893, 1000.000000000000114 ) ;
#31758 = CARTESIAN_POINT ( 'NONE',  ( 122.1743141859119817, -0.8832429491016019485, -18.19431474523657855 ) ) ;
#31759 = ORIENTED_EDGE ( 'NONE', *, *, #35709, .T. ) ;
#31760 = FACE_OUTER_BOUND ( 'NONE', #38369, .T. ) ;
#31761 = CARTESIAN_POINT ( 'NONE',  ( 119.7434548109119845, -2.551128697860804095, -8.956764161815621961 ) ) ;
#31762 = CARTESIAN_POINT ( 'NONE',  ( 112.6356140045247827, -10.62599879583958717, -11.00651665394454604 ) ) ;
#31763 = CARTESIAN_POINT ( 'NONE',  ( 127.7425183523501744, 0.8652765085452543969, -12.77968882490997338 ) ) ;
#31764 = CARTESIAN_POINT ( 'NONE',  ( 113.1366214775786432, -1.834011780172310813, -8.268836392978581529 ) ) ;
#31765 = CARTESIAN_POINT ( 'NONE',  ( 118.1285681442453068, -2.084020599724406786, -8.691656652584148546 ) ) ;
#31766 = PLANE ( 'NONE',  #24315 ) ;
#31767 = ORIENTED_EDGE ( 'NONE', *, *, #19432, .T. ) ;
#31768 = CARTESIAN_POINT ( 'NONE',  ( 115.5191414775786569, -6.222761293078241884, -8.102969835052219238 ) ) ;
#31769 = CARTESIAN_POINT ( 'NONE',  ( 115.8304577545247582, -7.250697342233347165, -7.631215200338321125 ) ) ;
#31770 = CARTESIAN_POINT ( 'NONE',  ( 84.86020291624818412, -29.99489077589588959, -11.86952202423883485 ) ) ;
#31771 = CARTESIAN_POINT ( 'NONE',  ( 114.8581140045248361, -10.62599879583958717, -11.00651665394454604 ) ) ;
#31772 = CIRCLE ( 'NONE', #17954, 2.000000000000000444 ) ;
#31773 = CARTESIAN_POINT ( 'NONE',  ( 116.3700414775786527, -5.638512984488999180, -18.83840828888717311 ) ) ;
#31774 = VERTEX_POINT ( 'NONE', #34017 ) ;
#31775 = CARTESIAN_POINT ( 'NONE',  ( 118.1285681442453068, -7.893985811506177619, -18.51759400769804742 ) ) ;
#31776 = DIRECTION ( 'NONE',  ( 0.000000000000000000, 0.000000000000000000, -1.000000000000000000 ) ) ;
#31777 = CARTESIAN_POINT ( 'NONE',  ( 113.4690515045247992, -2.477300249445798297, -7.631215200338321125 ) ) ;
#31778 = CARTESIAN_POINT ( 'NONE',  ( 114.3846081442453197, -10.63000616557722466, -14.87417383870573495 ) ) ;
#31779 = CARTESIAN_POINT ( 'NONE',  ( 114.3846081442453197, -10.63000616557722466, -14.87417383870573495 ) ) ;
#31780 = DIRECTION ( 'NONE',  ( 0.000000000000000000, -0.3818493186865936084, 0.9242245927363024194 ) ) ;
#31781 = FACE_OUTER_BOUND ( 'NONE', #37263, .T. ) ;
#31782 = CARTESIAN_POINT ( 'NONE',  ( 110.4825671295247815, 0.1403307496149613920, -13.39321520033831447 ) ) ;
#31783 = ADVANCED_FACE ( 'NONE', ( #12613 ), #26516, .T. ) ;
#31784 = VERTEX_POINT ( 'NONE', #38269 ) ;
#31785 = LINE ( 'NONE', #18112, #20852 ) ;
#31786 = CARTESIAN_POINT ( 'NONE',  ( 109.2294363213805610, -4.465500680915763354, -18.55270374900329600 ) ) ;
#31787 = CARTESIAN_POINT ( 'NONE',  ( 115.8595014775786609, -7.643976991954077427, -18.09477374809248928 ) ) ;
#31788 = CARTESIAN_POINT ( 'NONE',  ( 65.01991922978720595, -13.34372148804275149, -11.74794487108197849 ) ) ;
#31789 = CARTESIAN_POINT ( 'NONE',  ( 122.7777921015961198, -1.040089454026960292, -17.23633227186633476 ) ) ;
#31790 = CARTESIAN_POINT ( 'NONE',  ( 107.9128015045248219, -2.477300249445798297, -7.631215200338321125 ) ) ;
#31791 = CARTESIAN_POINT ( 'NONE',  ( 126.3243314201107097, -4.538965831925366956, -8.350727740338225402 ) ) ;
#31792 = CARTESIAN_POINT ( 'NONE',  ( 111.2646414775786496, -8.899110576539710493, -16.42337572283490132 ) ) ;
#31793 = LINE ( 'NONE', #21315, #19708 ) ;
#31794 = CARTESIAN_POINT ( 'NONE',  ( 124.3117748109119844, -10.30919188438810075, -12.61870101168855918 ) ) ;
#31795 = CARTESIAN_POINT ( 'NONE',  ( 116.9373081442452929, -8.166667518702817929, -8.995218007635861213 ) ) ;
#31796 = ORIENTED_EDGE ( 'NONE', *, *, #23804, .F. ) ;
#31797 = AXIS2_PLACEMENT_3D ( 'NONE', #20950, #25037, #28019 ) ;
#31798 = CARTESIAN_POINT ( 'NONE',  ( 116.4834948109119779, -7.894159318335828068, -9.358103419637847864 ) ) ;
#31799 = DIRECTION ( 'NONE',  ( -1.000000000000000000, 0.000000000000000000, 0.000000000000000000 ) ) ;
#31800 = CARTESIAN_POINT ( 'NONE',  ( 118.8092881442453290, -9.988377603198976828, -10.36322818467138340 ) ) ;
#31801 = CARTESIAN_POINT ( 'NONE',  ( 117.5045748109119756, -9.859900752359374465, -12.68260735090039404 ) ) ;
#31802 = EDGE_LOOP ( 'NONE', ( #23409, #12973, #24656, #34182, #19781 ) ) ;
#31803 = EDGE_CURVE ( 'NONE', #28126, #39007, #41761, .T. ) ;
#31804 = CARTESIAN_POINT ( 'NONE',  ( 121.2485348109119769, -8.899110576539710493, -16.42337572283490132 ) ) ;
#31805 = CARTESIAN_POINT ( 'NONE',  ( 118.3554748109119998, 0.2603800115204892296, -16.42320221600525088 ) ) ;
#31806 = CARTESIAN_POINT ( 'NONE',  ( 136.7878215370441524, 0.3576572923493759881, -15.41906115585400272 ) ) ;
#31807 = CARTESIAN_POINT ( 'NONE',  ( 109.3713171295247832, -10.62599879583958540, -13.39321520033831447 ) ) ;
#31808 = CARTESIAN_POINT ( 'NONE',  ( 62.16677121968579200, -14.49431128105087829, -9.102658187437317139 ) ) ;
#31809 = CARTESIAN_POINT ( 'NONE',  ( 86.48169505875749508, -25.99489077589524300, -13.39321520033831625 ) ) ;
#31810 = AXIS2_PLACEMENT_3D ( 'NONE', #16275, #43862, #37220 ) ;
#31811 = DIRECTION ( 'NONE',  ( 6.830048575890719297E-16, 0.5905882410490338463, 0.8069730661766898461 ) ) ;
#31812 = CARTESIAN_POINT ( 'NONE',  ( 115.4624148109119943, -5.638512984488999180, -18.83840828888717311 ) ) ;
#31813 = LINE ( 'NONE', #21560, #25869 ) ;
#31814 = CARTESIAN_POINT ( 'NONE',  ( 113.9875214775786532, -8.899110576539710493, -16.42337572283490132 ) ) ;
#31815 = CARTESIAN_POINT ( 'NONE',  ( 111.1729021944299944, 0.6269505268395592079, -12.14321520033830026 ) ) ;
#31816 = CARTESIAN_POINT ( 'NONE',  ( 112.2358197905468984, 0.6938714319018670640, -12.14321520033833579 ) ) ;
#31817 = CARTESIAN_POINT ( 'NONE',  ( 116.1777233795247781, -1.325403438956436419, -9.854619843455211026 ) ) ;
#31818 = CIRCLE ( 'NONE', #9283, 2.000000000000000444 ) ;
#31819 = CARTESIAN_POINT ( 'NONE',  ( -1.307700928565892706, -16.07486664983353819, -19.39321520033831447 ) ) ;
#31820 = DIRECTION ( 'NONE',  ( 0.6049664196031392382, -0.7962509850245451659, 0.000000000000000000 ) ) ;
#31821 = CARTESIAN_POINT ( 'NONE',  ( 111.4705635773848940, -2.467220198592768199, -17.83387418641523325 ) ) ;
#31823 = CARTESIAN_POINT ( 'NONE',  ( 117.4478481442453131, 0.2603800115204892296, -16.42320221600525088 ) ) ;
#31822 = CARTESIAN_POINT ( 'NONE',  ( 116.0086969107182142, -2.467220198592777525, -17.83387418641524391 ) ) ;
#31824 = B_SPLINE_CURVE_WITH_KNOTS ( 'NONE', 3,
 ( #9240, #29533, #43449, #26111, #40017, #22686, #26341, #19719, #15858, #1706, #40704, #29982, #37256, #8782, #6029, #22914, #29754, #19951, #36806, #36585, #16078, #43900, #5800, #5360, #5575, #40480, #26567, #19498, #23375, #19277, #30437, #12898, #33604, #13117, #33377, #2148, #23149 ),
 .UNSPECIFIED., .F., .F.,
 ( 4, 1, 1, 1, 1, 2, 2, 1, 1, 1, 1, 2, 2, 1, 1, 1, 2, 2, 1, 1, 2, 2, 2, 2, 4 ),
 ( 0.000000000000000000, 0.1250000000000005274, 0.1875000000000007772, 0.2187499999999955314, 0.2343749999999929223, 0.2421874999999915901, 0.2499999999999902855, 0.3749999999999692468, 0.4374999999999587552, 0.4687499999999535372, 0.4843749999999566458, 0.4921874999999523714, 0.4999999999999481526, 0.5624999999999441558, 0.5937499999999422684, 0.6093749999999412692, 0.6171874999999459321, 0.6249999999999507061, 0.6874999999999606981, 0.7187499999999656941, 0.7343749999999725775, 0.7499999999999793499, 0.8124999999999845679, 0.8749999999999896749, 1.000000000000000000 ),
 .UNSPECIFIED. ) ;
#31825 = CARTESIAN_POINT ( 'NONE',  ( 125.7866681442452688, -8.899110576539710493, -16.42337572283490132 ) ) ;
#31826 = CARTESIAN_POINT ( 'NONE',  ( 120.5110881442453206, -3.505236298600246325, -18.68346056562440793 ) ) ;
#31827 = CARTESIAN_POINT ( 'NONE',  ( 112.6828081442453282, -2.084020599724406786, -8.691656652584148546 ) ) ;
#31828 = ORIENTED_EDGE ( 'NONE', *, *, #38036, .T. ) ;
#31829 = CARTESIAN_POINT ( 'NONE',  ( 73.47343079648352671, -1.934511955536642791, -14.64321520033831447 ) ) ;
#31830 = CARTESIAN_POINT ( 'NONE',  ( 122.3263414775786373, -6.344957434206665248, -7.627207830600338134 ) ) ;
#31831 = CARTESIAN_POINT ( 'NONE',  ( 115.8999108795247821, -1.325403438956436419, -16.93181055722141792 ) ) ;
#31832 = CARTESIAN_POINT ( 'NONE',  ( 117.7314814775786260, -5.574606645277164318, -18.38911715685844683 ) ) ;
#31833 = EDGE_CURVE ( 'NONE', #23032, #18337, #13278, .T. ) ;
#31834 = CARTESIAN_POINT ( 'NONE',  ( 111.6050014775786536, 0.1319031606808879209, -14.10382304977623669 ) ) ;
#31835 = CARTESIAN_POINT ( 'NONE',  ( 93.24708369096698846, -25.99489077589524300, -13.39321520033831447 ) ) ;
#31836 = CARTESIAN_POINT ( 'NONE',  ( 111.0381921295247878, 0.8980012041604618078, -13.39321520033831447 ) ) ;
#31837 = CARTESIAN_POINT ( 'NONE',  ( 120.2274548109119934, -9.859900752359374465, -12.68260735090039404 ) ) ;
#31838 = CARTESIAN_POINT ( 'NONE',  ( 123.2906948109119867, -1.833838273342659697, -17.42832698103878286 ) ) ;
#31839 = CARTESIAN_POINT ( 'NONE',  ( 114.3846081442453197, 0.4262465694468551280, -12.03445270309932269 ) ) ;
#31840 = CARTESIAN_POINT ( 'NONE',  ( 109.2295198960366776, -5.481997562533197588, -7.823790098599812559 ) ) ;
#31841 = CARTESIAN_POINT ( 'NONE',  ( 87.41631446019775353, -25.99489077589524300, -13.39321520033831625 ) ) ;
#31842 = CARTESIAN_POINT ( 'NONE',  ( 116.5249890045247980, 0.8980012041604421569, -15.77991374673208469 ) ) ;
#31843 = DIRECTION ( 'NONE',  ( 1.000000000000000000, 0.000000000000000000, -0.000000000000000000 ) ) ;
#31844 = CARTESIAN_POINT ( 'NONE',  ( 119.2063748109119814, -1.561330072975668504, -17.79121239304076951 ) ) ;
#31845 = CARTESIAN_POINT ( 'NONE',  ( 115.8595014775786609, -1.834011780172310813, -8.268836392978581529 ) ) ;
#31846 = CARTESIAN_POINT ( 'NONE',  ( 111.5938171295247940, -10.62599879583958540, -13.39321520033831447 ) ) ;
#31847 = CARTESIAN_POINT ( 'NONE',  ( 114.7249681442453237, 0.2603800115204892296, -16.42320221600525088 ) ) ;
#31848 = ORIENTED_EDGE ( 'NONE', *, *, #39322, .T. ) ;
#31849 = FACE_OUTER_BOUND ( 'NONE', #16162, .T. ) ;
#31850 = CARTESIAN_POINT ( 'NONE',  ( 124.0281414775786146, -1.834011780172310813, -8.268836392978581529 ) ) ;
#31851 = CARTESIAN_POINT ( 'NONE',  ( 116.7104014775786425, -0.4660016031367893996, -10.09054647747474043 ) ) ;
#31852 = EDGE_CURVE ( 'NONE', #2648, #29655, #32015, .T. ) ;
#31853 = CARTESIAN_POINT ( 'NONE',  ( 122.3830681442452857, -1.833838273342659697, -17.42832698103878286 ) ) ;
#31854 = CARTESIAN_POINT ( 'NONE',  ( 124.5954081442453116, -3.383040157471821630, -19.15922257007629170 ) ) ;
#31855 = CARTESIAN_POINT ( 'NONE',  ( 120.5110881442453206, -6.344957434206665248, -7.627207830600338134 ) ) ;
#31856 = CIRCLE ( 'NONE', #2010, 2.200000000000001066 ) ;
#31857 = CARTESIAN_POINT ( 'NONE',  ( 113.1912390045248031, 0.8980012041604421569, -15.77991374673208469 ) ) ;
#31858 = CARTESIAN_POINT ( 'NONE',  ( 115.6325948109119821, -9.565557343593413364, -10.61323700422348004 ) ) ;
#31859 = LINE ( 'NONE', #28456, #44691 ) ;
#31860 = ORIENTED_EDGE ( 'NONE', *, *, #10799, .F. ) ;
#31861 = B_SPLINE_CURVE_WITH_KNOTS ( 'NONE', 3,
 ( #944, #15084, #11664, #39021, #4584, #42455, #15303, #14633, #712, #7561, #42009, #14863, #21920, #24669, #28772, #11448 ),
 .UNSPECIFIED., .F., .F.,
 ( 4, 2, 2, 2, 2, 2, 2, 4 ),
 ( 1.734723475976806902E-18, 0.0009594866571110036938, 0.001918973314222005653, 0.002878459971333007829, 0.003837946628444009571, 0.004797433285555011313, 0.005756919942666013923, 0.007675893256888017407 ),
 .UNSPECIFIED. ) ;
#31862 = CARTESIAN_POINT ( 'NONE',  ( 120.3976348109119812, -1.834011780172310813, -8.268836392978581529 ) ) ;
#31863 = CARTESIAN_POINT ( 'NONE',  ( 119.9518141859119851, -8.321307733199551748, -9.223433127585318303 ) ) ;
#31864 = CARTESIAN_POINT ( 'NONE',  ( 120.9081748109119872, -5.638512984488999180, -18.83840828888717311 ) ) ;
#31865 = ORIENTED_EDGE ( 'NONE', *, *, #5509, .F. ) ;
#31866 = CARTESIAN_POINT ( 'NONE',  ( 116.5249890045247980, 0.8980012041604421569, -15.77991374673208469 ) ) ;
#31867 = CARTESIAN_POINT ( 'NONE',  ( 124.0281414775786146, -1.834011780172310813, -8.268836392978581529 ) ) ;
#31868 = EDGE_CURVE ( 'NONE', #8341, #33992, #42404, .T. ) ;
#31870 = CARTESIAN_POINT ( 'NONE',  ( 122.0994348109119585, 0.9020085738987414503, -11.91225656197092242 ) ) ;
#31869 = CONICAL_SURFACE ( 'NONE', #12232, 1.610000000000000986, 0.9599310885968765916 ) ;
#31871 = CARTESIAN_POINT ( 'NONE',  ( 116.5969481442453031, -9.859900752359374465, -12.68260735090039404 ) ) ;
#31872 = CARTESIAN_POINT ( 'NONE',  ( 135.3184548109119874, -5.622599431619523358, -7.441364641445410655 ) ) ;
#31873 = CARTESIAN_POINT ( 'NONE',  ( 119.3198281442452924, -9.859900752359374465, -12.68260735090039404 ) ) ;
#31874 = DIRECTION ( 'NONE',  ( 0.000000000000000000, 0.9284778069183720062, 0.3713878862591650232 ) ) ;
#31875 = CARTESIAN_POINT ( 'NONE',  ( 119.7169148109119874, -0.1624402480850797581, -16.17319339645315424 ) ) ;
#31876 = CARTESIAN_POINT ( 'NONE',  ( 125.3566265649659073, -10.97543583693571989, -9.883038420138618108 ) ) ;
#31877 = CARTESIAN_POINT ( 'NONE',  ( 118.9227414775786542, 0.4262465694468514643, -12.03445270309931736 ) ) ;
#31878 = CARTESIAN_POINT ( 'NONE',  ( 112.8529881442453302, -1.561330072975668060, -17.79121239304076596 ) ) ;
#31879 = CARTESIAN_POINT ( 'NONE',  ( 118.3554748109119998, 0.2603800115204892296, -16.42320221600525088 ) ) ;
#31880 = CARTESIAN_POINT ( 'NONE',  ( 112.2857214775786474, -4.089484607189486809, -7.948022111789456723 ) ) ;
#31881 = DIRECTION ( 'NONE',  ( -1.000000000000000000, 0.000000000000000000, 0.000000000000000000 ) ) ;
#31882 = CARTESIAN_POINT ( 'NONE',  ( 118.9227414775786542, 0.4262465694468514643, -12.03445270309931736 ) ) ;
#31883 = ORIENTED_EDGE ( 'NONE', *, *, #20391, .F. ) ;
#31884 = CARTESIAN_POINT ( 'NONE',  ( 117.0507614775786465, -10.30919188438810075, -12.61870101168855918 ) ) ;
#31885 = CARTESIAN_POINT ( 'NONE',  ( 115.5526452545247622, -9.868328341294098749, -15.46607636864997204 ) ) ;
#31886 = CARTESIAN_POINT ( 'NONE',  ( 115.4624148109119943, -4.153390946401313677, -8.397313243818183892 ) ) ;
#31887 = DIRECTION ( 'NONE',  ( 0.000000000000000000, 0.6004852223388239540, -0.7996358532186341739 ) ) ;
#31888 = CARTESIAN_POINT ( 'NONE',  ( 122.0354079359119908, -4.360204210389830415, -8.000047426360247016 ) ) ;
#31889 = CARTESIAN_POINT ( 'NONE',  ( 121.4187148109119789, -6.344957434206665248, -7.627207830600338134 ) ) ;
#31890 = ORIENTED_EDGE ( 'NONE', *, *, #25861, .T. ) ;
#31891 = CARTESIAN_POINT ( 'NONE',  ( 66.06194382436763135, -14.97931106434683635, -4.893215200338314474 ) ) ;
#31892 = CARTESIAN_POINT ( 'NONE',  ( 120.2274548109119934, -9.859900752359374465, -12.68260735090039404 ) ) ;
#31893 = CARTESIAN_POINT ( 'NONE',  ( 120.3685329359119862, -4.283928203966213211, -7.183505701512925334 ) ) ;
#31894 = CARTESIAN_POINT ( 'NONE',  ( 63.51875845105345064, -14.83467802062719798, -16.85055330987278666 ) ) ;
#31895 = CARTESIAN_POINT ( 'NONE',  ( 76.19189222814999596, -49.76310523276725206, -36.33917278160905084 ) ) ;
#31896 = CARTESIAN_POINT ( 'NONE',  ( 112.9828796295247884, -4.863998795839590272, -8.388885654883775800 ) ) ;
#31897 = ORIENTED_EDGE ( 'NONE', *, *, #35709, .F. ) ;
#31898 = CARTESIAN_POINT ( 'NONE',  ( 114.1009748109119784, -4.089484607189486809, -7.948022111789456723 ) ) ;
#31899 = CARTESIAN_POINT ( 'NONE',  ( 124.7088614775786226, -9.565557343593413364, -10.61323700422348004 ) ) ;
#31900 = CARTESIAN_POINT ( 'NONE',  ( 70.19189222814998175, -52.97765562947117957, -34.39388673445118627 ) ) ;
#31901 = CARTESIAN_POINT ( 'NONE',  ( 122.0994348109119443, -10.15424416112533912, -14.75197769757731336 ) ) ;
#31902 = EDGE_CURVE ( 'NONE', #40888, #424, #7940, .T. ) ;
#31903 = AXIS2_PLACEMENT_3D ( 'NONE', #24389, #428, #24610 ) ;
#31904 = CARTESIAN_POINT ( 'NONE',  ( 124.1983214775786166, -8.166667518702819706, -8.995218007635861213 ) ) ;
#31905 = CARTESIAN_POINT ( 'NONE',  ( 111.8886348109120092, -6.222761293078241884, -8.102969835052219238 ) ) ;
#31906 = DIRECTION ( 'NONE',  ( 0.9609149988134837450, -0.1028163501681639419, 0.2570431154366518145 ) ) ;
#31907 = CARTESIAN_POINT ( 'NONE',  ( 125.1269327111056953, -1.267766418764818770, -16.93314635290698078 ) ) ;
#31908 = CARTESIAN_POINT ( 'NONE',  ( 112.3424481442453384, -6.344957434206662583, -7.627207830600332805 ) ) ;
#31909 = ORIENTED_EDGE ( 'NONE', *, *, #30899, .T. ) ;
#31910 = CARTESIAN_POINT ( 'NONE',  ( 114.3024890045248156, -9.868328341294098749, -11.32035403202665869 ) ) ;
#31911 = CARTESIAN_POINT ( 'NONE',  ( 121.6456214775786293, -10.63000616557722466, -14.87417383870573495 ) ) ;
#31912 = CARTESIAN_POINT ( 'NONE',  ( 59.90552009294155766, -2.897503654462286971, -19.39321520033830737 ) ) ;
#31913 = VERTEX_POINT ( 'NONE', #32332 ) ;
#31914 = CARTESIAN_POINT ( 'NONE',  ( 111.9453614775786434, -1.561330072975668060, -17.79121239304076596 ) ) ;
#31915 = CARTESIAN_POINT ( 'NONE',  ( 123.5176014775786228, -9.261995988541697145, -16.69588392320189030 ) ) ;
#31916 = CARTESIAN_POINT ( 'NONE',  ( 110.6214733795247867, -1.325403438956533675, -9.854619843455175499 ) ) ;
#31917 = CARTESIAN_POINT ( 'NONE',  ( 122.8368814775786291, -7.894159318335828068, -9.358103419637847864 ) ) ;
#31918 = ORIENTED_EDGE ( 'NONE', *, *, #4258, .F. ) ;
#31919 = CARTESIAN_POINT ( 'NONE',  ( 113.1366214775786432, -1.834011780172310813, -8.268836392978581529 ) ) ;
#31920 = B_SPLINE_CURVE_WITH_KNOTS ( 'NONE', 3,
 ( #37028, #26106, #30208, #9237, #29979, #43444, #44129, #33374, #4897, #12437 ),
 .UNSPECIFIED., .F., .F.,
 ( 4, 3, 3, 4 ),
 ( 0.000000000000000000, 0.0001671877560958114864, 0.0003343755126086554838, 0.0006438490228507209303 ),
 .UNSPECIFIED. ) ;
#31921 = FACE_OUTER_BOUND ( 'NONE', #26500, .T. ) ;
#31922 = CARTESIAN_POINT ( 'NONE',  ( 79.62450370917392206, 5.105616368456423082, -20.14282611309224436 ) ) ;
#31923 = CARTESIAN_POINT ( 'NONE',  ( 111.4441597945729541, -2.483185513731533511, -17.81261398230368798 ) ) ;
#31924 = CARTESIAN_POINT ( 'NONE',  ( 111.7751814775786556, -2.084020599724406786, -8.691656652584148546 ) ) ;
#31925 = CYLINDRICAL_SURFACE ( 'NONE', #18218, 5.000000000000004441 ) ;
#31926 = DIRECTION ( 'NONE',  ( -1.000000000000000000, 0.000000000000000000, 0.000000000000000000 ) ) ;
#31927 = CARTESIAN_POINT ( 'NONE',  ( 123.5743281442453139, -7.893985811506177619, -18.51759400769804742 ) ) ;
#31929 = CARTESIAN_POINT ( 'NONE',  ( 124.3117748109119844, 0.1319031606808879209, -14.10382304977623669 ) ) ;
#31928 = CARTESIAN_POINT ( 'NONE',  ( 122.5532481442453019, -10.63000616557722466, -14.87417383870573495 ) ) ;
#31930 = CARTESIAN_POINT ( 'NONE',  ( 119.7736414775786358, 0.1319031606808879209, -14.10382304977623669 ) ) ;
#31931 = CARTESIAN_POINT ( 'NONE',  ( 115.5212212410415873, 0.7607806665037644134, -12.14321520033829493 ) ) ;
#31932 = CARTESIAN_POINT ( 'NONE',  ( 120.1140014775786398, -1.561330072975668504, -17.79121239304076951 ) ) ;
#31933 = VERTEX_POINT ( 'NONE', #17981 ) ;
#31934 = CARTESIAN_POINT ( 'NONE',  ( 111.8752889883689932, 0.3193521225029610777, -12.14321520033831625 ) ) ;
#31935 = CARTESIAN_POINT ( 'NONE',  ( 116.1082702545247827, -10.62599879583958717, -15.77991374673208469 ) ) ;
#31936 = CARTESIAN_POINT ( 'NONE',  ( 114.9970202545248412, 0.1403307496149616695, -11.32035403202665336 ) ) ;
#31937 = CARTESIAN_POINT ( 'NONE',  ( 109.2324108795247923, -1.325403438956436419, -16.93181055722141792 ) ) ;
#31938 = CARTESIAN_POINT ( 'NONE',  ( 115.1359265045248605, -2.791137627527939813, -8.388885654883777576 ) ) ;
#31939 = CARTESIAN_POINT ( 'NONE',  ( 124.5954081442453116, -3.383040157471821630, -19.15922257007629170 ) ) ;
#31940 = CARTESIAN_POINT ( 'NONE',  ( 113.0231681442453322, 0.9020085738987339008, -11.91225656197089222 ) ) ;
#31941 = VERTEX_POINT ( 'NONE', #11374 ) ;
#31942 = CARTESIAN_POINT ( 'NONE',  ( 114.1009748109119784, -5.574606645277164318, -18.38911715685844683 ) ) ;
#31943 = CARTESIAN_POINT ( 'NONE',  ( 107.2182702545248105, -10.62599879583958717, -15.77991374673208469 ) ) ;
#31944 = CARTESIAN_POINT ( 'NONE',  ( 119.0361948109119794, -2.084020599724404121, -8.691656652584155651 ) ) ;
#31945 = CARTESIAN_POINT ( 'NONE',  ( 70.19189222814998175, -60.04498257489500190, -37.22079287717834717 ) ) ;
#31946 = CARTESIAN_POINT ( 'NONE',  ( 125.1626748109119802, -9.988377603198980381, -10.36322818467138518 ) ) ;
#31947 = CARTESIAN_POINT ( 'NONE',  ( -13.74785857260074096, -3.813629379304071421, -18.29023369286690581 ) ) ;
#31948 = CARTESIAN_POINT ( 'NONE',  ( 117.9583881442453048, -10.30919188438810075, -12.61870101168855918 ) ) ;
#31949 = CARTESIAN_POINT ( 'NONE',  ( 116.2471765045247594, -7.250697342233347165, -19.15521520033831138 ) ) ;
#31950 = CARTESIAN_POINT ( 'NONE',  ( 111.2465515045248168, -6.936859964151250502, -18.39754474579286025 ) ) ;
#31951 = ORIENTED_EDGE ( 'NONE', *, *, #15843, .T. ) ;
#31952 = CARTESIAN_POINT ( 'NONE',  ( 127.7429221096195420, -7.069607264515464173, -8.068942598320006709 ) ) ;
#31953 = CARTESIAN_POINT ( 'NONE',  ( 114.9518748109119883, -7.643976991954077427, -18.09477374809248928 ) ) ;
#31954 = CARTESIAN_POINT ( 'NONE',  ( 111.9453614775786434, -1.561330072975668060, -17.79121239304076596 ) ) ;
#31955 = CARTESIAN_POINT ( 'NONE',  ( 111.7751814775786556, -7.893985811506177619, -18.51759400769804742 ) ) ;
#31956 = CARTESIAN_POINT ( 'NONE',  ( 118.5256548109119876, -8.899110576539721151, -16.42337572283488711 ) ) ;
#31957 = CARTESIAN_POINT ( 'NONE',  ( 118.6958348109119754, -3.505236298600246325, -18.68346056562440793 ) ) ;
#31958 = CARTESIAN_POINT ( 'NONE',  ( 117.1642148109119859, -0.8288870151387760510, -10.36305467784173118 ) ) ;
#31959 = ORIENTED_EDGE ( 'NONE', *, *, #5018, .F. ) ;
#31960 = EDGE_CURVE ( 'NONE', #14735, #41199, #20539, .T. ) ;
#31961 = DIRECTION ( 'NONE',  ( 0.000000000000000000, 0.000000000000000000, -1.000000000000000000 ) ) ;
#31962 = AXIS2_PLACEMENT_3D ( 'NONE', #42574, #4256, #7230 ) ;
#31963 = DIRECTION ( 'NONE',  ( -1.000000000000000000, 0.000000000000000000, 0.000000000000000000 ) ) ;
#31964 = CARTESIAN_POINT ( 'NONE',  ( 115.6325948109119821, -9.565557343593413364, -10.61323700422348004 ) ) ;
#31965 = EDGE_LOOP ( 'NONE', ( #7426, #40693, #7326, #2143 ) ) ;
#31966 = AXIS2_PLACEMENT_3D ( 'NONE', #41398, #34515, #44811 ) ;
#31967 = DIRECTION ( 'NONE',  ( 0.000000000000000000, 0.3818493186865927203, -0.9242245927363029745 ) ) ;
#31968 = EDGE_CURVE ( 'NONE', #19363, #42815, #28252, .T. ) ;
#31969 = CARTESIAN_POINT ( 'NONE',  ( 106.8710046295248759, -4.863998795839590272, -7.631215200338315796 ) ) ;
#31970 = EDGE_CURVE ( 'NONE', #1522, #8271, #32165, .T. ) ;
#31971 = CARTESIAN_POINT ( 'NONE',  ( 111.0381921295247878, -9.868328341294093420, -13.39321520033831447 ) ) ;
#31972 = CARTESIAN_POINT ( 'NONE',  ( 112.1722681442453222, -8.899110576539710493, -16.42337572283490132 ) ) ;
#31973 = ORIENTED_EDGE ( 'NONE', *, *, #5843, .T. ) ;
#31974 = CARTESIAN_POINT ( 'NONE',  ( 118.1285681442453068, -2.084020599724406786, -8.691656652584148546 ) ) ;
#31975 = CARTESIAN_POINT ( 'NONE',  ( 117.2776681442452968, -4.153390946401325223, -8.397313243818185668 ) ) ;
#31976 = CARTESIAN_POINT ( 'NONE',  ( 124.5807827564429431, -9.809262384845451876, -14.15072059919280534 ) ) ;
#31977 = CARTESIAN_POINT ( 'NONE',  ( 121.8965016859119856, -9.665098340737509730, -17.37397104707595474 ) ) ;
#31978 = ORIENTED_EDGE ( 'NONE', *, *, #26998, .F. ) ;
#31979 = DIRECTION ( 'NONE',  ( -0.9908103287288504424, 0.1352586133457952811, 0.000000000000000000 ) ) ;
#31980 = CARTESIAN_POINT ( 'NONE',  ( 125.2231329858125264, -2.209379012606767390, -6.577246691088228125 ) ) ;
#31981 = CARTESIAN_POINT ( 'NONE',  ( 111.5243640045248412, -10.62599879583958717, -11.00651665394454604 ) ) ;
#31982 = CARTESIAN_POINT ( 'NONE',  ( 117.1329525761119186, -11.25461401719748977, -21.76703976714820143 ) ) ;
#31983 = EDGE_CURVE ( 'NONE', #5920, #39662, #18443, .T. ) ;
#31984 = CARTESIAN_POINT ( 'NONE',  ( 112.9664414775786412, 0.5811942927096154232, -14.16772938898807155 ) ) ;
#31985 = CARTESIAN_POINT ( 'NONE',  ( 116.9373081442452929, -1.833838273342659253, -17.42832698103878286 ) ) ;
#31986 = LINE ( 'NONE', #10144, #4627 ) ;
#31987 = EDGE_CURVE ( 'NONE', #18337, #30859, #18354, .T. ) ;
#31988 = EDGE_CURVE ( 'NONE', #8204, #34692, #11821, .T. ) ;
#31989 = ORIENTED_EDGE ( 'NONE', *, *, #31970, .T. ) ;
#31990 = CARTESIAN_POINT ( 'NONE',  ( 115.0653281442453277, -3.505236298600246325, -18.68346056562440793 ) ) ;
#31991 = CARTESIAN_POINT ( 'NONE',  ( 116.3860827545247787, -2.477300249445798297, -19.15521520033831138 ) ) ;
#31992 = CARTESIAN_POINT ( 'NONE',  ( 125.1733191598100916, -1.295815253274133161, -16.89579513612386563 ) ) ;
#31993 = DIRECTION ( 'NONE',  ( 0.7871354856660198740, 0.4483307682966886643, 0.4235767337848242442 ) ) ;
#31994 = CARTESIAN_POINT ( 'NONE',  ( 113.6471614775786492, -5.638512984488999180, -18.83840828888717311 ) ) ;
#31995 = VERTEX_POINT ( 'NONE', #43055 ) ;
#31996 = CARTESIAN_POINT ( 'NONE',  ( 118.6958348109119754, -6.344957434206665248, -7.627207830600338134 ) ) ;
#31997 = DIRECTION ( 'NONE',  ( 0.000000000000000000, 0.000000000000000000, 1.000000000000000000 ) ) ;
#31998 = CARTESIAN_POINT ( 'NONE',  ( 110.8992858795247827, -0.7896495226426338832, -17.46756447353520159 ) ) ;
#31999 = CARTESIAN_POINT ( 'NONE',  ( 116.9940348109119839, -9.988377603198976828, -10.36322818467138340 ) ) ;
#32000 = CARTESIAN_POINT ( 'NONE',  ( 112.3424481442453384, -6.344957434206662583, -7.627207830600332805 ) ) ;
#32001 = CARTESIAN_POINT ( 'NONE',  ( 127.2313854076800794, -10.35564729092436309, -13.79736478706461433 ) ) ;
#32002 = FACE_OUTER_BOUND ( 'NONE', #34996, .T. ) ;
#32003 = CARTESIAN_POINT ( 'NONE',  ( 109.0240515045248202, -6.936859964151250502, -18.39754474579286025 ) ) ;
#32004 = VERTEX_POINT ( 'NONE', #14561 ) ;
#32005 = CARTESIAN_POINT ( 'NONE',  ( 58.92639935879823554, -16.07256461744605147, -19.39321520033831447 ) ) ;
#32006 = CARTESIAN_POINT ( 'NONE',  ( 109.2294421271526943, -7.422887316267482660, -18.05243104752941719 ) ) ;
#32007 = CARTESIAN_POINT ( 'NONE',  ( 116.0864081442453113, -0.1624402480850797581, -16.17319339645315424 ) ) ;
#32008 = CARTESIAN_POINT ( 'NONE',  ( 65.02437422720751670, -13.34618800689889362, -11.75271837916926820 ) ) ;
#32009 = CARTESIAN_POINT ( 'NONE',  ( 116.5249890045247980, -9.868328341294098749, -11.32035403202665869 ) ) ;
#32010 = CARTESIAN_POINT ( 'NONE',  ( 114.3024890045248156, -9.868328341294098749, -11.32035403202665869 ) ) ;
#32011 = CIRCLE ( 'NONE', #42961, 3.000000000000001776 ) ;
#32012 = CARTESIAN_POINT ( 'NONE',  ( 127.1653849502323226, -5.235753722768803797, -7.932320622462421866 ) ) ;
#32013 = CARTESIAN_POINT ( 'NONE',  ( 112.6260814775786514, -0.8288870151387760510, -10.36305467784173118 ) ) ;
#32014 = DIRECTION ( 'NONE',  ( 0.000000000000000000, 0.6004852223388318366, -0.7996358532186281787 ) ) ;
#32015 =( BOUNDED_CURVE ( )  B_SPLINE_CURVE ( 2, ( #12841, #27193, #9184, #14114, #37199, #9871, #3618, #31431, #41938, #198, #19661, #10701, #26740, #9404, #5972, #19896, #33783 ),
 .UNSPECIFIED., .F., .T. ) 
 B_SPLINE_CURVE_WITH_KNOTS ( ( 3, 2, 2, 2, 2, 2, 2, 2, 3 ),
 ( 0.7670046674808920217, 0.7734375000000000000, 0.7812500000000000000, 0.7890625000000000000, 0.7968750000000000000, 0.8046875000000000000, 0.8125000000000000000, 0.8203125000000000000, 0.8267453325190590174 ),
 .UNSPECIFIED. ) 
 CURVE ( )  GEOMETRIC_REPRESENTATION_ITEM ( )  RATIONAL_B_SPLINE_CURVE ( ( 0.9778625265006449796, 0.9373222120152220338, 1.000000000000000000, 0.9238795325112869605, 1.000000000000000000, 0.9238795325112869605, 1.000000000000000000, 0.9238795325112869605, 1.000000000000000000, 0.9238795325112869605, 1.000000000000000000, 0.9238795325112869605, 1.000000000000000000, 0.9238795325112869605, 1.000000000000000000, 0.9373222120157009840, 0.9778625265000250311 ) ) 
 REPRESENTATION_ITEM ( '' )  );
#32016 = CARTESIAN_POINT ( 'NONE',  ( 124.1415948109119540, -6.344957434206665248, -7.627207830600338134 ) ) ;
#32017 = CARTESIAN_POINT ( 'NONE',  ( 116.4834948109119779, -1.561330072975668504, -17.79121239304076951 ) ) ;
#32018 = EDGE_LOOP ( 'NONE', ( #11336, #1544, #17253, #37791 ) ) ;
#32019 = CARTESIAN_POINT ( 'NONE',  ( 116.1431348109119881, 0.1319031606808879209, -14.10382304977623669 ) ) ;
#32020 = CARTESIAN_POINT ( 'NONE',  ( 89.78938736644981589, -25.99489077589524300, -13.39321520033831625 ) ) ;
#32021 = CARTESIAN_POINT ( 'NONE',  ( 116.8238548109119819, -4.089484607189486809, -7.948022111789456723 ) ) ;
#32022 = CARTESIAN_POINT ( 'NONE',  ( 118.2987481442453088, -7.894159318335828068, -9.358103419637847864 ) ) ;
#32023 = VERTEX_POINT ( 'NONE', #646 ) ;
#32024 = CARTESIAN_POINT ( 'NONE',  ( 121.0216281442452981, -7.894159318335828068, -9.358103419637847864 ) ) ;
#32025 = CARTESIAN_POINT ( 'NONE',  ( 121.1918081442452859, 0.9020085738987339008, -11.91225656197089222 ) ) ;
#32026 = AXIS2_PLACEMENT_3D ( 'NONE', #42169, #31439, #28260 ) ;
#32027 = FACE_OUTER_BOUND ( 'NONE', #32069, .T. ) ;
#32028 = CARTESIAN_POINT ( 'NONE',  ( 111.0381921295247878, 0.8980012041604618078, -13.39321520033831447 ) ) ;
#32029 = EDGE_CURVE ( 'NONE', #38271, #28617, #42834, .T. ) ;
#32030 = DIRECTION ( 'NONE',  ( -0.9970811988817434024, 0.07634843047859724008, 9.125038414728753042E-18 ) ) ;
#32031 = CARTESIAN_POINT ( 'NONE',  ( 116.8689275254964883, 0.3188565254943556693, -14.64321520033831447 ) ) ;
#32032 = CARTESIAN_POINT ( 'NONE',  ( 113.1217858795247935, -8.402594152722688392, -9.854619843455216355 ) ) ;
#32033 = CARTESIAN_POINT ( 'NONE',  ( 113.1933481442453058, -4.089484607189486809, -7.948022111789456723 ) ) ;
#32034 = CIRCLE ( 'NONE', #12407, 1.199999999999999734 ) ;
#32035 = DIRECTION ( 'NONE',  ( 0.1352586133457950590, 0.9908103287288504424, 0.000000000000000000 ) ) ;
#32036 = CARTESIAN_POINT ( 'NONE',  ( 116.3700414775786527, -4.153390946401321671, -8.397313243818183892 ) ) ;
#32037 = DIRECTION ( 'NONE',  ( -1.000000000000000000, 0.000000000000000000, 0.000000000000000000 ) ) ;
#32038 = EDGE_CURVE ( 'NONE', #18777, #29125, #25729, .T. ) ;
#32039 = DIRECTION ( 'NONE',  ( 0.000000000000000000, 0.6004852223388321697, -0.7996358532186279566 ) ) ;
#32040 = CARTESIAN_POINT ( 'NONE',  ( 112.9134265045247645, -2.791137627527939813, -8.388885654883777576 ) ) ;
#32041 = CARTESIAN_POINT ( 'NONE',  ( 113.1933481442453058, -5.574606645277164318, -18.38911715685844683 ) ) ;
#32042 = CARTESIAN_POINT ( 'NONE',  ( 0.04488520489200759078, -6.166763362545027327, -18.19321520033831519 ) ) ;
#32043 = CARTESIAN_POINT ( 'NONE',  ( 69.69189222814998175, -41.76310523276723785, -20.39321520033831447 ) ) ;
#32045 = CARTESIAN_POINT ( 'NONE',  ( 118.7525614775786380, -8.166667518702819706, -8.995218007635861213 ) ) ;
#32044 = CARTESIAN_POINT ( 'NONE',  ( 65.91876108126248823, -14.44801200876193192, -9.970851920820145153 ) ) ;
#32046 = CARTESIAN_POINT ( 'NONE',  ( 118.4122014775786340, -9.859900752359374465, -12.68260735090039404 ) ) ;
#32047 = CARTESIAN_POINT ( 'NONE',  ( 125.8433948109119456, -1.834011780172310813, -8.268836392978581529 ) ) ;
#32048 = ORIENTED_EDGE ( 'NONE', *, *, #8438, .F. ) ;
#32049 = CARTESIAN_POINT ( 'NONE',  ( 54.86886719809545809, -45.79521720516596872, -9.393215200338314474 ) ) ;
#32050 = ADVANCED_FACE ( 'NONE', ( #38946 ), #25505, .T. ) ;
#32051 = CARTESIAN_POINT ( 'NONE',  ( 122.8936081442453059, 0.2603800115204892296, -16.42320221600525088 ) ) ;
#32052 = CARTESIAN_POINT ( 'NONE',  ( 112.4272546295247821, -4.863998795839590272, -18.39754474579285315 ) ) ;
#32053 = CARTESIAN_POINT ( 'NONE',  ( 119.2063748109119814, -7.894159318335828068, -9.358103419637847864 ) ) ;
#32054 = CARTESIAN_POINT ( 'NONE',  ( 117.9016614775786280, -0.1624402480850797581, -16.17319339645315424 ) ) ;
#32055 = CARTESIAN_POINT ( 'NONE',  ( 85.90931634775512293, -27.45388746120685397, -8.668790192341086609 ) ) ;
#32056 = CARTESIAN_POINT ( 'NONE',  ( 114.3719421295247827, 0.8980012041604618078, -13.39321520033831447 ) ) ;
#32057 = CARTESIAN_POINT ( 'NONE',  ( 121.7590748109119687, -2.084020599724406786, -8.691656652584148546 ) ) ;
#32058 = CARTESIAN_POINT ( 'NONE',  ( 122.8368814775786291, -7.894159318335828068, -9.358103419637847864 ) ) ;
#32059 = CARTESIAN_POINT ( 'NONE',  ( 116.5249890045247980, -9.868328341294102302, -11.32035403202661428 ) ) ;
#32060 = AXIS2_PLACEMENT_3D ( 'NONE', #6901, #20812, #24451 ) ;
#32061 = CARTESIAN_POINT ( 'NONE',  ( 109.2294456423300915, -1.194640643069894370, -9.436217729478444838 ) ) ;
#32062 = CARTESIAN_POINT ( 'NONE',  ( 122.3826735609119680, -9.645473719204776586, -14.86997237629376656 ) ) ;
#32063 = CARTESIAN_POINT ( 'NONE',  ( 115.2053796295247849, -4.863998795839590272, -19.15521520033831493 ) ) ;
#32064 = DIRECTION ( 'NONE',  ( 1.000000000000000000, 0.000000000000000000, 0.000000000000000000 ) ) ;
#32065 = CARTESIAN_POINT ( 'NONE',  ( 118.5256548109119876, -0.4660016031367893996, -10.09054647747474043 ) ) ;
#32066 = CARTESIAN_POINT ( 'NONE',  ( 118.1285681442453068, -7.893985811506177619, -18.51759400769804742 ) ) ;
#32067 = CARTESIAN_POINT ( 'NONE',  ( 112.2188952545247531, 0.8980012041604421569, -11.00651665394454071 ) ) ;
#32068 = DIRECTION ( 'NONE',  ( 0.5735764363510499342, 0.3127926500124801890, -0.7570804645221008711 ) ) ;
#32069 = EDGE_LOOP ( 'NONE', ( #23098, #40398, #42130, #36396 ) ) ;
#32070 = CARTESIAN_POINT ( 'NONE',  ( 88.22708560785949317, -3.622631779710408395, -9.893215200338316251 ) ) ;
#32071 = CARTESIAN_POINT ( 'NONE',  ( 117.2776681442452968, -5.638512984488999180, -18.83840828888717311 ) ) ;
#32072 = CARTESIAN_POINT ( 'NONE',  ( 121.9292548109119849, -7.894159318335828068, -9.358103419637847864 ) ) ;
#32073 = APPLICATION_PROTOCOL_DEFINITION ( 'draft international standard', 'automotive_design', 1998, #6729 ) ;
#32074 = TOROIDAL_SURFACE ( 'NONE', #12431, 10.00000000000000000, 2.000000000000000000 ) ;
#32075 = CARTESIAN_POINT ( 'NONE',  ( 111.3780948109119890, -5.574606645277164318, -18.38911715685844683 ) ) ;
#32076 = CARTESIAN_POINT ( 'NONE',  ( 121.9292548109119849, -1.561330072975668948, -17.79121239304076951 ) ) ;
#32077 = CARTESIAN_POINT ( 'NONE',  ( 112.0105358795247810, -0.7896495226426338832, -17.46756447353520159 ) ) ;
#32078 = CARTESIAN_POINT ( 'NONE',  ( 114.8951481442453115, -8.899110576539710493, -16.42337572283490132 ) ) ;
#32079 = CARTESIAN_POINT ( 'NONE',  ( 123.9800954359119771, -11.07370829466463569, -12.81314460846529002 ) ) ;
#32080 = DIRECTION ( 'NONE',  ( 0.9609149988134837450, -0.1028163501681639419, 0.2570431154366518145 ) ) ;
#32081 = VERTEX_POINT ( 'NONE', #32104 ) ;
#32082 = EDGE_CURVE ( 'NONE', #36383, #15954, #1632, .T. ) ;
#32083 = CARTESIAN_POINT ( 'NONE',  ( 120.2990798109119766, -7.200787124940443817, -17.81845355600750835 ) ) ;
#32084 = CARTESIAN_POINT ( 'NONE',  ( 119.6601881442453106, -8.166667518702819706, -8.995218007635861213 ) ) ;
#32085 = ORIENTED_EDGE ( 'NONE', *, *, #20447, .F. ) ;
#32086 = PLANE ( 'NONE',  #40793 ) ;
#32087 = DIRECTION ( 'NONE',  ( 0.9609149988134837450, -0.1028163501681639419, 0.2570431154366518145 ) ) ;
#32088 = CARTESIAN_POINT ( 'NONE',  ( 116.9940348109119839, -0.1624402480850797581, -16.17319339645315424 ) ) ;
#32089 =( BOUNDED_SURFACE ( )  B_SPLINE_SURFACE ( 1, 2, ( 
 ( #40705, #27024, #30664, #34073, #40939, #20636, #16311, #34513, #16998, #41167, #29984, #30438, #12669, #40481, #2383, #44133, #23376 ),
 ( #9464, #13348, #37258, #6030, #19952, #2609, #9926, #44357, #13118, #16769, #27252, #37726, #20412, #34296, #30887, #17213, #3729 ) ),
 .UNSPECIFIED., .F., .F., .F. ) 
 B_SPLINE_SURFACE_WITH_KNOTS ( ( 2, 2 ),
 ( 3, 2, 2, 2, 2, 2, 2, 2, 3 ),
 ( 0.000000000000000000, 1.000000000000000000 ),
 ( 0.000000000000000000, 0.1250000000000000000, 0.2500000000000000000, 0.3750000000000000000, 0.5000000000000000000, 0.6250000000000000000, 0.7500000000000000000, 0.8750000000000000000, 1.000000000000000000 ),
 .UNSPECIFIED. ) 
 GEOMETRIC_REPRESENTATION_ITEM ( )  RATIONAL_B_SPLINE_SURFACE ( (
 ( 1.000000000000000000, 0.9238795325112869605, 1.000000000000000000, 0.9238795325112869605, 1.000000000000000000, 0.9238795325112869605, 1.000000000000000000, 0.9238795325112869605, 1.000000000000000000, 0.9238795325112869605, 1.000000000000000000, 0.9238795325112869605, 1.000000000000000000, 0.9238795325112869605, 1.000000000000000000, 0.9238795325112869605, 1.000000000000000000),
 ( 1.000000000000000000, 0.9238795325112869605, 1.000000000000000000, 0.9238795325112869605, 1.000000000000000000, 0.9238795325112869605, 1.000000000000000000, 0.9238795325112869605, 1.000000000000000000, 0.9238795325112869605, 1.000000000000000000, 0.9238795325112869605, 1.000000000000000000, 0.9238795325112869605, 1.000000000000000000, 0.9238795325112869605, 1.000000000000000000) ) ) 
 REPRESENTATION_ITEM ( '' )  SURFACE ( )  );
#32090 = DIRECTION ( 'NONE',  ( -1.000000000000000000, 0.000000000000000000, 0.000000000000000000 ) ) ;
#32091 = CARTESIAN_POINT ( 'NONE',  ( 64.22825944749166638, -35.92680753996140197, -5.785566283887345840 ) ) ;
#32092 = CARTESIAN_POINT ( 'NONE',  ( 118.9227414775786542, 0.4262465694468514643, -12.03445270309931736 ) ) ;
#32093 = B_SPLINE_CURVE_WITH_KNOTS ( 'NONE', 3,
 ( #12198, #40001, #33140, #15841, #6252, #17415, #23594, #16752, #45016, #27685 ),
 .UNSPECIFIED., .F., .F.,
 ( 4, 3, 3, 4 ),
 ( 0.000000000000000000, 0.0001671877560958089928, 0.0003343755126086549959, 0.0006438490228507220145 ),
 .UNSPECIFIED. ) ;
#32094 = CARTESIAN_POINT ( 'NONE',  ( 121.9100498793805230, -2.191907684172563986, -18.20049396185734025 ) ) ;
#32095 = CARTESIAN_POINT ( 'NONE',  ( 121.5888948109119809, 0.1319031606808879209, -14.10382304977623669 ) ) ;
#32096 = AXIS2_PLACEMENT_3D ( 'NONE', #18684, #21875, #25305 ) ;
#32097 = EDGE_CURVE ( 'NONE', #21089, #31317, #21851, .T. ) ;
#32098 = CARTESIAN_POINT ( 'NONE',  ( 124.6574308310802621, -11.08444345384245544, -8.635704745763826296 ) ) ;
#32099 = CARTESIAN_POINT ( 'NONE',  ( 118.4689281442453250, -10.15424416112533912, -14.75197769757731336 ) ) ;
#32100 = AXIS2_PLACEMENT_3D ( 'NONE', #22257, #18616, #16094 ) ;
#32101 = CARTESIAN_POINT ( 'NONE',  ( 113.8173414775786512, 0.2603800115204892296, -16.42320221600525088 ) ) ;
#32102 = CARTESIAN_POINT ( 'NONE',  ( 120.5110881442453206, -6.344957434206665248, -7.627207830600338134 ) ) ;
#32103 = CARTESIAN_POINT ( 'NONE',  ( 125.6164881442453094, -9.565557343593413364, -10.61323700422348004 ) ) ;
#32104 = CARTESIAN_POINT ( 'NONE',  ( 83.49267580666517574, -32.76310523276723785, -23.89321520033831803 ) ) ;
#32105 = CARTESIAN_POINT ( 'NONE',  ( 119.0929214775786278, -4.153390946401325223, -8.397313243818185668 ) ) ;
#32106 = ORIENTED_EDGE ( 'NONE', *, *, #33402, .F. ) ;
#32107 = CARTESIAN_POINT ( 'NONE',  ( 120.9081748109119872, -5.638512984488999180, -18.83840828888717311 ) ) ;
#32108 = CARTESIAN_POINT ( 'NONE',  ( 111.6632702545248605, 0.1403307496149616695, -11.32035403202665336 ) ) ;
#32109 = CARTESIAN_POINT ( 'NONE',  ( -3.429934629567074733, -4.841764211284793618, -17.89321520033831447 ) ) ;
#32110 = LINE ( 'NONE', #35753, #6534 ) ;
#32111 = CARTESIAN_POINT ( 'NONE',  ( -1.932019669644797988, -4.762702382056356321, -8.893215200338314474 ) ) ;
#32112 = CARTESIAN_POINT ( 'NONE',  ( 124.5386814775786206, -5.638512984488999180, -18.83840828888717311 ) ) ;
#32113 = VERTEX_POINT ( 'NONE', #21627 ) ;
#32114 = DIRECTION ( 'NONE',  ( 0.000000000000000000, 0.3818493186865927203, -0.9242245927363029745 ) ) ;
#32115 = CARTESIAN_POINT ( 'NONE',  ( 123.1772414775786189, -5.574606645277164318, -18.38911715685844683 ) ) ;
#32116 = CARTESIAN_POINT ( 'NONE',  ( 121.4103298109119748, -2.173413727453600508, -8.297982527556802879 ) ) ;
#32117 = CARTESIAN_POINT ( 'NONE',  ( 62.99192496234383043, -14.62834943820164746, -18.63369276689623533 ) ) ;
#32118 = CARTESIAN_POINT ( 'NONE',  ( 120.2542535264548889, -8.247323210606168686, -17.08054893949881148 ) ) ;
#32119 = CARTESIAN_POINT ( 'NONE',  ( 113.6774108795247997, -1.325403438956436419, -16.93181055722141792 ) ) ;
#32120 = ORIENTED_EDGE ( 'NONE', *, *, #5330, .F. ) ;
#32121 = CARTESIAN_POINT ( 'NONE',  ( 113.3635281442453504, -9.988377603198976828, -10.36322818467138340 ) ) ;
#32122 = CARTESIAN_POINT ( 'NONE',  ( 115.2922348109119781, -10.63000616557722466, -14.87417383870573495 ) ) ;
#32123 = CARTESIAN_POINT ( 'NONE',  ( 88.49587816393574258, -11.41200697344714143, -13.89319073456437792 ) ) ;
#32124 = AXIS2_PLACEMENT_3D ( 'NONE', #15847, #22452, #40696 ) ;
#32125 = CARTESIAN_POINT ( 'NONE',  ( 120.0572748109119772, -6.222761293078241884, -8.102969835052219238 ) ) ;
#32126 = CARTESIAN_POINT ( 'NONE',  ( 112.4559014775786778, -0.1624402480850797581, -16.17319339645315424 ) ) ;
#32127 =( NAMED_UNIT ( * ) PLANE_ANGLE_UNIT ( ) SI_UNIT ( $, .RADIAN. ) );
#32128 = CARTESIAN_POINT ( 'NONE',  ( 123.8579614775786126, 0.5811942927096110934, -14.16772938898807510 ) ) ;
#32129 = DIRECTION ( 'NONE',  ( 1.000000000000000000, 0.000000000000000000, -0.000000000000000000 ) ) ;
#32130 = CARTESIAN_POINT ( 'NONE',  ( 63.27883505452616930, -30.76310523276723785, -21.89321520033831447 ) ) ;
#32131 = CARTESIAN_POINT ( 'NONE',  ( 110.2548541094426895, 0.3591747506842615789, -12.14321520033831625 ) ) ;
#32132 = CARTESIAN_POINT ( 'NONE',  ( 112.1722681442453222, -0.4660016031367893996, -10.09054647747474043 ) ) ;
#32133 = ORIENTED_EDGE ( 'NONE', *, *, #11207, .F. ) ;
#32134 = CARTESIAN_POINT ( 'NONE',  ( 117.0111608795247946, -1.325403438956436419, -16.93181055722141792 ) ) ;
#32135 = VECTOR ( 'NONE', #14860, 1000.000000000000000 ) ;
#32136 = CARTESIAN_POINT ( 'NONE',  ( 119.4900081442453086, -1.834011780172310813, -8.268836392978581529 ) ) ;
#32137 = CARTESIAN_POINT ( 'NONE',  ( 61.35525772184064408, -2.221568293060733001, -19.50743695395307853 ) ) ;
#32138 = VERTEX_POINT ( 'NONE', #7484 ) ;
#32139 = PRODUCT_DEFINITION_SHAPE ( 'NONE', 'NONE',  #45151 ) ;
#32140 = CARTESIAN_POINT ( 'NONE',  ( 92.04708369096698561, -25.38011337280982715, -14.88121679464376257 ) ) ;
#32141 = CARTESIAN_POINT ( 'NONE',  ( 125.1626748109119802, -9.988377603198980381, -10.36322818467138518 ) ) ;
#32142 = CARTESIAN_POINT ( 'NONE',  ( 128.2184548109119930, -4.105398160058917334, -19.34506575923121474 ) ) ;
#32143 = CARTESIAN_POINT ( 'NONE',  ( 122.6667014775786413, -2.084020599724406786, -8.691656652584148546 ) ) ;
#32144 = VERTEX_POINT ( 'NONE', #21403 ) ;
#32145 = CARTESIAN_POINT ( 'NONE',  ( 118.9227414775786400, -10.63000616557722466, -14.87417383870573495 ) ) ;
#32146 = CARTESIAN_POINT ( 'NONE',  ( 74.47157298427187300, -3.053873105668316601, -10.39321520033831625 ) ) ;
#32147 = CARTESIAN_POINT ( 'NONE',  ( 112.1114130180079798, 0.7607806665037644134, -14.64321520033833046 ) ) ;
#32148 = CARTESIAN_POINT ( 'NONE',  ( 91.77400275106518279, -25.99489077589524300, -13.39321520033831625 ) ) ;
#32149 = CARTESIAN_POINT ( 'NONE',  ( 124.0848681442452772, -4.089484607189486809, -7.948022111789456723 ) ) ;
#32150 = DIRECTION ( 'NONE',  ( 0.000000000000000000, 0.3818493186865927203, -0.9242245927363029745 ) ) ;
#32151 = CIRCLE ( 'NONE', #12523, 2.000000000000001776 ) ;
#32152 = EDGE_CURVE ( 'NONE', #6107, #35524, #15014, .T. ) ;
#32153 = DIRECTION ( 'NONE',  ( -0.000000000000000000, -0.9284778069183718952, -0.3713878862591649677 ) ) ;
#32154 = CARTESIAN_POINT ( 'NONE',  ( 123.1205148109119563, -1.834011780172310813, -8.268836392978581529 ) ) ;
#32156 = CARTESIAN_POINT ( 'NONE',  ( 122.3263414775786373, -3.505236298600246325, -18.68346056562440793 ) ) ;
#32155 = CARTESIAN_POINT ( 'NONE',  ( 121.4187148109119789, -6.344957434206665248, -7.627207830600338134 ) ) ;
#32157 = CARTESIAN_POINT ( 'NONE',  ( 120.6463454359119822, 0.5291689781388270175, -13.89700978578772705 ) ) ;
#32158 = CARTESIAN_POINT ( 'NONE',  ( 124.4819548109119722, -2.084020599724406786, -8.691656652584148546 ) ) ;
#32159 = CARTESIAN_POINT ( 'NONE',  ( 113.3635281442453504, -0.1624402480850797581, -16.17319339645315424 ) ) ;
#32160 = CARTESIAN_POINT ( 'NONE',  ( 119.7169148109119874, -9.988377603198976828, -10.36322818467138340 ) ) ;
#32161 = ORIENTED_EDGE ( 'NONE', *, *, #17851, .T. ) ;
#32162 = CARTESIAN_POINT ( 'NONE',  ( 111.7802383310706773, 0.1843591316377651834, -12.14321520033831625 ) ) ;
#32163 = CARTESIAN_POINT ( 'NONE',  ( 114.9970202545248412, -10.62599879583958717, -15.77991374673208469 ) ) ;
#32164 = CARTESIAN_POINT ( 'NONE',  ( 113.3995983795247895, -8.402594152722688392, -16.93181055722141792 ) ) ;
#32165 = CIRCLE ( 'NONE', #4504, 2.000000000000000444 ) ;
#32166 = CARTESIAN_POINT ( 'NONE',  ( 112.8439733795247832, -1.325403438956436419, -9.854619843455211026 ) ) ;
#32167 = FACE_OUTER_BOUND ( 'NONE', #28058, .T. ) ;
#32168 = CARTESIAN_POINT ( 'NONE',  ( 114.2144281442453178, -8.166667518702817929, -8.995218007635859436 ) ) ;
#32169 = EDGE_LOOP ( 'NONE', ( #44782, #29038 ) ) ;
#32170 = CARTESIAN_POINT ( 'NONE',  ( 112.3424481442453384, -3.505236298600246325, -18.68346056562440793 ) ) ;
#32171 = CARTESIAN_POINT ( 'NONE',  ( 105.6903015045248253, -2.477300249445798297, -7.631215200338321125 ) ) ;
#32172 = DIRECTION ( 'NONE',  ( 0.7871354856660167654, -0.6167752151498625546, -0.002461946824136807422 ) ) ;
#32173 = FACE_OUTER_BOUND ( 'NONE', #36335, .T. ) ;
#32174 = DIRECTION ( 'NONE',  ( -0.9609149988134834119, 0.1028163501681648995, -0.2570431154366529802 ) ) ;
#32175 = CARTESIAN_POINT ( 'NONE',  ( -12.73631100612642797, -4.238385078766282454, -19.35607154375884775 ) ) ;
#32176 = CARTESIAN_POINT ( 'NONE',  ( 115.0653281442453277, -6.344957434206662583, -7.627207830600332805 ) ) ;
#32177 = DIRECTION ( 'NONE',  ( 0.000000000000000000, -0.3818493186865927203, 0.9242245927363029745 ) ) ;
#32178 = CARTESIAN_POINT ( 'NONE',  ( 110.6214733795247867, -1.325403438956436419, -9.854619843455211026 ) ) ;
#32179 = VERTEX_POINT ( 'NONE', #22083 ) ;
#32180 = DIRECTION ( 'NONE',  ( 0.7962509850245486076, 0.6049664196031347974, 0.000000000000000000 ) ) ;
#32181 = CARTESIAN_POINT ( 'NONE',  ( 118.5256548109119876, -8.899110576539710493, -16.42337572283490132 ) ) ;
#32182 = CARTESIAN_POINT ( 'NONE',  ( 115.5758681442453053, -1.561330072975668060, -17.79121239304076951 ) ) ;
#32183 = DIRECTION ( 'NONE',  ( 1.000000000000000000, 0.000000000000000000, -0.000000000000000000 ) ) ;
#32184 = CARTESIAN_POINT ( 'NONE',  ( 118.0151148109119816, 0.4262465694468589028, -12.03445270309934578 ) ) ;
#32185 = CARTESIAN_POINT ( 'NONE',  ( 118.1285681442453068, -2.084020599724406786, -8.691656652584148546 ) ) ;
#32186 = CARTESIAN_POINT ( 'NONE',  ( 117.3911214775786505, -7.894159318335828068, -9.358103419637847864 ) ) ;
#32187 = EDGE_LOOP ( 'NONE', ( #17816, #42366, #41588, #43418 ) ) ;
#32188 = CARTESIAN_POINT ( 'NONE',  ( 122.4521266859119635, -9.033780868592240054, -16.85052413769862056 ) ) ;
#32189 = LINE ( 'NONE', #26934, #43362 ) ;
#32190 = CARTESIAN_POINT ( 'NONE',  ( 119.2063748109119814, -7.894159318335828068, -9.358103419637847864 ) ) ;
#32191 = ORIENTED_EDGE ( 'NONE', *, *, #39681, .F. ) ;
#32192 = LINE ( 'NONE', #39720, #30388 ) ;
#32193 = CARTESIAN_POINT ( 'NONE',  ( 113.8740681442453138, 0.5811942927096154232, -14.16772938898807155 ) ) ;
#32194 = CARTESIAN_POINT ( 'NONE',  ( 106.3153796295248412, -4.863998795839590272, -8.388885654883775800 ) ) ;
#32195 = CARTESIAN_POINT ( 'NONE',  ( 114.1009748109119784, -5.574606645277164318, -18.38911715685844683 ) ) ;
#32196 = EDGE_LOOP ( 'NONE', ( #20416, #40631, #34601, #9336 ) ) ;
#32197 = CIRCLE ( 'NONE', #30029, 2.000000000000000444 ) ;
#32198 = VERTEX_POINT ( 'NONE', #28480 ) ;
#32199 = CARTESIAN_POINT ( 'NONE',  ( 117.5045748109119756, -9.859900752359374465, -12.68260735090039404 ) ) ;
#32200 = CARTESIAN_POINT ( 'NONE',  ( 117.1074881442453233, 0.4262465694468514643, -12.03445270309931736 ) ) ;
#32201 = CARTESIAN_POINT ( 'NONE',  ( 124.5391625940361138, -9.844727480109712658, -12.94707959821569077 ) ) ;
#32202 = STYLED_ITEM ( 'NONE', ( #14814 ), #15621 ) ;
#32203 = CARTESIAN_POINT ( 'NONE',  ( 124.1190016859119680, -9.665098340737509730, -17.37397104707595474 ) ) ;
#32204 = ORIENTED_EDGE ( 'NONE', *, *, #33337, .F. ) ;
#32205 = LINE ( 'NONE', #14665, #25203 ) ;
#32206 = DIRECTION ( 'NONE',  ( 0.000000000000000000, 0.000000000000000000, 1.000000000000000000 ) ) ;
#32207 = CARTESIAN_POINT ( 'NONE',  ( 109.6491296295247793, -4.863998795839590272, -19.15521520033831493 ) ) ;
#32208 = CARTESIAN_POINT ( 'NONE',  ( 61.69189222814998175, -69.76310523276724496, -16.89321520033831447 ) ) ;
#32209 = CARTESIAN_POINT ( 'NONE',  ( 125.9568481442452850, -3.505236298600246325, -18.68346056562440793 ) ) ;
#32210 = CARTESIAN_POINT ( 'NONE',  ( 118.4122014775786340, -9.859900752359374465, -12.68260735090039404 ) ) ;
#32211 = CARTESIAN_POINT ( 'NONE',  ( 61.69189222814998175, -80.85404093559408523, -31.07034979220001603 ) ) ;
#32212 = ORIENTED_EDGE ( 'NONE', *, *, #27452, .F. ) ;
#32213 = CARTESIAN_POINT ( 'NONE',  ( 118.6391081442452986, -5.574606645277164318, -18.38911715685844683 ) ) ;
#32214 = CIRCLE ( 'NONE', #41005, 1.499999999999998002 ) ;
#32215 = CARTESIAN_POINT ( 'NONE',  ( 116.1777233795247781, -8.938348069036489818, -17.46756447353520159 ) ) ;
#32216 = AXIS2_PLACEMENT_3D ( 'NONE', #6279, #20199, #37961 ) ;
#32217 = FACE_OUTER_BOUND ( 'NONE', #30299, .T. ) ;
#32218 = CARTESIAN_POINT ( 'NONE',  ( 116.4555358795247884, -0.7896495226426338832, -17.46756447353520159 ) ) ;
#32219 = CARTESIAN_POINT ( 'NONE',  ( 114.1009748109119784, -4.089484607189486809, -7.948022111789456723 ) ) ;
#32220 = VERTEX_POINT ( 'NONE', #35971 ) ;
#32221 = CARTESIAN_POINT ( 'NONE',  ( 117.6747548109119919, -1.834011780172310813, -8.268836392978581529 ) ) ;
#32222 = DIRECTION ( 'NONE',  ( 0.3445294493088594256, 0.9387755102040817867, 0.000000000000000000 ) ) ;
#32223 = CARTESIAN_POINT ( 'NONE',  ( 112.6356140045247827, -10.62599879583958717, -11.00651665394454604 ) ) ;
#32224 = CARTESIAN_POINT ( 'NONE',  ( 115.2355081442453155, -10.30919188438810075, -12.61870101168855918 ) ) ;
#32225 = CARTESIAN_POINT ( 'NONE',  ( 117.1074881442453233, -10.63000616557722466, -14.87417383870573495 ) ) ;
#32226 =( GEOMETRIC_REPRESENTATION_CONTEXT ( 3 ) GLOBAL_UNCERTAINTY_ASSIGNED_CONTEXT ( ( #956 ) ) GLOBAL_UNIT_ASSIGNED_CONTEXT ( ( #5660, #34594, #3378 ) ) REPRESENTATION_CONTEXT ( 'NONE', 'WORKASPACE' ) );
#32227 = CARTESIAN_POINT ( 'NONE',  ( 127.0298367773221315, -10.26141744229719954, -13.69217050928270929 ) ) ;
#32228 = LINE ( 'NONE', #17884, #12587 ) ;
#32229 = LINE ( 'NONE', #1001, #4437 ) ;
#32230 = EDGE_LOOP ( 'NONE', ( #25393, #32465 ) ) ;
#32231 = AXIS2_PLACEMENT_3D ( 'NONE', #40522, #12030, #25933 ) ;
#32232 = CARTESIAN_POINT ( 'NONE',  ( 116.1082702545247827, -10.62599879583958540, -15.77991374673208469 ) ) ;
#32233 = CARTESIAN_POINT ( 'NONE',  ( 109.2295226117709603, -5.526696438288506208, -18.58224487948997350 ) ) ;
#32234 = CARTESIAN_POINT ( 'NONE',  ( 121.1350814775786233, -9.859900752359378018, -12.68260735090039759 ) ) ;
#32235 = CARTESIAN_POINT ( 'NONE',  ( 63.22841645929758414, -12.65390981026857453, -10.35299945512634245 ) ) ;
#32236 = CARTESIAN_POINT ( 'NONE',  ( 122.5488326359456011, -1.179503403430467667, -17.05068175419387089 ) ) ;
#32237 = CARTESIAN_POINT ( 'NONE',  ( 113.9552233795247815, -1.325403438956436419, -9.854619843455211026 ) ) ;
#32238 = CARTESIAN_POINT ( 'NONE',  ( 126.2184548109105435, -4.159894987975746972, -8.443039665293909479 ) ) ;
#32239 = CARTESIAN_POINT ( 'NONE',  ( 112.9664414775786412, -9.859900752359374465, -12.68260735090039404 ) ) ;
#32240 = CYLINDRICAL_SURFACE ( 'NONE', #6601, 5.000000000000002665 ) ;
#32241 = CARTESIAN_POINT ( 'NONE',  ( 125.3328548109119964, -9.261995988541697145, -16.69588392320189030 ) ) ;
#32242 = CARTESIAN_POINT ( 'NONE',  ( 120.3409081442453044, -0.4660016031367893996, -10.09054647747474043 ) ) ;
#32243 = ORIENTED_EDGE ( 'NONE', *, *, #38937, .T. ) ;
#32244 = CARTESIAN_POINT ( 'NONE',  ( 119.4332814775786318, -8.899110576539710493, -16.42337572283490132 ) ) ;
#32245 = FACE_OUTER_BOUND ( 'NONE', #40521, .T. ) ;
#32246 = CARTESIAN_POINT ( 'NONE',  ( 119.5467348109119712, -4.089484607189486809, -7.948022111789456723 ) ) ;
#32247 = CARTESIAN_POINT ( 'NONE',  ( 119.3198281442452924, -9.859900752359374465, -12.68260735090039404 ) ) ;
#32248 = ORIENTED_EDGE ( 'NONE', *, *, #2756, .T. ) ;
#32249 = ADVANCED_FACE ( 'NONE', ( #871 ), #17664, .T. ) ;
#32250 = CARTESIAN_POINT ( 'NONE',  ( 124.1983214775786166, -1.833838273342659697, -17.42832698103878286 ) ) ;
#32251 = ADVANCED_FACE ( 'NONE', ( #35515 ), #35107, .T. ) ;
#32252 = CIRCLE ( 'NONE', #17709, 5.999999999999997335 ) ;
#32253 = CARTESIAN_POINT ( 'NONE',  ( 121.9292548109119849, -1.561330072975668948, -17.79121239304076951 ) ) ;
#32254 = DIRECTION ( 'NONE',  ( 0.9609149988134837450, -0.1028163501681639419, 0.2570431154366518145 ) ) ;
#32255 = CARTESIAN_POINT ( 'NONE',  ( 110.2047546295247855, -4.863998795839590272, -7.631215200338315796 ) ) ;
#32256 = DIRECTION ( 'NONE',  ( 0.000000000000000000, -1.000000000000000000, -1.195183497228115774E-16 ) ) ;
#32257 = CARTESIAN_POINT ( 'NONE',  ( 116.7329504682427768, 0.5115630086001619059, -14.64321520033831447 ) ) ;
#32258 = CARTESIAN_POINT ( 'NONE',  ( 111.6632702545248605, 0.1403307496149616695, -11.32035403202665336 ) ) ;
#32259 = AXIS2_PLACEMENT_3D ( 'NONE', #15897, #23189, #44173 ) ;
#32260 = CARTESIAN_POINT ( 'NONE',  ( 118.3554748109119998, 0.2603800115204892296, -16.42320221600525088 ) ) ;
#32261 = CARTESIAN_POINT ( 'NONE',  ( 137.3374356171263457, -9.844308156483171146, -11.96184393924012213 ) ) ;
#32262 = CARTESIAN_POINT ( 'NONE',  ( 117.2209414775786485, -2.084020599724406786, -8.691656652584148546 ) ) ;
#32263 = CARTESIAN_POINT ( 'NONE',  ( 126.2202699136542066, -0.8305752925518951058, -10.43662590553933889 ) ) ;
#32264 = CARTESIAN_POINT ( 'NONE',  ( 117.3343948109119737, -6.222761293078222344, -8.102969835052219238 ) ) ;
#32265 = CARTESIAN_POINT ( 'NONE',  ( 108.9545983795247821, -8.402594152722688392, -16.93181055722141792 ) ) ;
#32266 = CARTESIAN_POINT ( 'NONE',  ( 112.6260814775786514, -0.8288870151387760510, -10.36305467784173118 ) ) ;
#32267 = FILL_AREA_STYLE ('',( #10865 ) ) ;
#32268 = ADVANCED_FACE ( 'NONE', ( #19104 ), #29441, .T. ) ;
#32269 = CARTESIAN_POINT ( 'NONE',  ( 111.5883843147880725, -2.395992375830774179, -17.92872468182854462 ) ) ;
#32271 = CARTESIAN_POINT ( 'NONE',  ( 117.5613014775786525, 0.9020085738987339008, -11.91225656197089222 ) ) ;
#32270 = CARTESIAN_POINT ( 'NONE',  ( 65.71141733757100667, -16.34216531378293524, -9.991044251572791524 ) ) ;
#32272 = CARTESIAN_POINT ( 'NONE',  ( 118.5823814775786360, -7.643976991954077427, -18.09477374809248928 ) ) ;
#32273 = CARTESIAN_POINT ( 'NONE',  ( 112.5693548109119888, 0.4262465694468514643, -12.03445270309931736 ) ) ;
#32274 = ORIENTED_EDGE ( 'NONE', *, *, #18105, .T. ) ;
#32275 = CARTESIAN_POINT ( 'NONE',  ( 137.3802547664383269, -7.424459469978982540, -8.936682238071227857 ) ) ;
#32276 = CARTESIAN_POINT ( 'NONE',  ( 123.4041481442452834, -10.30919188438810075, -12.61870101168855918 ) ) ;
#32277 = CARTESIAN_POINT ( 'NONE',  ( 113.1217858795247935, -8.402594152722688392, -9.854619843455216355 ) ) ;
#32278 = CARTESIAN_POINT ( 'NONE',  ( 118.1285681442453068, -2.084020599724406786, -8.691656652584148546 ) ) ;
#32279 =( BOUNDED_CURVE ( )  B_SPLINE_CURVE ( 2, ( #33052, #3363, #1826, #3141, #15981, #43570, #29657, #23905, #43801, #12339, #22811, #45094, #29884, #40149, #36706 ),
 .UNSPECIFIED., .F., .T. ) 
 B_SPLINE_CURVE_WITH_KNOTS ( ( 3, 2, 2, 2, 2, 2, 2, 3 ),
 ( 0.7602707595410509445, 0.7812500000000000000, 0.8125000000000000000, 0.8437500000000000000, 0.8750000000000000000, 0.9062500000000000000, 0.9375000000000000000, 0.9667092643636859828 ),
 .UNSPECIFIED. ) 
 CURVE ( )  GEOMETRIC_REPRESENTATION_ITEM ( )  RATIONAL_B_SPLINE_CURVE ( ( 0.9664089390052280626, 0.9488976130786129781, 1.000000000000000000, 0.9238795325112869605, 1.000000000000000000, 0.9238795325112869605, 1.000000000000000000, 0.9238795325112869605, 1.000000000000000000, 0.9238795325112869605, 1.000000000000000000, 0.9238795325112869605, 1.000000000000000000, 0.9288504685323130117, 0.9907073674001189989 ) ) 
 REPRESENTATION_ITEM ( '' )  );
#32280 = EDGE_CURVE ( 'NONE', #523, #9906, #23502, .T. ) ;
#32282 = CARTESIAN_POINT ( 'NONE',  ( 115.8595014775786609, -7.643976991954077427, -18.09477374809248928 ) ) ;
#32281 = COLOUR_RGB ( '',0.7921568627450980005, 0.8196078431372548767, 0.9333333333333333481 ) ;
#32283 = EDGE_CURVE ( 'NONE', #34894, #44507, #11840, .T. ) ;
#32284 = CARTESIAN_POINT ( 'NONE',  ( 94.20708369096698220, -26.21217205256509075, -14.21600912764254687 ) ) ;
#32285 = CARTESIAN_POINT ( 'NONE',  ( 107.7044421295247929, 0.8980012041604618078, -13.39321520033831447 ) ) ;
#32286 = CARTESIAN_POINT ( 'NONE',  ( 122.6667014775786413, -2.084020599724406786, -8.691656652584148546 ) ) ;
#32287 = CIRCLE ( 'NONE', #18472, 4.999999999999999112 ) ;
#32288 = CARTESIAN_POINT ( 'NONE',  ( 124.5954081442453116, -6.222761293078241884, -8.102969835052219238 ) ) ;
#32289 = CARTESIAN_POINT ( 'NONE',  ( 115.9473434012278830, 0.04929351793716424401, -14.64321520033828961 ) ) ;
#32290 = CARTESIAN_POINT ( 'NONE',  ( 109.2294483239461016, -0.3417072992519313845, -10.56426903870459810 ) ) ;
#32291 = CARTESIAN_POINT ( 'NONE',  ( 121.2714235609119697, -9.645473719204776586, -14.86997237629376656 ) ) ;
#32292 = CARTESIAN_POINT ( 'NONE',  ( 106.7320983795247855, -8.402594152722688392, -16.93181055722141792 ) ) ;
#32293 = CARTESIAN_POINT ( 'NONE',  ( 117.1067020526858897, 1.586544940016389571, -21.37821035455269936 ) ) ;
#32294 = CARTESIAN_POINT ( 'NONE',  ( 83.47365629695968892, -32.82170496130314064, -21.84607615589008489 ) ) ;
#32295 = CARTESIAN_POINT ( 'NONE',  ( 116.0864081442453113, -9.988377603198976828, -10.36322818467138340 ) ) ;
#32296 = CARTESIAN_POINT ( 'NONE',  ( 120.0005481442453146, -5.638512984488999180, -18.83840828888717311 ) ) ;
#32297 = CARTESIAN_POINT ( 'NONE',  ( 111.2465515045248168, -2.477300249445798297, -7.631215200338321125 ) ) ;
#32298 = CARTESIAN_POINT ( 'NONE',  ( 112.5126281442453120, -10.30919188438810075, -12.61870101168855918 ) ) ;
#32299 = EDGE_LOOP ( 'NONE', ( #4176, #41956, #17192, #25635 ) ) ;
#32300 = DIRECTION ( 'NONE',  ( -0.000000000000000000, -0.9284778069183721172, -0.3713878862591650232 ) ) ;
#32301 = VECTOR ( 'NONE', #7880, 1000.000000000000000 ) ;
#32302 = CARTESIAN_POINT ( 'NONE',  ( 115.7460481442453357, 0.9020085738987339008, -11.91225656197089222 ) ) ;
#32303 = CARTESIAN_POINT ( 'NONE',  ( 123.4608748109119745, 0.4262465694468514643, -12.03445270309931736 ) ) ;
#32304 = EDGE_CURVE ( 'NONE', #11237, #31245, #20569, .T. ) ;
#32305 = CARTESIAN_POINT ( 'NONE',  ( 111.4348214775786801, -3.505236298600246325, -18.68346056562440793 ) ) ;
#32306 = CARTESIAN_POINT ( 'NONE',  ( 120.4543614775786295, -4.089484607189486809, -7.948022111789456723 ) ) ;
#32307 = ADVANCED_FACE ( 'NONE', ( #25540 ), #26384, .F. ) ;
#32308 = ADVANCED_FACE ( 'NONE', ( #8209 ), #4778, .T. ) ;
#32309 = CARTESIAN_POINT ( 'NONE',  ( 115.8304577545247582, -7.250697342233347165, -7.631215200338321125 ) ) ;
#32310 = CARTESIAN_POINT ( 'NONE',  ( 117.6747548109119919, -7.643976991954077427, -18.09477374809248928 ) ) ;
#32311 = CARTESIAN_POINT ( 'NONE',  ( 122.4521266859119635, -0.06289925094097943703, -9.412459353600674206 ) ) ;
#32312 = CARTESIAN_POINT ( 'NONE',  ( 88.46631044337289040, -25.23119213852205789, -15.24166438581092109 ) ) ;
#32313 = ORIENTED_EDGE ( 'NONE', *, *, #6940, .T. ) ;
#32314 = AXIS2_PLACEMENT_3D ( 'NONE', #10524, #24424, #34665 ) ;
#32315 = CARTESIAN_POINT ( 'NONE',  ( 122.3132204359119868, 1.345710702986147034, -13.97328579221134426 ) ) ;
#32316 = CARTESIAN_POINT ( 'NONE',  ( 119.8870948109119752, -9.261995988541697145, -16.69588392320189030 ) ) ;
#32317 = ORIENTED_EDGE ( 'NONE', *, *, #4709, .T. ) ;
#32318 = CARTESIAN_POINT ( 'NONE',  ( 122.4700493874820069, -6.063848558940142297, -18.38516058545102183 ) ) ;
#32319 = CARTESIAN_POINT ( 'NONE',  ( 64.37076103624345080, -2.792960894985629938, -8.058217223812896179 ) ) ;
#32320 = CARTESIAN_POINT ( 'NONE',  ( 122.0427081442452817, 0.5811942927096049871, -14.16772938898809286 ) ) ;
#32321 = CARTESIAN_POINT ( 'NONE',  ( 115.5191414775786569, -6.222761293078241884, -8.102969835052219238 ) ) ;
#32322 = CARTESIAN_POINT ( 'NONE',  ( 77.43858880758799046, -56.71620948281238839, -1.734724326163099350 ) ) ;
#32323 = CARTESIAN_POINT ( 'NONE',  ( 124.5144432999385913, -9.734490656202709147, -12.26242464252682396 ) ) ;
#32324 = CARTESIAN_POINT ( 'NONE',  ( 119.2063748109119814, -7.894159318335828068, -9.358103419637847864 ) ) ;
#32325 = DIRECTION ( 'NONE',  ( 1.000000000000000000, 0.000000000000000000, -0.000000000000000000 ) ) ;
#32326 = CARTESIAN_POINT ( 'NONE',  ( 122.4965214775786251, 0.1319031606808879209, -14.10382304977623669 ) ) ;
#32327 = CARTESIAN_POINT ( 'NONE',  ( 125.0211000582884537, -11.98805063819766303, -10.86686075357930470 ) ) ;
#32328 = CARTESIAN_POINT ( 'NONE',  ( 122.2696148109119889, -5.574606645277164318, -18.38911715685844683 ) ) ;
#32329 = CARTESIAN_POINT ( 'NONE',  ( 112.5126281442453120, -10.30919188438810075, -12.61870101168855918 ) ) ;
#32330 = CARTESIAN_POINT ( 'NONE',  ( 120.7947214775786193, -9.261995988541697145, -16.69588392320189030 ) ) ;
#32331 = CARTESIAN_POINT ( 'NONE',  ( 113.5337081442453240, -9.261995988541697145, -16.69588392320189030 ) ) ;
#32332 = CARTESIAN_POINT ( 'NONE',  ( 87.80477198183443477, -24.14644159042263993, -12.62951656296512937 ) ) ;
#32333 = CARTESIAN_POINT ( 'NONE',  ( 120.9081748109119872, -4.153390946401325223, -8.397313243818185668 ) ) ;
#32334 = ORIENTED_EDGE ( 'NONE', *, *, #26825, .F. ) ;
#32335 = CARTESIAN_POINT ( 'NONE',  ( 122.0994348109119443, 0.9020085738987339008, -11.91225656197089222 ) ) ;
#32336 = CARTESIAN_POINT ( 'NONE',  ( 111.5243640045248412, 0.1403307496149616695, -15.46607636864997204 ) ) ;
#32337 = DIRECTION ( 'NONE',  ( 1.000000000000000000, 0.000000000000000000, -0.000000000000000000 ) ) ;
#32338 = CARTESIAN_POINT ( 'NONE',  ( 121.9470836909669913, -25.99489077589524300, -13.39321520033831447 ) ) ;
#32339 = CARTESIAN_POINT ( 'NONE',  ( 119.9518141859119851, -0.8832429491016020595, -18.19431474523658565 ) ) ;
#32340 = CARTESIAN_POINT ( 'NONE',  ( 124.7088614775786226, 0.2603800115204892296, -16.42320221600525088 ) ) ;
#32341 = ORIENTED_EDGE ( 'NONE', *, *, #22250, .F. ) ;
#32342 = CARTESIAN_POINT ( 'NONE',  ( 123.4608748109119745, 0.4262465694468514643, -12.03445270309931736 ) ) ;
#32343 = CARTESIAN_POINT ( 'NONE',  ( 88.46631044337289040, -26.75858941326842810, -11.54476601486570964 ) ) ;
#32344 = CARTESIAN_POINT ( 'NONE',  ( 63.19915535949495222, -13.42640250087169385, -18.61752652045166911 ) ) ;
#32345 = EDGE_CURVE ( 'NONE', #25696, #4599, #4127, .T. ) ;
#32346 = FACE_OUTER_BOUND ( 'NONE', #15465, .T. ) ;
#32347 = CIRCLE ( 'NONE', #24360, 2.000000000000000444 ) ;
#32348 = CARTESIAN_POINT ( 'NONE',  ( 107.6349890045248401, -9.868328341294098749, -11.32035403202665869 ) ) ;
#32349 = ORIENTED_EDGE ( 'NONE', *, *, #34761, .F. ) ;
#32350 = CARTESIAN_POINT ( 'NONE',  ( 115.8027748109119841, -0.4660016031367893996, -10.09054647747474043 ) ) ;
#32351 = CARTESIAN_POINT ( 'NONE',  ( 125.8433948109119456, -1.834011780172310813, -8.268836392978581529 ) ) ;
#32352 = CARTESIAN_POINT ( 'NONE',  ( 120.6245414775786458, -0.1624402480850797581, -16.17319339645315424 ) ) ;
#32353 = CARTESIAN_POINT ( 'NONE',  ( 127.0066334552993084, -3.087553896376482143, -8.300037743346093677 ) ) ;
#32354 = SURFACE_STYLE_FILL_AREA ( #25975 ) ;
#32355 = CARTESIAN_POINT ( 'NONE',  ( 111.7184548109119788, -0.8288870151387760510, -10.36305467784173118 ) ) ;
#32356 = DIRECTION ( 'NONE',  ( 0.9908103287288504424, -0.1352586133457951423, 0.000000000000000000 ) ) ;
#32357 = CARTESIAN_POINT ( 'NONE',  ( 151.2860562277021472, -2.495269033102075262, -17.79652296963211455 ) ) ;
#32358 = CARTESIAN_POINT ( 'NONE',  ( 125.3895814775786448, -2.084020599724406786, -8.691656652584148546 ) ) ;
#32359 = VERTEX_POINT ( 'NONE', #32805 ) ;
#32360 = CARTESIAN_POINT ( 'NONE',  ( 115.8999108795247821, -1.325403438956436419, -16.93181055722141792 ) ) ;
#32361 = CARTESIAN_POINT ( 'NONE',  ( 121.5321681442453183, -9.988377603198976828, -10.36322818467138340 ) ) ;
#32362 =( BOUNDED_CURVE ( )  B_SPLINE_CURVE ( 2, ( #17860, #1416, #29244, #4840, #18759, #32649, #15335, #11694, #25604, #39508, #8270, #22174, #36069, #42121, #38670, #21584, #7669 ),
 .UNSPECIFIED., .F., .T. ) 
 B_SPLINE_CURVE_WITH_KNOTS ( ( 3, 2, 2, 2, 2, 2, 2, 2, 3 ),
 ( 0.3296282416568590001, 0.3359375000000000000, 0.3437500000000000000, 0.3515625000000000000, 0.3593750000000000000, 0.3671875000000000000, 0.3750000000000000000, 0.3828125000000000000, 0.3891217583431409999 ),
 .UNSPECIFIED. ) 
 CURVE ( )  GEOMETRIC_REPRESENTATION_ITEM ( )  RATIONAL_B_SPLINE_CURVE ( ( 0.9763430640195970289, 0.9385262470928680267, 1.000000000000000000, 0.9238795325112869605, 1.000000000000000000, 0.9238795325112869605, 1.000000000000000000, 0.9238795325112869605, 1.000000000000000000, 0.9238795325112869605, 1.000000000000000000, 0.9238795325112869605, 1.000000000000000000, 0.9238795325112869605, 1.000000000000000000, 0.9385262470928680267, 0.9763430640195970289 ) ) 
 REPRESENTATION_ITEM ( '' )  );
#32363 = CARTESIAN_POINT ( 'NONE',  ( 137.3930029278097891, -9.295380705929696674, -15.97142107135823430 ) ) ;
#32364 = EDGE_LOOP ( 'NONE', ( #11166, #35267, #20264, #3391, #6886 ) ) ;
#32365 = EDGE_CURVE ( 'NONE', #26037, #11292, #13320, .T. ) ;
#32366 = CARTESIAN_POINT ( 'NONE',  ( 112.7395348109119766, -4.153390946401321671, -8.397313243818183892 ) ) ;
#32367 = CARTESIAN_POINT ( 'NONE',  ( 127.0553483106875206, -4.550849702174990519, -18.80261012643152796 ) ) ;
#32368 = CARTESIAN_POINT ( 'NONE',  ( 124.8790414775786246, -8.899110576539710493, -16.42337572283490132 ) ) ;
#32369 = CIRCLE ( 'NONE', #41130, 2.999999999999999556 ) ;
#32370 = ORIENTED_EDGE ( 'NONE', *, *, #8425, .F. ) ;
#32371 = CARTESIAN_POINT ( 'NONE',  ( 119.4900081442453086, -1.834011780172310813, -8.268836392978581529 ) ) ;
#32372 = DIRECTION ( 'NONE',  ( 0.9999995469159186356, 0.0009519285464175526951, 0.000000000000000000 ) ) ;
#32373 = CARTESIAN_POINT ( 'NONE',  ( 79.49708691561605178, 5.079251341110372131, -20.33566263698374144 ) ) ;
#32374 = CARTESIAN_POINT ( 'NONE',  ( 125.4584548109119737, 2.768327990826033425, -17.42353644532102308 ) ) ;
#32375 = CIRCLE ( 'NONE', #7640, 1.587500000000000577 ) ;
#32376 = CARTESIAN_POINT ( 'NONE',  ( 124.8790414775786246, -0.4660016031367893996, -10.09054647747474043 ) ) ;
#32377 = DIRECTION ( 'NONE',  ( 0.000000000000000000, 0.000000000000000000, -1.000000000000000000 ) ) ;
#32378 = CYLINDRICAL_SURFACE ( 'NONE', #44146, 0.4999999999999996669 ) ;
#32379 = CARTESIAN_POINT ( 'NONE',  ( 126.0135748109119902, -8.166667518702819706, -8.995218007635861213 ) ) ;
#32380 = CARTESIAN_POINT ( 'NONE',  ( 124.5954081442453116, -6.222761293078241884, -8.102969835052219238 ) ) ;
#32381 = CARTESIAN_POINT ( 'NONE',  ( 116.6774435224926094, -8.419877142191296571, -17.02538347942430619 ) ) ;
#32382 = CARTESIAN_POINT ( 'NONE',  ( 123.5176014775786228, -0.8288870151387760510, -10.36305467784173118 ) ) ;
#32383 = FACE_OUTER_BOUND ( 'NONE', #26530, .T. ) ;
#32384 = CARTESIAN_POINT ( 'NONE',  ( 119.3765548109119834, 0.9020085738987339008, -11.91225656197089222 ) ) ;
#32385 = VERTEX_POINT ( 'NONE', #28740 ) ;
#32386 = CARTESIAN_POINT ( 'NONE',  ( 117.7873752477523794, -1.220279397241701647, -16.99638242193885418 ) ) ;
#32387 = CARTESIAN_POINT ( 'NONE',  ( 116.5944421295247793, 0.8980012041604618078, -13.39321520033831447 ) ) ;
#32388 = CARTESIAN_POINT ( 'NONE',  ( 115.9693640045247776, 0.1403307496149616695, -15.46607636864997204 ) ) ;
#32389 = CARTESIAN_POINT ( 'NONE',  ( 111.3854577545248645, -2.791137627527939813, -18.39754474579286025 ) ) ;
#32390 = CARTESIAN_POINT ( 'NONE',  ( 126.3230600034178650, -9.796589426897714503, -12.29887078920687493 ) ) ;
#32391 = CARTESIAN_POINT ( 'NONE',  ( 115.1220548109119761, -8.166667518702817929, -8.995218007635861213 ) ) ;
#32392 = ORIENTED_EDGE ( 'NONE', *, *, #5843, .F. ) ;
#32393 = CARTESIAN_POINT ( 'NONE',  ( 113.7038881442453402, -6.222761293078241884, -8.102969835052219238 ) ) ;
#32394 = CARTESIAN_POINT ( 'NONE',  ( 108.2600671295247992, -10.62599879583958540, -13.39321520033831447 ) ) ;
#32395 = CARTESIAN_POINT ( 'NONE',  ( 119.6392035773848761, -2.467220198592778413, -17.83387418641524391 ) ) ;
#32396 = CARTESIAN_POINT ( 'NONE',  ( 112.5126281442453120, 0.1319031606808879209, -14.10382304977623669 ) ) ;
#32397 = CARTESIAN_POINT ( 'NONE',  ( 122.8936081442453059, -9.565557343593390272, -10.61323700422343919 ) ) ;
#32398 = PLANE ( 'NONE',  #21386 ) ;
#32399 = CARTESIAN_POINT ( 'NONE',  ( 114.8384214775786489, 0.9020085738987339008, -11.91225656197089222 ) ) ;
#32400 = CARTESIAN_POINT ( 'NONE',  ( 112.4967077545247633, -7.250697342233347165, -7.631215200338321125 ) ) ;
#32401 = CARTESIAN_POINT ( 'NONE',  ( 110.9687390045248350, -9.868328341294098749, -11.32035403202665869 ) ) ;
#32402 = CIRCLE ( 'NONE', #6182, 2.999999999999999556 ) ;
#32403 = VERTEX_POINT ( 'NONE', #39447 ) ;
#32404 = CARTESIAN_POINT ( 'NONE',  ( 126.7702028005611368, -7.286025587178694529, -8.706033641032410841 ) ) ;
#32405 = CARTESIAN_POINT ( 'NONE',  ( 120.6245414775786458, -0.1624402480850797581, -16.17319339645315424 ) ) ;
#32406 = CARTESIAN_POINT ( 'NONE',  ( 114.7816948109119863, 0.5811942927096154232, -14.16772938898807155 ) ) ;
#32407 = CYLINDRICAL_SURFACE ( 'NONE', #43074, 3.000000000000001332 ) ;
#32408 = CARTESIAN_POINT ( 'NONE',  ( 117.9583881442453048, 0.1319031606808853119, -14.10382304977625800 ) ) ;
#32409 = CARTESIAN_POINT ( 'NONE',  ( 120.3409081442453044, -8.899110576539710493, -16.42337572283490132 ) ) ;
#32410 = CARTESIAN_POINT ( 'NONE',  ( 115.3489614775786407, -0.8288870151387760510, -10.36305467784173118 ) ) ;
#32411 = ORIENTED_EDGE ( 'NONE', *, *, #40657, .F. ) ;
#32412 = AXIS2_PLACEMENT_3D ( 'NONE', #37705, #38573, #24034 ) ;
#32413 = CARTESIAN_POINT ( 'NONE',  ( 120.3685329359119862, -4.283928203966213211, -7.183505701512925334 ) ) ;
#32414 = EDGE_CURVE ( 'NONE', #23460, #15244, #43315, .T. ) ;
#32415 = CARTESIAN_POINT ( 'NONE',  ( 121.4544569107182070, -2.467220198592778413, -17.83387418641524391 ) ) ;
#32416 = CARTESIAN_POINT ( 'NONE',  ( 119.3198281442452924, -9.859900752359374465, -12.68260735090039404 ) ) ;
#32417 = ORIENTED_EDGE ( 'NONE', *, *, #37255, .T. ) ;
#32418 = CARTESIAN_POINT ( 'NONE',  ( 124.1497896737536877, -8.611453504372539314, -17.77011218421760574 ) ) ;
#32419 = CARTESIAN_POINT ( 'NONE',  ( 116.3700414775786527, -5.638512984488999180, -18.83840828888717311 ) ) ;
#32420 = CARTESIAN_POINT ( 'NONE',  ( 115.4831921295247952, 0.8980012041604618078, -13.39321520033831447 ) ) ;
#32421 = CARTESIAN_POINT ( 'NONE',  ( 119.0690086830089882, -1.087735405160626723, -17.17288456429612964 ) ) ;
#32422 = VERTEX_POINT ( 'NONE', #4325 ) ;
#32423 = ORIENTED_EDGE ( 'NONE', *, *, #8269, .F. ) ;
#32424 = CARTESIAN_POINT ( 'NONE',  ( 123.1205148109119563, -7.643976991954077427, -18.09477374809248928 ) ) ;
#32425 = CARTESIAN_POINT ( 'NONE',  ( 115.9162281442453093, -5.574606645277164318, -18.38911715685844683 ) ) ;
#32426 = CARTESIAN_POINT ( 'NONE',  ( 124.5571602873148294, -9.865299344075070920, -13.45945633590898538 ) ) ;
#32427 = CARTESIAN_POINT ( 'NONE',  ( 126.2184548109119788, -4.863998795839242995, -13.39321520033831447 ) ) ;
#32428 = ORIENTED_EDGE ( 'NONE', *, *, #39772, .F. ) ;
#32429 = CARTESIAN_POINT ( 'NONE',  ( 112.1489877442403298, -8.920892194852200419, -16.35787768542246923 ) ) ;
#32430 = CARTESIAN_POINT ( 'NONE',  ( 61.99939684703689124, -65.50319228955336825, -44.43454011388369906 ) ) ;
#32431 = CARTESIAN_POINT ( 'NONE',  ( 110.7603796295247918, -4.863998795839590272, -19.15521520033831493 ) ) ;
#32432 = EDGE_CURVE ( 'NONE', #24584, #31011, #38035, .T. ) ;
#32433 = CARTESIAN_POINT ( 'NONE',  ( 112.2289948109119848, -1.834011780172310813, -8.268836392978581529 ) ) ;
#32434 = CARTESIAN_POINT ( 'NONE',  ( 126.6942948109119840, -8.899110576539710493, -16.42337572283490132 ) ) ;
#32435 = CARTESIAN_POINT ( 'NONE',  ( 120.9081748109119872, -4.153390946401325223, -8.397313243818185668 ) ) ;
#32436 = LINE ( 'NONE', #32211, #37841 ) ;
#32437 = ORIENTED_EDGE ( 'NONE', *, *, #35385, .F. ) ;
#32438 = AXIS2_PLACEMENT_3D ( 'NONE', #3278, #44346, #16755 ) ;
#32439 = CARTESIAN_POINT ( 'NONE',  ( 118.2420214775786320, -6.222761293078241884, -8.102969835052219238 ) ) ;
#32440 = DIRECTION ( 'NONE',  ( -0.2768435750659241079, -0.3568721902840695792, 0.8921882507333129819 ) ) ;
#32441 = CARTESIAN_POINT ( 'NONE',  ( 113.9264514740559520, -1.081026697600511843, -17.18181821144401056 ) ) ;
#32442 = CARTESIAN_POINT ( 'NONE',  ( 114.5803015045248117, -2.477300249445798297, -7.631215200338321125 ) ) ;
#32443 = CARTESIAN_POINT ( 'NONE',  ( 118.6958348109119754, -6.344957434206665248, -7.627207830600338134 ) ) ;
#32444 = EDGE_LOOP ( 'NONE', ( #24552, #11658, #38988, #4640 ) ) ;
#32445 = CARTESIAN_POINT ( 'NONE',  ( 115.4624148109119943, -5.638512984488999180, -18.83840828888717311 ) ) ;
#32446 = DIRECTION ( 'NONE',  ( -0.8636456077245080465, 0.5040994586965603652, 0.000000000000000000 ) ) ;
#32447 = CARTESIAN_POINT ( 'NONE',  ( 106.5931921295248372, 0.8980012041604618078, -13.39321520033831447 ) ) ;
#32448 = CARTESIAN_POINT ( 'NONE',  ( 117.4478481442453131, 0.2603800115204892296, -16.42320221600525088 ) ) ;
#32449 = CARTESIAN_POINT ( 'NONE',  ( 117.5045748109119756, 0.5811942927096110934, -14.16772938898807510 ) ) ;
#32450 = CARTESIAN_POINT ( 'NONE',  ( 127.0915067942372190, -10.29034310956583731, -13.72608135453547185 ) ) ;
#32451 = CARTESIAN_POINT ( 'NONE',  ( 120.8456493241987317, -6.333924026435813204, -18.89660969823682279 ) ) ;
#32452 = CARTESIAN_POINT ( 'NONE',  ( 105.5513952545248060, -9.868328341294098749, -15.46607636864997204 ) ) ;
#32453 = ORIENTED_EDGE ( 'NONE', *, *, #28576, .T. ) ;
#32454 = CARTESIAN_POINT ( 'NONE',  ( 116.5043621053768703, 0.3967854368539331933, -16.28112951403851838 ) ) ;
#32455 = CARTESIAN_POINT ( 'NONE',  ( 109.2295493080124231, -10.35223054996752623, -12.16705481747161599 ) ) ;
#32456 = CARTESIAN_POINT ( 'NONE',  ( 121.7023481442452919, -0.8288870151387760510, -10.36305467784173118 ) ) ;
#32457 = AXIS2_PLACEMENT_3D ( 'NONE', #12682, #15871, #16091 ) ;
#32458 = CARTESIAN_POINT ( 'NONE',  ( 112.6356140045247827, 0.1403307496149616695, -15.46607636864997204 ) ) ;
#32459 = CARTESIAN_POINT ( 'NONE',  ( 113.6079577545248043, -2.791137627527939813, -18.39754474579286025 ) ) ;
#32460 = CARTESIAN_POINT ( 'NONE',  ( 113.8740681442453138, -9.859900752359374465, -12.68260735090039404 ) ) ;
#32461 = CARTESIAN_POINT ( 'NONE',  ( 113.1933481442453058, -5.574606645277164318, -18.38911715685844683 ) ) ;
#32462 = DIRECTION ( 'NONE',  ( 0.000000000000000000, 0.000000000000000000, 1.000000000000000000 ) ) ;
#32463 = CARTESIAN_POINT ( 'NONE',  ( 123.9146881442452894, 0.9020085738987339008, -11.91225656197089222 ) ) ;
#32464 = CARTESIAN_POINT ( 'NONE',  ( 119.7736414775786358, -10.30919188438810075, -12.61870101168855918 ) ) ;
#32465 = ORIENTED_EDGE ( 'NONE', *, *, #26305, .T. ) ;
#32466 = CARTESIAN_POINT ( 'NONE',  ( 119.3198281442452924, -9.859900752359374465, -12.68260735090039404 ) ) ;
#32467 = CARTESIAN_POINT ( 'NONE',  ( 112.5693548109119888, -10.63000616557722466, -14.87417383870573495 ) ) ;
#32468 = CARTESIAN_POINT ( 'NONE',  ( 120.0572748109119772, -3.383040157471821630, -19.15922257007629170 ) ) ;
#32469 = CARTESIAN_POINT ( 'NONE',  ( 120.6245414775786458, -0.1624402480850797581, -16.17319339645315424 ) ) ;
#32470 = ORIENTED_EDGE ( 'NONE', *, *, #23388, .T. ) ;
#32471 = CARTESIAN_POINT ( 'NONE',  ( 124.5386814775786206, -4.153390946401325223, -8.397313243818185668 ) ) ;
#32472 = AXIS2_PLACEMENT_3D ( 'NONE', #18466, #28279, #14817 ) ;
#32473 = CARTESIAN_POINT ( 'NONE',  ( 119.7169148109119874, -9.988377603198976828, -10.36322818467138340 ) ) ;
#32474 = AXIS2_PLACEMENT_3D ( 'NONE', #25530, #38513, #35995 ) ;
#32475 = CARTESIAN_POINT ( 'NONE',  ( 112.8529881442453302, -7.894159318335828068, -9.358103419637847864 ) ) ;
#32476 = CARTESIAN_POINT ( 'NONE',  ( 69.36136150295220659, -58.33016572499207797, -33.43006446620090344 ) ) ;
#32477 = DIRECTION ( 'NONE',  ( 0.000000000000000000, 0.000000000000000000, 1.000000000000000000 ) ) ;
#32478 = CARTESIAN_POINT ( 'NONE',  ( 115.6915515045247531, -6.936859964151250502, -18.39754474579286025 ) ) ;
#32479 = CARTESIAN_POINT ( 'NONE',  ( 119.8870948109119752, -9.261995988541697145, -16.69588392320189030 ) ) ;
#32480 = AXIS2_PLACEMENT_3D ( 'NONE', #33567, #19236, #19005 ) ;
#32481 = CARTESIAN_POINT ( 'NONE',  ( 137.4478226697652303, -9.800447051581507196, -12.23758396775345858 ) ) ;
#32482 = CARTESIAN_POINT ( 'NONE',  ( 114.3278814775786429, 0.1319031606808879209, -14.10382304977623669 ) ) ;
#32483 = CARTESIAN_POINT ( 'NONE',  ( 112.0020881442453344, -9.565557343593413364, -10.61323700422348004 ) ) ;
#32484 = CARTESIAN_POINT ( 'NONE',  ( 126.2940345447988761, -0.6470042893710473697, -10.63705365171230355 ) ) ;
#32485 = CARTESIAN_POINT ( 'NONE',  ( -12.73765092793578191, -4.237858357736757675, -7.430846270786123142 ) ) ;
#32486 = CARTESIAN_POINT ( 'NONE',  ( 111.5243640045248412, 0.1403307496149616695, -15.46607636864997204 ) ) ;
#32487 = CARTESIAN_POINT ( 'NONE',  ( 122.0274825628256963, -2.263366209404226392, -18.10533625161308180 ) ) ;
#32488 = DIRECTION ( 'NONE',  ( 0.7071067811865520136, 0.000000000000000000, -0.7071067811865431318 ) ) ;
#32489 = CARTESIAN_POINT ( 'NONE',  ( 68.56885555382550024, -20.41671115022302274, -14.39321520033831625 ) ) ;
#32491 = CARTESIAN_POINT ( 'NONE',  ( 120.7379948109119709, -10.63000616557722466, -14.87417383870573495 ) ) ;
#32490 = CARTESIAN_POINT ( 'NONE',  ( 60.11760374155739584, -14.70486118635414385, -7.429569208445769846 ) ) ;
#32492 = CARTESIAN_POINT ( 'NONE',  ( 119.6034614775786196, -3.505236298600246325, -18.68346056562440793 ) ) ;
#32493 = CARTESIAN_POINT ( 'NONE',  ( 114.2711548109119803, -0.1624402480850797581, -16.17319339645315424 ) ) ;
#32494 = ORIENTED_EDGE ( 'NONE', *, *, #24246, .F. ) ;
#32495 = DIRECTION ( 'NONE',  ( -0.000000000000000000, -0.9284778069183721172, -0.3713878862591650232 ) ) ;
#32496 = CARTESIAN_POINT ( 'NONE',  ( 125.7866681442452688, -0.4660016031367893996, -10.09054647747474043 ) ) ;
#32497 = CARTESIAN_POINT ( 'NONE',  ( 116.6638952545248031, -9.868328341294098749, -15.46607636864997204 ) ) ;
#32498 = CARTESIAN_POINT ( 'NONE',  ( 118.4689281442453392, -10.15424416112533912, -14.75197769757731336 ) ) ;
#32499 = EDGE_CURVE ( 'NONE', #43873, #34005, #38846, .T. ) ;
#32500 = CARTESIAN_POINT ( 'NONE',  ( 119.9438214775786378, -2.084020599724406786, -8.691656652584148546 ) ) ;
#32501 = CARTESIAN_POINT ( 'NONE',  ( 115.8027748109119841, -8.899110576539710493, -16.42337572283490132 ) ) ;
#32502 = CARTESIAN_POINT ( 'NONE',  ( 85.78840348512180469, -27.74674259770401719, -8.784702801739287636 ) ) ;
#32503 = CARTESIAN_POINT ( 'NONE',  ( 109.7185827545247889, -2.477300249445798297, -19.15521520033831138 ) ) ;
#32504 = CARTESIAN_POINT ( 'NONE',  ( 124.9357681442453014, -7.643976991954077427, -18.09477374809248928 ) ) ;
#32505 = CARTESIAN_POINT ( 'NONE',  ( 124.4252281442452812, -0.8288870151387760510, -10.36305467784173118 ) ) ;
#32506 = FACE_OUTER_BOUND ( 'NONE', #1130, .T. ) ;
#32507 = CARTESIAN_POINT ( 'NONE',  ( -13.55920938158181599, -4.791027969838746792, -8.800393969189304499 ) ) ;
#32508 = CARTESIAN_POINT ( 'NONE',  ( 120.1601735609119856, -9.645473719204776586, -14.86997237629376656 ) ) ;
#32509 = CARTESIAN_POINT ( 'NONE',  ( 114.3719421295247827, 0.8980012041604618078, -13.39321520033831447 ) ) ;
#32510 = CARTESIAN_POINT ( 'NONE',  ( 117.2294421295247844, 1.035107641088057973, -4.893215200338314474 ) ) ;
#32511 = CARTESIAN_POINT ( 'NONE',  ( 82.44760263944102974, -31.73904833139433279, -23.17969760592469441 ) ) ;
#32512 = CARTESIAN_POINT ( 'NONE',  ( 117.1074881442453233, -10.63000616557722466, -14.87417383870573495 ) ) ;
#32513 = CARTESIAN_POINT ( 'NONE',  ( 117.2776681442452968, -5.638512984488999180, -18.83840828888717311 ) ) ;
#32514 = DIRECTION ( 'NONE',  ( 1.000000000000000000, 0.000000000000000000, 0.000000000000000000 ) ) ;
#32515 = CARTESIAN_POINT ( 'NONE',  ( 111.8886348109120092, -3.383040157471821630, -19.15922257007629170 ) ) ;
#32516 = CARTESIAN_POINT ( 'NONE',  ( 73.53114257624162065, -54.10809544429395856, -7.393215200338315363 ) ) ;
#32517 = ORIENTED_EDGE ( 'NONE', *, *, #37552, .F. ) ;
#32518 = CARTESIAN_POINT ( 'NONE',  ( 74.66232006577804725, -2.500611837642884527, -7.993215200338315007 ) ) ;
#32519 = CARTESIAN_POINT ( 'NONE',  ( 118.0718414775786300, -9.261995988541697145, -16.69588392320189030 ) ) ;
#32520 = CARTESIAN_POINT ( 'NONE',  ( 122.4397948109119767, -0.1624402480850797581, -16.17319339645315424 ) ) ;
#32521 = CARTESIAN_POINT ( 'NONE',  ( 0.000000000000000000, 0.000000000000000000, 0.000000000000000000 ) ) ;
#32522 = CARTESIAN_POINT ( 'NONE',  ( 113.9875214775786532, -8.899110576539710493, -16.42337572283490132 ) ) ;
#32523 = CARTESIAN_POINT ( 'NONE',  ( 122.5532481442453019, -10.63000616557722466, -14.87417383870573495 ) ) ;
#32524 = EDGE_CURVE ( 'NONE', #735, #44542, #32197, .T. ) ;
#32525 = AXIS2_PLACEMENT_3D ( 'NONE', #33391, #43914, #29096 ) ;
#32526 = CARTESIAN_POINT ( 'NONE',  ( 114.3024890045248156, 0.8980012041604421569, -15.77991374673208469 ) ) ;
#32527 = CARTESIAN_POINT ( 'NONE',  ( 116.7104014775786425, -8.899110576539710493, -16.42337572283490132 ) ) ;
#32528 = CARTESIAN_POINT ( 'NONE',  ( 116.7904600221807669, -3.161398967842792285, -18.30238421764784462 ) ) ;
#32529 = DIRECTION ( 'NONE',  ( 0.9609149988134837450, -0.1028163501681639419, 0.2570431154366518145 ) ) ;
#32530 = VERTEX_POINT ( 'NONE', #5898 ) ;
#32531 = EDGE_CURVE ( 'NONE', #27501, #17020, #5288, .T. ) ;
#32532 = CIRCLE ( 'NONE', #36918, 2.445500000000004448 ) ;
#32533 = CARTESIAN_POINT ( 'NONE',  ( 120.7157985609119635, -0.08252387247370887580, -11.91645802438286417 ) ) ;
#32534 = EDGE_CURVE ( 'NONE', #42200, #16463, #11124, .T. ) ;
#32535 = CARTESIAN_POINT ( 'NONE',  ( 120.6812681442452941, -10.30919188438810075, -12.61870101168855918 ) ) ;
#32536 = VERTEX_POINT ( 'NONE', #41039 ) ;
#32537 = FACE_BOUND ( 'NONE', #21945, .T. ) ;
#32538 = CARTESIAN_POINT ( 'NONE',  ( 89.12784890491134604, -26.75858941326842810, -11.54476601486570964 ) ) ;
#32539 = CYLINDRICAL_SURFACE ( 'NONE', #12185, 3.000000000000001776 ) ;
#32540 = CARTESIAN_POINT ( 'NONE',  ( 115.9729548109119861, -3.505236298600246325, -18.68346056562440793 ) ) ;
#32541 = CARTESIAN_POINT ( 'NONE',  ( 124.5252192005878698, -9.794068186057833358, -12.55818921246619624 ) ) ;
#32542 =( BOUNDED_SURFACE ( )  B_SPLINE_SURFACE ( 1, 2, ( 
 ( #34330, #6301, #16575, #38578, #39043, #7814, #20446, #28569, #42252, #42031, #34106, #3103, #17030, #42478, #23641, #2643, #3932, #518, #2874, #17852, #14430, #13153, #27056, #16804, #44618, #13384, #41202, #9961, #43368, #8707, #8035, #15104, #43142, #32640, #11912, #18526, #12365, #18298, #32193, #39721, #18750, #25374, #22612, #4383, #39498, #29235, #28794, #25812, #8486, #14882, #33077, #15326, #19200, #15548, #1408, #1849, #29453, #1192, #12137, #26039, #21940, #39945, #8261, #22390, #35832, #15778, #36286, #966, #26265, #5054, #42700, #36510, #11470, #5284, #29680, #18969, #36060, #4829, #4606, #22165, #39272, #32858, #32419, #29014, #42924, #11687, #25593, #43592, #1628, #40172, #21722, #35609, #37650, #16236, #44503, #37179, #16004, #40403, #9384, #26496, #36731, #44286, #13494, #27399, #12820, #9851, #2766, #5952, #9164, #44053, #26718, #16690, #43826, #30582, #23294, #20109, #29912, #40862, #40627, #13266, #9615, #20335, #12592, #5723, #19876, #27172, #33765, #41093, #2533, #16917, #5497, #8936, #16460, #23068, #30811, #6189, #33995, #23760, #37420, #13039, #2991, #6425, #34218, #30364, #22840, #44735, #30139, #19418, #33304, #26938, #36952, #2306, #19641, #33528, #23534, #2080, #38521, #27623, #14375, #35093, #24863, #3441, #31691, #24416, #3215, #41537, #41755, #13716, #23983, #31468, #680, #14598, #20, #42197, #3876, #38307, #10300, #31248, #13933, #17798, #31028, #460, #10515, #7299, #17141, #28065, #27845, #28288, #41975, #7524, #44959, #38092, #7084, #10958, #20993, #38754, #34867, #4095, #37871, #41321, #3655, #24201, #18017, #21218, #21440, #35325, #24639, #240, #31915, #10080, #6647, #17576, #20555, #34436, #17360, #6868, #20776, #34656, #14150, #10740, #12082, #18911, #39446, #18477, #4998, #15495, #14829, #21886, #4776, #8207, #18697, #25321, #19140, #25090, #38984, #1355, #25539, #32141, #29402, #11187, #1132, #36005, #35552, #32586, #15268, #21664, #39893, #22115, #25988, #22338, #29176, #8654, #36233, #7978, #32804, #1574, #28739 ),
 ( #1797, #35782, #908, #43088, #28962, #11856, #25763, #39669, #4550, #8432, #43314, #7756, #22555, #36455, #42870, #4324, #18245, #5226, #33023, #15051, #28518, #42423, #11627, #42643, #11412, #39214, #32366, #40573, #43541, #8879, #16403, #30302, #26436, #15724, #33254, #33935, #15951, #40345, #19820, #26884, #23242, #12311, #5897, #29854, #37361, #36675, #23475, #44228, #19365, #43769, #36900, #43996, #37123, #26208, #40115, #2706, #29626, #16633, #22780, #5671, #40803, #30527, #19589, #5445, #6133, #20052, #33470, #2026, #12535, #9106, #23008, #2250, #2478, #16179, #33706, #30082, #12760, #26659, #9333, #12988, #9559, #36640, #2208, #29365, #26170, #32764, #30038, #11816, #1760, #5413, #36195, #19329, #33215, #22298, #40535, #22738, #26621, #22971, #40075, #9296, #36861, #8620, #5631, #19551, #15459, #33429, #15686, #1989, #43276, #23204, #15915, #39631, #19779, #8839, #25724, #16137, #8394, #43955, #12718, #29813, #43506, #12274, #12045, #29588, #4959, #43729, #1537, #22517, #25948, #39855, #36414, #37082, #26395, #5182, #5857, #33661, #2438, #19099, #29137, #12497, #32986, #43049, #18873, #40305, #9069, #37776, #27306, #6549, #13175, #12951, #23893, #34566, #16596, #13404, #20007, #17269, #44189, #34126, #20466, #23434, #34347, #3125, #9516, #27754, #9981, #13838, #10203, #41223, #41669, #24111, #40998, #38005, #6779, #2663, #20689, #2896, #17049, #30489, #10426, #30942, #26847, #6997, #44865, #40760, #3350, #37318, #31160, #45079, #13621, #30718, #44640, #44409, #16825, #6089, #27530, #33893, #9752, #27077, #23663, #37550, #24334, #41445, #6322, #38218, #20909, #34783, #20240, #16361, #30263, #10645, #34994, #4004, #21120, #31376, #38886, #8727, #22633, #7424, #5073, #43167, #595, #3778, #38655, #21345, #11936, #38437, #25832, #17926, #15349, #24550, #36083, #35229, #39740, #4854, #15572, #7207, #371, #14505, #8508, #28418, #22412, #42329, #12158, #147, #3566, #11090, #17702, #26061, #1429, #29257, #36305, #32661, #8284, #43391, #18990, #32878, #31825 ) ),
 .UNSPECIFIED., .F., .F., .T. ) 
 B_SPLINE_SURFACE_WITH_KNOTS ( ( 2, 2 ),
 ( 3, 2, 2, 2, 2, 2, 2, 2, 2, 2, 2, 2, 2, 2, 2, 2, 2, 2, 2, 2, 2, 2, 2, 2, 2, 2, 2, 2, 2, 2, 2, 2, 2, 2, 2, 2, 2, 2, 2, 2, 2, 2, 2, 2, 2, 2, 2, 2, 2, 2, 2, 2, 2, 2, 2, 2, 2, 2, 2, 2, 2, 2, 2, 2, 2, 2, 2, 2, 2, 2, 2, 2, 2, 2, 2, 2, 2, 2, 2, 2, 2, 2, 2, 2, 2, 2, 2, 2, 2, 2, 2, 2, 2, 2, 2, 2, 2, 2, 2, 2, 2, 2, 2, 2, 2, 2, 2, 2, 2, 2, 2, 2, 2, 2, 2, 2, 2, 2, 2, 2, 2, 2, 2, 2, 2, 2, 2, 2, 3 ),
 ( 0.000000000000000000, 1.000000000000000000 ),
 ( 0.000000000000000000, 0.007812500000000000000, 0.01562500000000000000, 0.02343750000000000000, 0.03125000000000000000, 0.03906250000000000000, 0.04687500000000000000, 0.05468750000000000000, 0.06250000000000000000, 0.07031250000000000000, 0.07812500000000000000, 0.08593750000000000000, 0.09375000000000000000, 0.1015625000000000000, 0.1093750000000000000, 0.1171875000000000000, 0.1250000000000000000, 0.1328125000000000000, 0.1406250000000000000, 0.1484375000000000000, 0.1562500000000000000, 0.1640625000000000000, 0.1718750000000000000, 0.1796875000000000000, 0.1875000000000000000, 0.1953125000000000000, 0.2031250000000000000, 0.2109375000000000000, 0.2187500000000000000, 0.2265625000000000000, 0.2343750000000000000, 0.2421875000000000000, 0.2500000000000000000, 0.2578125000000000000, 0.2656250000000000000, 0.2734375000000000000, 0.2812500000000000000, 0.2890625000000000000, 0.2968750000000000000, 0.3046875000000000000, 0.3125000000000000000, 0.3203125000000000000, 0.3281250000000000000, 0.3359375000000000000, 0.3437500000000000000, 0.3515625000000000000, 0.3593750000000000000, 0.3671875000000000000, 0.3750000000000000000, 0.3828125000000000000, 0.3906250000000000000, 0.3984375000000000000, 0.4062500000000000000, 0.4140625000000000000, 0.4218750000000000000, 0.4296875000000000000, 0.4375000000000000000, 0.4453125000000000000, 0.4531250000000000000, 0.4609375000000000000, 0.4687500000000000000, 0.4765625000000000000, 0.4843750000000000000, 0.4921875000000000000, 0.5000000000000000000, 0.5078125000000000000, 0.5156250000000000000, 0.5234375000000000000, 0.5312500000000000000, 0.5390625000000000000, 0.5468750000000000000, 0.5546875000000000000, 0.5625000000000000000, 0.5703125000000000000, 0.5781250000000000000, 0.5859375000000000000, 0.5937500000000000000, 0.6015625000000000000, 0.6093750000000000000, 0.6171875000000000000, 0.6250000000000000000, 0.6328125000000000000, 0.6406250000000000000, 0.6484375000000000000, 0.6562500000000000000, 0.6640625000000000000, 0.6718750000000000000, 0.6796875000000000000, 0.6875000000000000000, 0.6953125000000000000, 0.7031250000000000000, 0.7109375000000000000, 0.7187500000000000000, 0.7265625000000000000, 0.7343750000000000000, 0.7421875000000000000, 0.7500000000000000000, 0.7578125000000000000, 0.7656250000000000000, 0.7734375000000000000, 0.7812500000000000000, 0.7890625000000000000, 0.7968750000000000000, 0.8046875000000000000, 0.8125000000000000000, 0.8203125000000000000, 0.8281250000000000000, 0.8359375000000000000, 0.8437500000000000000, 0.8515625000000000000, 0.8593750000000000000, 0.8671875000000000000, 0.8750000000000000000, 0.8828125000000000000, 0.8906250000000000000, 0.8984375000000000000, 0.9062500000000000000, 0.9140625000000000000, 0.9218750000000000000, 0.9296875000000000000, 0.9375000000000000000, 0.9453125000000000000, 0.9531250000000000000, 0.9609375000000000000, 0.9687500000000000000, 0.9765625000000000000, 0.9843750000000000000, 0.9921875000000000000, 1.000000000000000000 ),
 .UNSPECIFIED. ) 
 GEOMETRIC_REPRESENTATION_ITEM ( )  RATIONAL_B_SPLINE_SURFACE ( (
 ( 1.000000000000000000, 0.9238795325112869605, 1.000000000000000000, 0.9238795325112869605, 1.000000000000000000, 0.9238795325112869605, 1.000000000000000000, 0.9238795325112869605, 1.000000000000000000, 0.9238795325112869605, 1.000000000000000000, 0.9238795325112869605, 1.000000000000000000, 0.9238795325112869605, 1.000000000000000000, 0.9238795325112869605, 1.000000000000000000, 0.9238795325112869605, 1.000000000000000000, 0.9238795325112869605, 1.000000000000000000, 0.9238795325112869605, 1.000000000000000000, 0.9238795325112869605, 1.000000000000000000, 0.9238795325112869605, 1.000000000000000000, 0.9238795325112869605, 1.000000000000000000, 0.9238795325112869605, 1.000000000000000000, 0.9238795325112869605, 1.000000000000000000, 0.9238795325112869605, 1.000000000000000000, 0.9238795325112869605, 1.000000000000000000, 0.9238795325112869605, 1.000000000000000000, 0.9238795325112869605, 1.000000000000000000, 0.9238795325112869605, 1.000000000000000000, 0.9238795325112869605, 1.000000000000000000, 0.9238795325112869605, 1.000000000000000000, 0.9238795325112869605, 1.000000000000000000, 0.9238795325112869605, 1.000000000000000000, 0.9238795325112869605, 1.000000000000000000, 0.9238795325112869605, 1.000000000000000000, 0.9238795325112869605, 1.000000000000000000, 0.9238795325112869605, 1.000000000000000000, 0.9238795325112869605, 1.000000000000000000, 0.9238795325112869605, 1.000000000000000000, 0.9238795325112869605, 1.000000000000000000, 0.9238795325112869605, 1.000000000000000000, 0.9238795325112869605, 1.000000000000000000, 0.9238795325112869605, 1.000000000000000000, 0.9238795325112869605, 1.000000000000000000, 0.9238795325112869605, 1.000000000000000000, 0.9238795325112869605, 1.000000000000000000, 0.9238795325112869605, 1.000000000000000000, 0.9238795325112869605, 1.000000000000000000, 0.9238795325112869605, 1.000000000000000000, 0.9238795325112869605, 1.000000000000000000, 0.9238795325112869605, 1.000000000000000000, 0.9238795325112869605, 1.000000000000000000, 0.9238795325112869605, 1.000000000000000000, 0.9238795325112869605, 1.000000000000000000, 0.9238795325112869605, 1.000000000000000000, 0.9238795325112869605, 1.000000000000000000, 0.9238795325112869605, 1.000000000000000000, 0.9238795325112869605, 1.000000000000000000, 0.9238795325112869605, 1.000000000000000000, 0.9238795325112869605, 1.000000000000000000, 0.9238795325112869605, 1.000000000000000000, 0.9238795325112869605, 1.000000000000000000, 0.9238795325112869605, 1.000000000000000000, 0.9238795325112869605, 1.000000000000000000, 0.9238795325112869605, 1.000000000000000000, 0.9238795325112869605, 1.000000000000000000, 0.9238795325112869605, 1.000000000000000000, 0.9238795325112869605, 1.000000000000000000, 0.9238795325112869605, 1.000000000000000000, 0.9238795325112869605, 1.000000000000000000, 0.9238795325112869605, 1.000000000000000000, 0.9238795325112869605, 1.000000000000000000, 0.9238795325112869605, 1.000000000000000000, 0.9238795325112869605, 1.000000000000000000, 0.9238795325112869605, 1.000000000000000000, 0.9238795325112869605, 1.000000000000000000, 0.9238795325112869605, 1.000000000000000000, 0.9238795325112869605, 1.000000000000000000, 0.9238795325112869605, 1.000000000000000000, 0.9238795325112869605, 1.000000000000000000, 0.9238795325112869605, 1.000000000000000000, 0.9238795325112869605, 1.000000000000000000, 0.9238795325112869605, 1.000000000000000000, 0.9238795325112869605, 1.000000000000000000, 0.9238795325112869605, 1.000000000000000000, 0.9238795325112869605, 1.000000000000000000, 0.9238795325112869605, 1.000000000000000000, 0.9238795325112869605, 1.000000000000000000, 0.9238795325112869605, 1.000000000000000000, 0.9238795325112869605, 1.000000000000000000, 0.9238795325112869605, 1.000000000000000000, 0.9238795325112869605, 1.000000000000000000, 0.9238795325112869605, 1.000000000000000000, 0.9238795325112869605, 1.000000000000000000, 0.9238795325112869605, 1.000000000000000000, 0.9238795325112869605, 1.000000000000000000, 0.9238795325112869605, 1.000000000000000000, 0.9238795325112869605, 1.000000000000000000, 0.9238795325112869605, 1.000000000000000000, 0.9238795325112869605, 1.000000000000000000, 0.9238795325112869605, 1.000000000000000000, 0.9238795325112869605, 1.000000000000000000, 0.9238795325112869605, 1.000000000000000000, 0.9238795325112869605, 1.000000000000000000, 0.9238795325112869605, 1.000000000000000000, 0.9238795325112869605, 1.000000000000000000, 0.9238795325112869605, 1.000000000000000000, 0.9238795325112869605, 1.000000000000000000, 0.9238795325112869605, 1.000000000000000000, 0.9238795325112869605, 1.000000000000000000, 0.9238795325112869605, 1.000000000000000000, 0.9238795325112869605, 1.000000000000000000, 0.9238795325112869605, 1.000000000000000000, 0.9238795325112869605, 1.000000000000000000, 0.9238795325112869605, 1.000000000000000000, 0.9238795325112869605, 1.000000000000000000, 0.9238795325112869605, 1.000000000000000000, 0.9238795325112869605, 1.000000000000000000, 0.9238795325112869605, 1.000000000000000000, 0.9238795325112869605, 1.000000000000000000, 0.9238795325112869605, 1.000000000000000000, 0.9238795325112869605, 1.000000000000000000, 0.9238795325112869605, 1.000000000000000000, 0.9238795325112869605, 1.000000000000000000, 0.9238795325112869605, 1.000000000000000000, 0.9238795325112869605, 1.000000000000000000, 0.9238795325112869605, 1.000000000000000000, 0.9238795325112869605, 1.000000000000000000, 0.9238795325112869605, 1.000000000000000000, 0.9238795325112869605, 1.000000000000000000, 0.9238795325112869605, 1.000000000000000000, 0.9238795325112869605, 1.000000000000000000, 0.9238795325112869605, 1.000000000000000000, 0.9238795325112869605, 1.000000000000000000, 0.9238795325112869605, 1.000000000000000000, 0.9238795325112869605, 1.000000000000000000),
 ( 1.000000000000000000, 0.9238795325112869605, 1.000000000000000000, 0.9238795325112869605, 1.000000000000000000, 0.9238795325112869605, 1.000000000000000000, 0.9238795325112869605, 1.000000000000000000, 0.9238795325112869605, 1.000000000000000000, 0.9238795325112869605, 1.000000000000000000, 0.9238795325112869605, 1.000000000000000000, 0.9238795325112869605, 1.000000000000000000, 0.9238795325112869605, 1.000000000000000000, 0.9238795325112869605, 1.000000000000000000, 0.9238795325112869605, 1.000000000000000000, 0.9238795325112869605, 1.000000000000000000, 0.9238795325112869605, 1.000000000000000000, 0.9238795325112869605, 1.000000000000000000, 0.9238795325112869605, 1.000000000000000000, 0.9238795325112869605, 1.000000000000000000, 0.9238795325112869605, 1.000000000000000000, 0.9238795325112869605, 1.000000000000000000, 0.9238795325112869605, 1.000000000000000000, 0.9238795325112869605, 1.000000000000000000, 0.9238795325112869605, 1.000000000000000000, 0.9238795325112869605, 1.000000000000000000, 0.9238795325112869605, 1.000000000000000000, 0.9238795325112869605, 1.000000000000000000, 0.9238795325112869605, 1.000000000000000000, 0.9238795325112869605, 1.000000000000000000, 0.9238795325112869605, 1.000000000000000000, 0.9238795325112869605, 1.000000000000000000, 0.9238795325112869605, 1.000000000000000000, 0.9238795325112869605, 1.000000000000000000, 0.9238795325112869605, 1.000000000000000000, 0.9238795325112869605, 1.000000000000000000, 0.9238795325112869605, 1.000000000000000000, 0.9238795325112869605, 1.000000000000000000, 0.9238795325112869605, 1.000000000000000000, 0.9238795325112869605, 1.000000000000000000, 0.9238795325112869605, 1.000000000000000000, 0.9238795325112869605, 1.000000000000000000, 0.9238795325112869605, 1.000000000000000000, 0.9238795325112869605, 1.000000000000000000, 0.9238795325112869605, 1.000000000000000000, 0.9238795325112869605, 1.000000000000000000, 0.9238795325112869605, 1.000000000000000000, 0.9238795325112869605, 1.000000000000000000, 0.9238795325112869605, 1.000000000000000000, 0.9238795325112869605, 1.000000000000000000, 0.9238795325112869605, 1.000000000000000000, 0.9238795325112869605, 1.000000000000000000, 0.9238795325112869605, 1.000000000000000000, 0.9238795325112869605, 1.000000000000000000, 0.9238795325112869605, 1.000000000000000000, 0.9238795325112869605, 1.000000000000000000, 0.9238795325112869605, 1.000000000000000000, 0.9238795325112869605, 1.000000000000000000, 0.9238795325112869605, 1.000000000000000000, 0.9238795325112869605, 1.000000000000000000, 0.9238795325112869605, 1.000000000000000000, 0.9238795325112869605, 1.000000000000000000, 0.9238795325112869605, 1.000000000000000000, 0.9238795325112869605, 1.000000000000000000, 0.9238795325112869605, 1.000000000000000000, 0.9238795325112869605, 1.000000000000000000, 0.9238795325112869605, 1.000000000000000000, 0.9238795325112869605, 1.000000000000000000, 0.9238795325112869605, 1.000000000000000000, 0.9238795325112869605, 1.000000000000000000, 0.9238795325112869605, 1.000000000000000000, 0.9238795325112869605, 1.000000000000000000, 0.9238795325112869605, 1.000000000000000000, 0.9238795325112869605, 1.000000000000000000, 0.9238795325112869605, 1.000000000000000000, 0.9238795325112869605, 1.000000000000000000, 0.9238795325112869605, 1.000000000000000000, 0.9238795325112869605, 1.000000000000000000, 0.9238795325112869605, 1.000000000000000000, 0.9238795325112869605, 1.000000000000000000, 0.9238795325112869605, 1.000000000000000000, 0.9238795325112869605, 1.000000000000000000, 0.9238795325112869605, 1.000000000000000000, 0.9238795325112869605, 1.000000000000000000, 0.9238795325112869605, 1.000000000000000000, 0.9238795325112869605, 1.000000000000000000, 0.9238795325112869605, 1.000000000000000000, 0.9238795325112869605, 1.000000000000000000, 0.9238795325112869605, 1.000000000000000000, 0.9238795325112869605, 1.000000000000000000, 0.9238795325112869605, 1.000000000000000000, 0.9238795325112869605, 1.000000000000000000, 0.9238795325112869605, 1.000000000000000000, 0.9238795325112869605, 1.000000000000000000, 0.9238795325112869605, 1.000000000000000000, 0.9238795325112869605, 1.000000000000000000, 0.9238795325112869605, 1.000000000000000000, 0.9238795325112869605, 1.000000000000000000, 0.9238795325112869605, 1.000000000000000000, 0.9238795325112869605, 1.000000000000000000, 0.9238795325112869605, 1.000000000000000000, 0.9238795325112869605, 1.000000000000000000, 0.9238795325112869605, 1.000000000000000000, 0.9238795325112869605, 1.000000000000000000, 0.9238795325112869605, 1.000000000000000000, 0.9238795325112869605, 1.000000000000000000, 0.9238795325112869605, 1.000000000000000000, 0.9238795325112869605, 1.000000000000000000, 0.9238795325112869605, 1.000000000000000000, 0.9238795325112869605, 1.000000000000000000, 0.9238795325112869605, 1.000000000000000000, 0.9238795325112869605, 1.000000000000000000, 0.9238795325112869605, 1.000000000000000000, 0.9238795325112869605, 1.000000000000000000, 0.9238795325112869605, 1.000000000000000000, 0.9238795325112869605, 1.000000000000000000, 0.9238795325112869605, 1.000000000000000000, 0.9238795325112869605, 1.000000000000000000, 0.9238795325112869605, 1.000000000000000000, 0.9238795325112869605, 1.000000000000000000, 0.9238795325112869605, 1.000000000000000000, 0.9238795325112869605, 1.000000000000000000, 0.9238795325112869605, 1.000000000000000000, 0.9238795325112869605, 1.000000000000000000, 0.9238795325112869605, 1.000000000000000000, 0.9238795325112869605, 1.000000000000000000, 0.9238795325112869605, 1.000000000000000000, 0.9238795325112869605, 1.000000000000000000, 0.9238795325112869605, 1.000000000000000000, 0.9238795325112869605, 1.000000000000000000, 0.9238795325112869605, 1.000000000000000000, 0.9238795325112869605, 1.000000000000000000) ) ) 
 REPRESENTATION_ITEM ( '' )  SURFACE ( )  );
#32543 = CARTESIAN_POINT ( 'NONE',  ( 122.1561614775786353, -8.899110576539710493, -16.42337572283490132 ) ) ;
#32544 = DIRECTION ( 'NONE',  ( 0.000000000000000000, -0.9242245927363028635, -0.3818493186865930533 ) ) ;
#32545 = CARTESIAN_POINT ( 'NONE',  ( 78.93021946355167984, -3.662536865724447921, -14.39321520033831625 ) ) ;
#32546 = CARTESIAN_POINT ( 'NONE',  ( 125.1670174127246469, -12.14974810887502521, -14.66706061084391699 ) ) ;
#32547 = VECTOR ( 'NONE', #5396, 1000.000000000000227 ) ;
#32548 = CARTESIAN_POINT ( 'NONE',  ( 123.7445081442452874, -7.894159318335828068, -9.358103419637847864 ) ) ;
#32549 = ADVANCED_FACE ( 'NONE', ( #33255 ), #22763, .T. ) ;
#32550 = CARTESIAN_POINT ( 'NONE',  ( 112.4559014775786494, -9.988377603198976828, -10.36322818467138340 ) ) ;
#32551 = CARTESIAN_POINT ( 'NONE',  ( 121.0216281442452981, -1.561330072975668948, -17.79121239304076951 ) ) ;
#32552 = CARTESIAN_POINT ( 'NONE',  ( 125.7866681442452688, -8.899110576539710493, -16.42337572283490132 ) ) ;
#32553 = DIRECTION ( 'NONE',  ( -0.000000000000000000, -0.9284778069183721172, -0.3713878862591650232 ) ) ;
#32554 = EDGE_CURVE ( 'NONE', #9687, #574, #23243, .T. ) ;
#32555 = EDGE_CURVE ( 'NONE', #11788, #16463, #6739, .T. ) ;
#32556 = CARTESIAN_POINT ( 'NONE',  ( 120.5110881442453206, -3.505236298600246325, -18.68346056562440793 ) ) ;
#32557 = ORIENTED_EDGE ( 'NONE', *, *, #6632, .F. ) ;
#32558 = CARTESIAN_POINT ( 'NONE',  ( 118.9794681442453026, -9.261995988541697145, -16.69588392320189030 ) ) ;
#32559 = CARTESIAN_POINT ( 'NONE',  ( 112.6356140045247827, 0.1403307496149616695, -15.46607636864997204 ) ) ;
#32560 = CARTESIAN_POINT ( 'NONE',  ( 87.68939540009954214, -24.14644159042263993, -12.62951656296512937 ) ) ;
#32561 = CARTESIAN_POINT ( 'NONE',  ( 114.1577014775786552, -3.505236298600246325, -18.68346056562440793 ) ) ;
#32562 = DIRECTION ( 'NONE',  ( -0.000000000000000000, -0.9284778069183721172, -0.3713878862591650232 ) ) ;
#32563 = CARTESIAN_POINT ( 'NONE',  ( 125.3328548109119964, -9.261995988541697145, -16.69588392320189030 ) ) ;
#32564 = VERTEX_POINT ( 'NONE', #12312 ) ;
#32565 = CARTESIAN_POINT ( 'NONE',  ( 121.9859814775786333, -9.565557343593413364, -10.61323700422348004 ) ) ;
#32566 = CARTESIAN_POINT ( 'NONE',  ( -13.43670958668108462, -4.952261022111287936, -18.17119155822705778 ) ) ;
#32567 = CARTESIAN_POINT ( 'NONE',  ( 123.2855641859119942, -0.8832429491016019485, -18.19431474523657855 ) ) ;
#32568 = CIRCLE ( 'NONE', #43523, 2.999999999999999556 ) ;
#32569 = CARTESIAN_POINT ( 'NONE',  ( 61.43583762032555029, 4.505738898882963639, -12.14321520033831625 ) ) ;
#32570 = CARTESIAN_POINT ( 'NONE',  ( 108.8851452545248151, -9.868328341294098749, -15.46607636864997204 ) ) ;
#32571 = ORIENTED_EDGE ( 'NONE', *, *, #6805, .T. ) ;
#32572 = CARTESIAN_POINT ( 'NONE',  ( 113.7038881442453402, -3.383040157471821630, -19.15922257007629170 ) ) ;
#32573 = CARTESIAN_POINT ( 'NONE',  ( 88.52634549546732501, -11.38007610471903419, -13.93176785127966966 ) ) ;
#32574 = CARTESIAN_POINT ( 'NONE',  ( 121.3052614775786111, -7.643976991954077427, -18.09477374809248928 ) ) ;
#32575 = CARTESIAN_POINT ( 'NONE',  ( 79.05243529145373316, 4.793396140045460108, -4.893215200338314474 ) ) ;
#32576 = CARTESIAN_POINT ( 'NONE',  ( 123.7445081442452874, -7.894159318335831621, -9.358103419637849640 ) ) ;
#32577 = CARTESIAN_POINT ( 'NONE',  ( 124.5847204811916669, -3.807985514183276354, -19.09877912889402651 ) ) ;
#32578 = LINE ( 'NONE', #39204, #260 ) ;
#32579 = VERTEX_POINT ( 'NONE', #16634 ) ;
#32580 = CARTESIAN_POINT ( 'NONE',  ( 114.8581140045248361, 0.1403307496149616695, -15.46607636864997204 ) ) ;
#32581 = AXIS2_PLACEMENT_3D ( 'NONE', #4628, #18324, #4856 ) ;
#32582 = CARTESIAN_POINT ( 'NONE',  ( 120.5678148109119832, -8.166667518702819706, -8.995218007635861213 ) ) ;
#32583 = CARTESIAN_POINT ( 'NONE',  ( 31.16203868753470019, 11.28474725185576055, -8.893215200338314474 ) ) ;
#32584 = ORIENTED_EDGE ( 'NONE', *, *, #14765, .F. ) ;
#32585 = DIRECTION ( 'NONE',  ( 1.000000000000000000, -1.084202172485504040E-15, 0.000000000000000000 ) ) ;
#32586 = CARTESIAN_POINT ( 'NONE',  ( 125.5030348109119558, -3.383040157471821630, -19.15922257007629170 ) ) ;
#32587 = CARTESIAN_POINT ( 'NONE',  ( 111.5006797178593700, -0.3595008806742178709, -15.96590799893915857 ) ) ;
#32588 = ADVANCED_FACE ( 'NONE', ( #30528 ), #36457, .F. ) ;
#32589 = CARTESIAN_POINT ( 'NONE',  ( 125.1059481442452750, -1.833838273342660141, -17.42832698103878286 ) ) ;
#32590 = EDGE_LOOP ( 'NONE', ( #6429, #31252, #10204, #12062 ) ) ;
#32591 = CARTESIAN_POINT ( 'NONE',  ( 117.3911214775786505, -1.561330072975668504, -17.79121239304076951 ) ) ;
#32592 = LINE ( 'NONE', #5676, #26696 ) ;
#32593 = DIRECTION ( 'NONE',  ( 0.000000000000000000, 0.000000000000000000, 1.000000000000000000 ) ) ;
#32594 = CARTESIAN_POINT ( 'NONE',  ( 115.2518531537514832, 0.4930828106259610433, -14.64321520033831447 ) ) ;
#32595 = DIRECTION ( 'NONE',  ( 0.000000000000000000, -0.3818493186865927203, 0.9242245927363029745 ) ) ;
#32596 =( GEOMETRIC_REPRESENTATION_CONTEXT ( 3 ) GLOBAL_UNCERTAINTY_ASSIGNED_CONTEXT ( ( #8251 ) ) GLOBAL_UNIT_ASSIGNED_CONTEXT ( ( #25752, #39658, #12749 ) ) REPRESENTATION_CONTEXT ( 'NONE', 'WORKASPACE' ) );
#32597 = CARTESIAN_POINT ( 'NONE',  ( 124.4252281442452812, -9.261995988541697145, -16.69588392320189030 ) ) ;
#32598 = CARTESIAN_POINT ( 'NONE',  ( 72.54180985774836188, -56.94300424148091366, -35.25083934068751290 ) ) ;
#32599 = DIRECTION ( 'NONE',  ( 0.000000000000000000, -0.3818493186865936084, 0.9242245927363024194 ) ) ;
#32600 = CARTESIAN_POINT ( 'NONE',  ( 113.1366214775786432, -7.643976991954077427, -18.09477374809248928 ) ) ;
#32601 =( REPRESENTATION_RELATIONSHIP ('NONE','NONE', #36667, #10805 ) REPRESENTATION_RELATIONSHIP_WITH_TRANSFORMATION ( #37524 )SHAPE_REPRESENTATION_RELATIONSHIP( ) );
#32602 = CARTESIAN_POINT ( 'NONE',  ( 125.3895814775786448, -2.084020599724406786, -8.691656652584148546 ) ) ;
#32603 = CARTESIAN_POINT ( 'NONE',  ( 85.43169907558235820, -26.60966817898065884, -11.90521360603286816 ) ) ;
#32604 = CARTESIAN_POINT ( 'NONE',  ( 123.0070614775786169, -10.15424416112533912, -14.75197769757731336 ) ) ;
#32605 = CARTESIAN_POINT ( 'NONE',  ( 113.5904348109119866, -2.084020599724406786, -8.691656652584148546 ) ) ;
#32606 = CARTESIAN_POINT ( 'NONE',  ( 121.0216281442452981, -1.561330072975668948, -17.79121239304076951 ) ) ;
#32607 = ADVANCED_FACE ( 'NONE', ( #1798, #26209 ), #5446, .F. ) ;
#32608 = ORIENTED_EDGE ( 'NONE', *, *, #42087, .F. ) ;
#32609 = FACE_OUTER_BOUND ( 'NONE', #15708, .T. ) ;
#32610 = DIRECTION ( 'NONE',  ( 0.000000000000000000, -0.9284778069183718952, -0.3713878862591650232 ) ) ;
#32611 = CARTESIAN_POINT ( 'NONE',  ( 110.5520202545248054, 0.1403307496149616695, -11.32035403202665336 ) ) ;
#32612 = CARTESIAN_POINT ( 'NONE',  ( 111.2465515045248168, -6.936859964151250502, -18.39754474579286025 ) ) ;
#32613 = EDGE_CURVE ( 'NONE', #15033, #13487, #2479, .T. ) ;
#32614 = CARTESIAN_POINT ( 'NONE',  ( 126.2333338125945517, -9.798786772754054297, -12.54286052501422688 ) ) ;
#32615 = CARTESIAN_POINT ( 'NONE',  ( 113.6471614775786492, -5.638512984488999180, -18.83840828888717311 ) ) ;
#32616 = ORIENTED_EDGE ( 'NONE', *, *, #39615, .T. ) ;
#32617 = CARTESIAN_POINT ( 'NONE',  ( 116.6536748109119941, -10.15424416112533912, -14.75197769757731336 ) ) ;
#32618 = CARTESIAN_POINT ( 'NONE',  ( 108.3295202545248657, -10.62599879583958717, -15.77991374673208469 ) ) ;
#32619 = LINE ( 'NONE', #21917, #10321 ) ;
#32620 = EDGE_CURVE ( 'NONE', #12113, #11479, #2027, .T. ) ;
#32621 = CYLINDRICAL_SURFACE ( 'NONE', #24746, 1.999999999999998890 ) ;
#32622 = CARTESIAN_POINT ( 'NONE',  ( 123.2223381469516568, -3.929494816604741203, -18.62311481910882804 ) ) ;
#32623 = CARTESIAN_POINT ( 'NONE',  ( 113.8604010812576774, -0.01829820670803256055, -12.14321520033831625 ) ) ;
#32624 = CARTESIAN_POINT ( 'NONE',  ( 115.8595014775786609, -1.834011780172310813, -8.268836392978581529 ) ) ;
#32625 = CARTESIAN_POINT ( 'NONE',  ( 109.1629577545248395, -7.250697342233347165, -7.631215200338321125 ) ) ;
#32626 = CARTESIAN_POINT ( 'NONE',  ( 113.2606921295247702, -9.868328341294093420, -13.39321520033831447 ) ) ;
#32627 = ORIENTED_EDGE ( 'NONE', *, *, #27633, .F. ) ;
#32628 = DIRECTION ( 'NONE',  ( 0.000000000000000000, 0.000000000000000000, -1.000000000000000000 ) ) ;
#32629 = CARTESIAN_POINT ( 'NONE',  ( 117.3343948109119737, -6.222761293078241884, -8.102969835052219238 ) ) ;
#32630 = CARTESIAN_POINT ( 'NONE',  ( 115.5191414775786569, -3.383040157471821630, -19.15922257007629170 ) ) ;
#32631 = CARTESIAN_POINT ( 'NONE',  ( 71.02242295334774269, -51.54654354869580857, -36.92625453930496349 ) ) ;
#32632 = CARTESIAN_POINT ( 'NONE',  ( 125.2761281442453054, 0.4262465694468514643, -12.03445270309931736 ) ) ;
#32633 = CARTESIAN_POINT ( 'NONE',  ( 124.9357681442453014, -7.643976991954077427, -18.09477374809248928 ) ) ;
#32634 = CARTESIAN_POINT ( 'NONE',  ( 116.5402214775786405, -9.565557343593413364, -10.61323700422348004 ) ) ;
#32635 = ORIENTED_EDGE ( 'NONE', *, *, #27585, .F. ) ;
#32636 = CARTESIAN_POINT ( 'NONE',  ( 122.8688454359119646, 0.5291689781388270175, -13.89700978578772705 ) ) ;
#32637 = CARTESIAN_POINT ( 'NONE',  ( 113.6773954522301864, 0.1168444861213632779, -14.64321520033831447 ) ) ;
#32638 = CARTESIAN_POINT ( 'NONE',  ( 119.4332814775786318, -8.899110576539710493, -16.42337572283490132 ) ) ;
#32639 = EDGE_LOOP ( 'NONE', ( #38922, #6550, #30426, #15805, #41863, #8777 ) ) ;
#32640 = CARTESIAN_POINT ( 'NONE',  ( 113.5904348109119866, -7.893985811506177619, -18.51759400769804742 ) ) ;
#32641 = CARTESIAN_POINT ( 'NONE',  ( 106.6626452545248611, -9.868328341294098749, -15.46607636864997204 ) ) ;
#32642 = CARTESIAN_POINT ( 'NONE',  ( 114.3278814775786429, 0.1319031606808879209, -14.10382304977623669 ) ) ;
#32643 = ORIENTED_EDGE ( 'NONE', *, *, #9573, .F. ) ;
#32644 = VERTEX_POINT ( 'NONE', #30304 ) ;
#32645 = CARTESIAN_POINT ( 'NONE',  ( 121.4754414775786131, -1.833838273342659697, -17.42832698103878286 ) ) ;
#32646 = CARTESIAN_POINT ( 'NONE',  ( 115.9729548109119861, -3.505236298600246325, -18.68346056562440793 ) ) ;
#32647 = CARTESIAN_POINT ( 'NONE',  ( 110.8846310998092264, -2.698019154030093514, -17.52653087006472177 ) ) ;
#32648 = EDGE_CURVE ( 'NONE', #35146, #38132, #15482, .T. ) ;
#32649 = CARTESIAN_POINT ( 'NONE',  ( 116.3133148109120043, -2.084020599724407230, -8.691656652584150322 ) ) ;
#32650 = ORIENTED_EDGE ( 'NONE', *, *, #26741, .F. ) ;
#32651 = CARTESIAN_POINT ( 'NONE',  ( 119.7434548109119703, -4.863998795839242995, -13.39321520033831447 ) ) ;
#32652 = CARTESIAN_POINT ( 'NONE',  ( 61.79265099467970401, -65.87623890127542836, -43.58359585756122101 ) ) ;
#32653 = CARTESIAN_POINT ( 'NONE',  ( 112.2883483795247770, -0.7896495226426338832, -9.318865927141430916 ) ) ;
#32654 = CARTESIAN_POINT ( 'NONE',  ( 116.7104014775786425, -0.4660016031367893996, -10.09054647747474043 ) ) ;
#32656 = CARTESIAN_POINT ( 'NONE',  ( 116.8238548109119819, -5.574606645277164318, -18.38911715685844683 ) ) ;
#32655 = CARTESIAN_POINT ( 'NONE',  ( 112.6828081442453282, -7.893985811506177619, -18.51759400769804742 ) ) ;
#32657 = CARTESIAN_POINT ( 'NONE',  ( 120.3976348109119812, -7.643976991954077427, -18.09477374809248928 ) ) ;
#32658 = DIRECTION ( 'NONE',  ( 0.000000000000000000, 0.000000000000000000, 1.000000000000000000 ) ) ;
#32659 = EDGE_LOOP ( 'NONE', ( #4885, #4548, #38083, #14935 ) ) ;
#32660 = CARTESIAN_POINT ( 'NONE',  ( 118.4122014775786340, -9.859900752359374465, -12.68260735090039404 ) ) ;
#32661 = CARTESIAN_POINT ( 'NONE',  ( 125.5030348109119558, -6.222761293078241884, -8.102969835052219238 ) ) ;
#32662 = CARTESIAN_POINT ( 'NONE',  ( 111.5938171295247940, -10.62599879583958540, -13.39321520033831447 ) ) ;
#32663 = CARTESIAN_POINT ( 'NONE',  ( 116.4555358795247884, -8.402594152722688392, -9.854619843455216355 ) ) ;
#32664 = CARTESIAN_POINT ( 'NONE',  ( 114.0941296295247867, -4.863998795839590272, -19.15521520033831493 ) ) ;
#32665 = EDGE_CURVE ( 'NONE', #43595, #1042, #35836, .T. ) ;
#32666 = CARTESIAN_POINT ( 'NONE',  ( 116.9940348109119839, -9.988377603198976828, -10.36322818467138340 ) ) ;
#32667 = VERTEX_POINT ( 'NONE', #3817 ) ;
#32668 = CARTESIAN_POINT ( 'NONE',  ( 121.8725281442453223, -3.383040157471821630, -19.15922257007629170 ) ) ;
#32669 = CARTESIAN_POINT ( 'NONE',  ( 96.54708369096698561, -28.17862604940189541, -13.73821557025528683 ) ) ;
#32670 = CARTESIAN_POINT ( 'NONE',  ( 106.3153796295248412, -4.863998795839590272, -19.15521520033831493 ) ) ;
#32671 = CARTESIAN_POINT ( 'NONE',  ( 117.5613014775786525, 0.9020085738987339008, -11.91225656197089222 ) ) ;
#32672 = CARTESIAN_POINT ( 'NONE',  ( 116.4834948109119779, -1.561330072975668504, -17.79121239304076951 ) ) ;
#32673 = CARTESIAN_POINT ( 'NONE',  ( 126.3115243456358883, -9.898515367256928599, -13.04493836775356463 ) ) ;
#32674 = CARTESIAN_POINT ( 'NONE',  ( 117.0832711243935051, -11.36631965120432319, -5.665662734129918832 ) ) ;
#32675 = CARTESIAN_POINT ( 'NONE',  ( 107.2877233795247776, -1.325403438956436419, -9.854619843455211026 ) ) ;
#32676 = ORIENTED_EDGE ( 'NONE', *, *, #1678, .F. ) ;
#32677 = CARTESIAN_POINT ( 'NONE',  ( 116.3860827545247787, -2.477300249445798297, -19.15521520033830427 ) ) ;
#32678 = CARTESIAN_POINT ( 'NONE',  ( 109.2294433879109761, -10.43664627197690642, -13.07502879523307016 ) ) ;
#32679 = CARTESIAN_POINT ( 'NONE',  ( 118.5823814775786360, -7.643976991954077427, -18.09477374809248928 ) ) ;
#32680 = CARTESIAN_POINT ( 'NONE',  ( 112.7745202545247878, 0.1403307496149616695, -11.32035403202665336 ) ) ;
#32681 = CARTESIAN_POINT ( 'NONE',  ( 114.9275671295247889, 0.1403307496149613920, -13.39321520033831447 ) ) ;
#32682 = CARTESIAN_POINT ( 'NONE',  ( 113.8173414775786512, -9.565557343593413364, -10.61323700422348004 ) ) ;
#32683 = CARTESIAN_POINT ( 'NONE',  ( 78.93021946355167984, -3.662536865724447921, -19.39321520033831447 ) ) ;
#32684 = CARTESIAN_POINT ( 'NONE',  ( 112.3424481442453384, -3.505236298600246325, -18.68346056562440793 ) ) ;
#32685 = CARTESIAN_POINT ( 'NONE',  ( 118.2987481442453088, -1.561330072975668504, -17.79121239304076951 ) ) ;
#32686 = ORIENTED_EDGE ( 'NONE', *, *, #43690, .T. ) ;
#32687 = CARTESIAN_POINT ( 'NONE',  ( 117.3343948109119737, -6.222761293078241884, -8.102969835052219238 ) ) ;
#32688 = CARTESIAN_POINT ( 'NONE',  ( 116.3700414775786527, -5.638512984488999180, -18.83840828888717311 ) ) ;
#32690 = EDGE_CURVE ( 'NONE', #35231, #1795, #24149, .T. ) ;
#32689 = CARTESIAN_POINT ( 'NONE',  ( 119.7169148109119874, -9.988377603198976828, -10.36322818467138340 ) ) ;
#32691 = CARTESIAN_POINT ( 'NONE',  ( 121.3052614775786111, -7.643976991954077427, -18.09477374809248928 ) ) ;
#32692 = ORIENTED_EDGE ( 'NONE', *, *, #44046, .F. ) ;
#32693 = CARTESIAN_POINT ( 'NONE',  ( 123.4041481442452834, 0.1319031606808879209, -14.10382304977623669 ) ) ;
#32694 = CARTESIAN_POINT ( 'NONE',  ( 118.6958348109119754, -6.344957434206665248, -7.627207830600338134 ) ) ;
#32695 = CARTESIAN_POINT ( 'NONE',  ( 125.0211000582877006, -8.115061802111570799, -6.569347472097891050 ) ) ;
#32696 = CARTESIAN_POINT ( 'NONE',  ( 120.2841814775786276, 0.9020085738987339008, -11.91225656197089222 ) ) ;
#32697 = CARTESIAN_POINT ( 'NONE',  ( 151.2860562277021472, -1.295815253274133161, -16.89579513612386563 ) ) ;
#32698 = DIRECTION ( 'NONE',  ( 0.9609149988134843001, -0.1028163501681632064, 0.2570431154366505933 ) ) ;
#32699 = CARTESIAN_POINT ( 'NONE',  ( 112.4272546295247821, -4.863998795839590272, -18.39754474579285315 ) ) ;
#32700 = CARTESIAN_POINT ( 'NONE',  ( 123.0772048109119652, -2.527210466738041728, -8.967976844669124148 ) ) ;
#32701 = AXIS2_PLACEMENT_3D ( 'NONE', #1220, #8292, #22419 ) ;
#32702 = CARTESIAN_POINT ( 'NONE',  ( 135.5886503745816469, -10.36823017854120543, -11.00515641294314584 ) ) ;
#32703 = CARTESIAN_POINT ( 'NONE',  ( 114.4413348109119823, -0.8288870151387760510, -10.36305467784173118 ) ) ;
#32704 = CARTESIAN_POINT ( 'NONE',  ( 124.2550481442452792, -9.988377603198980381, -10.36322818467138518 ) ) ;
#32705 = PLANE ( 'NONE',  #21397 ) ;
#32706 = CARTESIAN_POINT ( 'NONE',  ( 110.8992858795247827, -8.402594152722688392, -9.854619843455216355 ) ) ;
#32707 = CARTESIAN_POINT ( 'NONE',  ( 114.7249681442453237, -9.565557343593413364, -10.61323700422348004 ) ) ;
#32708 = CARTESIAN_POINT ( 'NONE',  ( 114.9859420330015354, -1.172797794773246416, -17.05961127468924587 ) ) ;
#32709 = CARTESIAN_POINT ( 'NONE',  ( -2.040426804217055246, -6.896677610160479865, -18.93444115535162453 ) ) ;
#32711 = CARTESIAN_POINT ( 'NONE',  ( 118.2420214775786320, -3.383040157471821630, -19.15922257007629170 ) ) ;
#32710 = CARTESIAN_POINT ( 'NONE',  ( 61.93156847455978919, -13.30602482174417389, -7.732832247245597479 ) ) ;
#32712 = EDGE_CURVE ( 'NONE', #8271, #21347, #31637, .T. ) ;
#32713 = CARTESIAN_POINT ( 'NONE',  ( 121.3619881442452879, -5.574606645277164318, -18.38911715685844683 ) ) ;
#32714 = ORIENTED_EDGE ( 'NONE', *, *, #3612, .F. ) ;
#32715 = CARTESIAN_POINT ( 'NONE',  ( 136.2632467228178825, -7.076446026251988819, -7.986235859556298777 ) ) ;
#32716 = CARTESIAN_POINT ( 'NONE',  ( 69.69189222815028018, -41.76310523276638520, -10.89321520033831447 ) ) ;
#32717 = CARTESIAN_POINT ( 'NONE',  ( 109.4407702545248355, 0.1403307496149616695, -11.32035403202665336 ) ) ;
#32718 = CARTESIAN_POINT ( 'NONE',  ( 119.6034614775786196, -3.505236298600246325, -18.68346056562440793 ) ) ;
#32719 = CARTESIAN_POINT ( 'NONE',  ( 120.9081748109119872, -4.153390946401325223, -8.397313243818185668 ) ) ;
#32720 = CARTESIAN_POINT ( 'NONE',  ( 117.2776681442452968, -4.153390946401325223, -8.397313243818185668 ) ) ;
#32721 = CARTESIAN_POINT ( 'NONE',  ( 125.2231329858062878, 1.951969713414328123, -16.04783498356866644 ) ) ;
#32722 = CARTESIAN_POINT ( 'NONE',  ( 108.5378796295247810, -4.863998795839590272, -19.15521520033831493 ) ) ;
#32723 = CARTESIAN_POINT ( 'NONE',  ( 123.1205148109119563, -7.643976991954077427, -18.09477374809248928 ) ) ;
#32724 = CARTESIAN_POINT ( 'NONE',  ( 125.2761281442453054, 0.4262465694468514643, -12.03445270309931736 ) ) ;
#32725 = LINE ( 'NONE', #22256, #23838 ) ;
#32726 = CARTESIAN_POINT ( 'NONE',  ( 112.4201593777725208, -1.267766418764741276, -16.93314635290707315 ) ) ;
#32727 = CARTESIAN_POINT ( 'NONE',  ( 124.1190016859119680, -9.665098340737509730, -17.37397104707595474 ) ) ;
#32728 = CARTESIAN_POINT ( 'NONE',  ( 116.1082702545247827, -10.62599879583958717, -15.77991374673208469 ) ) ;
#32729 = FACE_OUTER_BOUND ( 'NONE', #40738, .T. ) ;
#32730 = CARTESIAN_POINT ( 'NONE',  ( 83.38637814964508266, -33.05952087933068384, -23.46618001151087540 ) ) ;
#32731 = CARTESIAN_POINT ( 'NONE',  ( 119.4332814775786318, -0.4660016031367893996, -10.09054647747474043 ) ) ;
#32732 = CARTESIAN_POINT ( 'NONE',  ( 117.2209414775786485, -7.893985811506177619, -18.51759400769804742 ) ) ;
#32733 = CARTESIAN_POINT ( 'NONE',  ( 107.6349890045248401, 0.8980012041604421569, -15.77991374673208469 ) ) ;
#32734 = CARTESIAN_POINT ( 'NONE',  ( 116.0864081442453113, -9.988377603198976828, -10.36322818467138340 ) ) ;
#32735 = DIRECTION ( 'NONE',  ( -0.7871354856660202071, 0.6167752151498580027, 0.002461946824133919541 ) ) ;
#32736 = ORIENTED_EDGE ( 'NONE', *, *, #40464, .T. ) ;
#32737 = DIRECTION ( 'NONE',  ( 0.9609149988134843001, -0.1028163501681632064, 0.2570431154366505933 ) ) ;
#32738 = CARTESIAN_POINT ( 'NONE',  ( 119.1496481442453046, -3.383040157471821630, -19.15922257007629170 ) ) ;
#32739 = CIRCLE ( 'NONE', #31288, 8.000000000000001776 ) ;
#32740 = CARTESIAN_POINT ( 'NONE',  ( 111.8886348109120092, -3.383040157471821630, -19.15922257007629170 ) ) ;
#32741 = PRODUCT_CONTEXT ( 'NONE', #37879, 'mechanical' ) ;
#32742 = CARTESIAN_POINT ( 'NONE',  ( 113.0231681442453180, -10.15424416112533912, -14.75197769757731336 ) ) ;
#32743 = CARTESIAN_POINT ( 'NONE',  ( 111.3213681442453264, -7.643976991954077427, -18.09477374809248928 ) ) ;
#32744 = CARTESIAN_POINT ( 'NONE',  ( 114.9275671295247889, -10.62599879583958540, -13.39321520033831447 ) ) ;
#32745 = CARTESIAN_POINT ( 'NONE',  ( 118.2987481442453088, -7.894159318335828068, -9.358103419637847864 ) ) ;
#32746 = CARTESIAN_POINT ( 'NONE',  ( 96.21525317080913453, -24.35736823789046568, -12.15943839496780399 ) ) ;
#32747 = CARTESIAN_POINT ( 'NONE',  ( 89.67401078471493747, -25.99489077589524300, -13.39321520033831447 ) ) ;
#32748 = ORIENTED_EDGE ( 'NONE', *, *, #15069, .F. ) ;
#32749 = AXIS2_PLACEMENT_3D ( 'NONE', #12837, #36748, #19893 ) ;
#32750 = CARTESIAN_POINT ( 'NONE',  ( 119.5350954359119839, 0.5291689781388270175, -13.89700978578772705 ) ) ;
#32751 = CARTESIAN_POINT ( 'NONE',  ( 122.0427081442452817, 0.5811942927096110934, -14.16772938898807510 ) ) ;
#32752 = EDGE_LOOP ( 'NONE', ( #26722, #28555, #33646, #36479 ) ) ;
#32753 = CARTESIAN_POINT ( 'NONE',  ( 77.77634386988368931, 3.254514819260763581, -4.893215200338314474 ) ) ;
#32754 = CARTESIAN_POINT ( 'NONE',  ( 111.4705635773848940, -2.467220198592768199, -17.83387418641523325 ) ) ;
#32755 = DIRECTION ( 'NONE',  ( -0.8636456077245080465, 0.5040994586965603652, 0.000000000000000000 ) ) ;
#32756 = CARTESIAN_POINT ( 'NONE',  ( 119.2063748109119814, -7.894159318335828068, -9.358103419637847864 ) ) ;
#32757 = CARTESIAN_POINT ( 'NONE',  ( 68.15795393973013461, -1.183743427963408701, -16.39321520033831447 ) ) ;
#32758 = CARTESIAN_POINT ( 'NONE',  ( 124.5060894275148087, -9.676259452193004762, -12.03595266200289338 ) ) ;
#32759 = CARTESIAN_POINT ( 'NONE',  ( 125.1626748109119802, -0.1624402480850797581, -16.17319339645315424 ) ) ;
#32760 = FACE_OUTER_BOUND ( 'NONE', #42587, .T. ) ;
#32761 = CARTESIAN_POINT ( 'NONE',  ( 123.7445081442452874, -7.894159318335828068, -9.358103419637847864 ) ) ;
#32762 = CONICAL_SURFACE ( 'NONE', #5108, 2.445500000000004448, 0.9599310885968757034 ) ;
#32763 = CARTESIAN_POINT ( 'NONE',  ( 125.3495511204625927, -11.67227941590863871, -15.26752859910581606 ) ) ;
#32764 = CARTESIAN_POINT ( 'NONE',  ( 116.0864081442453113, -0.1624402480850797581, -16.17319339645315424 ) ) ;
#32765 = CARTESIAN_POINT ( 'NONE',  ( 121.9859814775786333, -9.565557343593413364, -10.61323700422348004 ) ) ;
#32766 = CARTESIAN_POINT ( 'NONE',  ( 117.9016614775786280, -9.988377603198976828, -10.36322818467138340 ) ) ;
#32767 = CARTESIAN_POINT ( 'NONE',  ( 117.3343948109119737, -3.383040157471821630, -19.15922257007629170 ) ) ;
#32768 = CARTESIAN_POINT ( 'NONE',  ( 114.2330358795247776, -8.402594152722688392, -9.854619843455216355 ) ) ;
#32769 = CARTESIAN_POINT ( 'NONE',  ( 125.6732148109119862, -9.859900752359378018, -12.68260735090039759 ) ) ;
#32770 = ORIENTED_EDGE ( 'NONE', *, *, #3188, .F. ) ;
#32771 = CARTESIAN_POINT ( 'NONE',  ( 121.4187148109119789, -6.344957434206665248, -7.627207830600338134 ) ) ;
#32772 = CARTESIAN_POINT ( 'NONE',  ( 115.4831921295247952, 0.8980012041604618078, -13.39321520033831447 ) ) ;
#32773 = CARTESIAN_POINT ( 'NONE',  ( 110.8298327545248299, -6.936859964151250502, -8.388885654883777576 ) ) ;
#32774 = CARTESIAN_POINT ( 'NONE',  ( 72.54180985774836188, -55.08604862764417476, -34.50806356816917742 ) ) ;
#32775 = CARTESIAN_POINT ( 'NONE',  ( 112.8529881442453302, -7.894159318335828068, -9.358103419637847864 ) ) ;
#32776 = CIRCLE ( 'NONE', #37876, 2.999999999999998224 ) ;
#32777 = CARTESIAN_POINT ( 'NONE',  ( 138.2184548109119930, -3.657522433324904565, -16.24880879654457289 ) ) ;
#32778 = FACE_OUTER_BOUND ( 'NONE', #2508, .T. ) ;
#32779 = ORIENTED_EDGE ( 'NONE', *, *, #17770, .T. ) ;
#32780 = AXIS2_PLACEMENT_3D ( 'NONE', #27965, #21103, #20677 ) ;
#32781 = CARTESIAN_POINT ( 'NONE',  ( 125.3328548109119964, -0.8288870151387760510, -10.36305467784173118 ) ) ;
#32782 = CARTESIAN_POINT ( 'NONE',  ( 121.0630641859119976, -0.8832429491016019485, -18.19431474523657855 ) ) ;
#32783 = CARTESIAN_POINT ( 'NONE',  ( 123.9106423109119675, -9.959231468620755479, -10.70263013195267199 ) ) ;
#32784 = CARTESIAN_POINT ( 'NONE',  ( 111.7289948109119990, -2.109465145232937378, -8.734689011829464889 ) ) ;
#32785 = EDGE_CURVE ( 'NONE', #25810, #12184, #7246, .T. ) ;
#32786 = CARTESIAN_POINT ( 'NONE',  ( 105.5513952545248060, -9.868328341294098749, -15.46607636864997204 ) ) ;
#32787 = ORIENTED_EDGE ( 'NONE', *, *, #1678, .T. ) ;
#32788 = CARTESIAN_POINT ( 'NONE',  ( 115.1787814775786387, -9.988377603198976828, -10.36322818467138340 ) ) ;
#32789 = CARTESIAN_POINT ( 'NONE',  ( 88.68764736394132342, -11.19478773543180239, -14.07713050782770026 ) ) ;
#32790 = CARTESIAN_POINT ( 'NONE',  ( 119.4332814775786318, -8.899110576539710493, -16.42337572283490132 ) ) ;
#32791 = CARTESIAN_POINT ( 'NONE',  ( 115.3489614775786407, -0.8288870151387760510, -10.36305467784173118 ) ) ;
#32792 = LINE ( 'NONE', #1564, #19109 ) ;
#32793 = CARTESIAN_POINT ( 'NONE',  ( 125.3328548109119964, -0.8288870151387760510, -10.36305467784173118 ) ) ;
#32794 = CARTESIAN_POINT ( 'NONE',  ( 116.0388171295248014, 0.1403307496149613920, -13.39321520033831447 ) ) ;
#32795 = VECTOR ( 'NONE', #44322, 1000.000000000000114 ) ;
#32796 = CARTESIAN_POINT ( 'NONE',  ( 123.0070614775786169, 0.9020085738987339008, -11.91225656197089222 ) ) ;
#32797 = CARTESIAN_POINT ( 'NONE',  ( 64.66964420208745423, -0.6762465888536760561, -16.74452531359828100 ) ) ;
#32798 = ORIENTED_EDGE ( 'NONE', *, *, #11649, .F. ) ;
#32799 = EDGE_CURVE ( 'NONE', #23633, #37929, #10024, .T. ) ;
#32800 =( BOUNDED_SURFACE ( )  B_SPLINE_SURFACE ( 1, 2, ( 
 ( #22574, #11876, #35797, #29644, #11647, #12327, #18263, #22355, #25337, #39462, #4569, #7995, #18493, #43558, #5016, #22132, #26226, #7775, #21682, #32821, #35570, #32159, #42661, #36025, #4793, #32605, #927, #11432, #44698, #13458, #33726, #30100, #16881, #29872, #12552, #44016, #12778, #2724, #40135, #2496, #26680, #30772, #43787, #26459, #40591, #9350, #16650, #40361, #30545, #23260, #6151, #2045, #26904, #37143, #44466, #40824, #6386, #15969, #36916, #5917, #13231, #19839, #27132, #16425, #2954, #36692, #8900, #30321, #9125, #22798, #37381, #20071, #41056, #23495, #44247, #34179, #9813, #23722, #13005, #5462, #37612, #16196, #20294, #33957, #19382, #33270, #9579, #23029, #5687, #19606, #33490, #2268, #14956, #14283, #21346, #4233, #38887, #18151, #24765, #18601, #24551, #38438, #814, #372, #21571, #3779, #39121, #596, #35458, #34995, #32046, #38656, #42781, #32272, #14506, #25449, #21794, #7656, #39351, #35688, #7425, #4463, #18384, #28202, #1040, #28419, #14733, #42109, #8119, #28645, #7208, #32492, #42551, #21121, #28868, #17703, #11542, #22020, #11313, #10870, #35914, #17927, #1267, #31603, #25223, #35230, #4005, #31826, #42330, #11091, #4680, #7888, #24992, #27980, #41884, #10646, #1936, #29987, #40254, #22241, #1485, #15633, #32713, #42995, #5364, #19723, #15407, #8566, #29311, #43224, #11991, #9020, #12445, #25893, #33381, #22918, #23153, #15862, #43904, #36810, #36137, #39797, #29537, #22466, #11762, #19281, #33609, #15180, #8786, #5132, #37035, #4905, #36360, #19048, #32935, #5578, #18821, #19502, #43453, #26346, #1710, #29758, #12218, #2152, #43670, #26571, #26116, #40021, #22692, #16082, #36589, #12673, #33160, #5804, #25672, #29083, #40485, #9244, #39577, #8340, #44812, #10154, #30890, #37730, #41618, #34516, #37954, #34076, #6948, #24062, #23612, #20639, #13570, #3294, #45031, #41170, #31107, #6728, #13351, #37498, #17217, #13791, #33844, #40942, #23843, #27255, #6500, #44360, #38169, #44137, #12902, #20415, #19955, #9930, #23379, #27480, #20192 ),
 ( #20853, #27703, #34299, #10374, #3072, #6272, #17001, #30441, #2386, #30217, #9698, #24283, #2843, #41399, #2613, #37261, #16314, #16772, #6033, #26798, #30667, #40708, #9467, #16545, #27027, #13121, #44588, #28362, #39070, #14456, #7605, #25172, #99, #3954, #31994, #14231, #38383, #28147, #992, #8064, #11264, #42275, #32219, #38836, #24711, #24940, #17654, #34731, #17431, #42057, #14907, #10815, #11038, #7156, #10596, #3514, #38600, #21067, #35406, #35177, #21519, #544, #4181, #7377, #31324, #28818, #18098, #7839, #756, #28593, #21293, #14012, #42504, #17876, #39296, #41836, #24499, #27927, #34945, #3731, #18326, #31550, #31773, #14679, #21745, #318, #35635, #4411, #42728, #11493, #25398, #22416, #22639, #32666, #2102, #18776, #35856, #39969, #4630, #29037, #29705, #43618, #29261, #21969, #8289, #29937, #36087, #15355, #5310, #40199, #8732, #18551, #19226, #1434, #5525, #42946, #19445, #12392, #39527, #43172, #39745, #15577, #36536, #32443, #1217, #16030, #40430, #36757, #43851, #11941, #33106, #8965, #4858, #33328, #1877, #15804, #25837, #15131, #12623, #29482, #26521, #11711, #8512, #36309, #22191, #26065, #5079, #26291, #43395, #12163, #25622, #18994, #32882, #1656, #22864, #27200, #37897, #5746, #13518, #40886, #6675, #3019, #20137, #20582, #16941, #33788, #30836, #44759, #40654, #27427, #26966, #30612, #23320, #34461, #2791, #19667, #44983, #34023, #33554, #41349, #2332, #10105, #24009, #16718, #37205, #17166, #44311, #13741, #16262, #44529, #26748, #2560, #5978, #9409, #19903, #3240, #6452, #16489, #31055, #27650, #9191, #41118, #23097, #34247, #30165, #30389, #9640, #13066, #36978, #13292, #44082, #12847, #9877, #23562, #37443, #6215, #23787, #37677, #20360, #4125, #31272, #18045, #42001, #7552, #3468, #28311, #31495, #31939, #42223, #7784, #17383, #38332, #7323, #705, #38548, #14625, #35120, #4351, #38117, #41565, #21243, #45, #18271, #38781, #21467, #28543, #24888, #31718, #35578, #42447, #11213, #28092, #936, #25118, #17602, #39014, #35350 ) ),
 .UNSPECIFIED., .F., .F., .F. ) 
 B_SPLINE_SURFACE_WITH_KNOTS ( ( 2, 2 ),
 ( 3, 2, 2, 2, 2, 2, 2, 2, 2, 2, 2, 2, 2, 2, 2, 2, 2, 2, 2, 2, 2, 2, 2, 2, 2, 2, 2, 2, 2, 2, 2, 2, 2, 2, 2, 2, 2, 2, 2, 2, 2, 2, 2, 2, 2, 2, 2, 2, 2, 2, 2, 2, 2, 2, 2, 2, 2, 2, 2, 2, 2, 2, 2, 2, 2, 2, 2, 2, 2, 2, 2, 2, 2, 2, 2, 2, 2, 2, 2, 2, 2, 2, 2, 2, 2, 2, 2, 2, 2, 2, 2, 2, 2, 2, 2, 2, 2, 2, 2, 2, 2, 2, 2, 2, 2, 2, 2, 2, 2, 2, 2, 2, 2, 2, 2, 2, 2, 2, 2, 2, 2, 2, 2, 2, 2, 2, 2, 2, 3 ),
 ( 0.000000000000000000, 1.000000000000000000 ),
 ( 0.000000000000000000, 0.007812500000000000000, 0.01562500000000000000, 0.02343750000000000000, 0.03125000000000000000, 0.03906250000000000000, 0.04687500000000000000, 0.05468750000000000000, 0.06250000000000000000, 0.07031250000000000000, 0.07812500000000000000, 0.08593750000000000000, 0.09375000000000000000, 0.1015625000000000000, 0.1093750000000000000, 0.1171875000000000000, 0.1250000000000000000, 0.1328125000000000000, 0.1406250000000000000, 0.1484375000000000000, 0.1562500000000000000, 0.1640625000000000000, 0.1718750000000000000, 0.1796875000000000000, 0.1875000000000000000, 0.1953125000000000000, 0.2031250000000000000, 0.2109375000000000000, 0.2187500000000000000, 0.2265625000000000000, 0.2343750000000000000, 0.2421875000000000000, 0.2500000000000000000, 0.2578125000000000000, 0.2656250000000000000, 0.2734375000000000000, 0.2812500000000000000, 0.2890625000000000000, 0.2968750000000000000, 0.3046875000000000000, 0.3125000000000000000, 0.3203125000000000000, 0.3281250000000000000, 0.3359375000000000000, 0.3437500000000000000, 0.3515625000000000000, 0.3593750000000000000, 0.3671875000000000000, 0.3750000000000000000, 0.3828125000000000000, 0.3906250000000000000, 0.3984375000000000000, 0.4062500000000000000, 0.4140625000000000000, 0.4218750000000000000, 0.4296875000000000000, 0.4375000000000000000, 0.4453125000000000000, 0.4531250000000000000, 0.4609375000000000000, 0.4687500000000000000, 0.4765625000000000000, 0.4843750000000000000, 0.4921875000000000000, 0.5000000000000000000, 0.5078125000000000000, 0.5156250000000000000, 0.5234375000000000000, 0.5312500000000000000, 0.5390625000000000000, 0.5468750000000000000, 0.5546875000000000000, 0.5625000000000000000, 0.5703125000000000000, 0.5781250000000000000, 0.5859375000000000000, 0.5937500000000000000, 0.6015625000000000000, 0.6093750000000000000, 0.6171875000000000000, 0.6250000000000000000, 0.6328125000000000000, 0.6406250000000000000, 0.6484375000000000000, 0.6562500000000000000, 0.6640625000000000000, 0.6718750000000000000, 0.6796875000000000000, 0.6875000000000000000, 0.6953125000000000000, 0.7031250000000000000, 0.7109375000000000000, 0.7187500000000000000, 0.7265625000000000000, 0.7343750000000000000, 0.7421875000000000000, 0.7500000000000000000, 0.7578125000000000000, 0.7656250000000000000, 0.7734375000000000000, 0.7812500000000000000, 0.7890625000000000000, 0.7968750000000000000, 0.8046875000000000000, 0.8125000000000000000, 0.8203125000000000000, 0.8281250000000000000, 0.8359375000000000000, 0.8437500000000000000, 0.8515625000000000000, 0.8593750000000000000, 0.8671875000000000000, 0.8750000000000000000, 0.8828125000000000000, 0.8906250000000000000, 0.8984375000000000000, 0.9062500000000000000, 0.9140625000000000000, 0.9218750000000000000, 0.9296875000000000000, 0.9375000000000000000, 0.9453125000000000000, 0.9531250000000000000, 0.9609375000000000000, 0.9687500000000000000, 0.9765625000000000000, 0.9843750000000000000, 0.9921875000000000000, 1.000000000000000000 ),
 .UNSPECIFIED. ) 
 GEOMETRIC_REPRESENTATION_ITEM ( )  RATIONAL_B_SPLINE_SURFACE ( (
 ( 1.000000000000000000, 0.9238795325112869605, 1.000000000000000000, 0.9238795325112869605, 1.000000000000000000, 0.9238795325112869605, 1.000000000000000000, 0.9238795325112869605, 1.000000000000000000, 0.9238795325112869605, 1.000000000000000000, 0.9238795325112869605, 1.000000000000000000, 0.9238795325112869605, 1.000000000000000000, 0.9238795325112869605, 1.000000000000000000, 0.9238795325112869605, 1.000000000000000000, 0.9238795325112869605, 1.000000000000000000, 0.9238795325112869605, 1.000000000000000000, 0.9238795325112869605, 1.000000000000000000, 0.9238795325112869605, 1.000000000000000000, 0.9238795325112869605, 1.000000000000000000, 0.9238795325112869605, 1.000000000000000000, 0.9238795325112869605, 1.000000000000000000, 0.9238795325112869605, 1.000000000000000000, 0.9238795325112869605, 1.000000000000000000, 0.9238795325112869605, 1.000000000000000000, 0.9238795325112869605, 1.000000000000000000, 0.9238795325112869605, 1.000000000000000000, 0.9238795325112869605, 1.000000000000000000, 0.9238795325112869605, 1.000000000000000000, 0.9238795325112869605, 1.000000000000000000, 0.9238795325112869605, 1.000000000000000000, 0.9238795325112869605, 1.000000000000000000, 0.9238795325112869605, 1.000000000000000000, 0.9238795325112869605, 1.000000000000000000, 0.9238795325112869605, 1.000000000000000000, 0.9238795325112869605, 1.000000000000000000, 0.9238795325112869605, 1.000000000000000000, 0.9238795325112869605, 1.000000000000000000, 0.9238795325112869605, 1.000000000000000000, 0.9238795325112869605, 1.000000000000000000, 0.9238795325112869605, 1.000000000000000000, 0.9238795325112869605, 1.000000000000000000, 0.9238795325112869605, 1.000000000000000000, 0.9238795325112869605, 1.000000000000000000, 0.9238795325112869605, 1.000000000000000000, 0.9238795325112869605, 1.000000000000000000, 0.9238795325112869605, 1.000000000000000000, 0.9238795325112869605, 1.000000000000000000, 0.9238795325112869605, 1.000000000000000000, 0.9238795325112869605, 1.000000000000000000, 0.9238795325112869605, 1.000000000000000000, 0.9238795325112869605, 1.000000000000000000, 0.9238795325112869605, 1.000000000000000000, 0.9238795325112869605, 1.000000000000000000, 0.9238795325112869605, 1.000000000000000000, 0.9238795325112869605, 1.000000000000000000, 0.9238795325112869605, 1.000000000000000000, 0.9238795325112869605, 1.000000000000000000, 0.9238795325112869605, 1.000000000000000000, 0.9238795325112869605, 1.000000000000000000, 0.9238795325112869605, 1.000000000000000000, 0.9238795325112869605, 1.000000000000000000, 0.9238795325112869605, 1.000000000000000000, 0.9238795325112869605, 1.000000000000000000, 0.9238795325112869605, 1.000000000000000000, 0.9238795325112869605, 1.000000000000000000, 0.9238795325112869605, 1.000000000000000000, 0.9238795325112869605, 1.000000000000000000, 0.9238795325112869605, 1.000000000000000000, 0.9238795325112869605, 1.000000000000000000, 0.9238795325112869605, 1.000000000000000000, 0.9238795325112869605, 1.000000000000000000, 0.9238795325112869605, 1.000000000000000000, 0.9238795325112869605, 1.000000000000000000, 0.9238795325112869605, 1.000000000000000000, 0.9238795325112869605, 1.000000000000000000, 0.9238795325112869605, 1.000000000000000000, 0.9238795325112869605, 1.000000000000000000, 0.9238795325112869605, 1.000000000000000000, 0.9238795325112869605, 1.000000000000000000, 0.9238795325112869605, 1.000000000000000000, 0.9238795325112869605, 1.000000000000000000, 0.9238795325112869605, 1.000000000000000000, 0.9238795325112869605, 1.000000000000000000, 0.9238795325112869605, 1.000000000000000000, 0.9238795325112869605, 1.000000000000000000, 0.9238795325112869605, 1.000000000000000000, 0.9238795325112869605, 1.000000000000000000, 0.9238795325112869605, 1.000000000000000000, 0.9238795325112869605, 1.000000000000000000, 0.9238795325112869605, 1.000000000000000000, 0.9238795325112869605, 1.000000000000000000, 0.9238795325112869605, 1.000000000000000000, 0.9238795325112869605, 1.000000000000000000, 0.9238795325112869605, 1.000000000000000000, 0.9238795325112869605, 1.000000000000000000, 0.9238795325112869605, 1.000000000000000000, 0.9238795325112869605, 1.000000000000000000, 0.9238795325112869605, 1.000000000000000000, 0.9238795325112869605, 1.000000000000000000, 0.9238795325112869605, 1.000000000000000000, 0.9238795325112869605, 1.000000000000000000, 0.9238795325112869605, 1.000000000000000000, 0.9238795325112869605, 1.000000000000000000, 0.9238795325112869605, 1.000000000000000000, 0.9238795325112869605, 1.000000000000000000, 0.9238795325112869605, 1.000000000000000000, 0.9238795325112869605, 1.000000000000000000, 0.9238795325112869605, 1.000000000000000000, 0.9238795325112869605, 1.000000000000000000, 0.9238795325112869605, 1.000000000000000000, 0.9238795325112869605, 1.000000000000000000, 0.9238795325112869605, 1.000000000000000000, 0.9238795325112869605, 1.000000000000000000, 0.9238795325112869605, 1.000000000000000000, 0.9238795325112869605, 1.000000000000000000, 0.9238795325112869605, 1.000000000000000000, 0.9238795325112869605, 1.000000000000000000, 0.9238795325112869605, 1.000000000000000000, 0.9238795325112869605, 1.000000000000000000, 0.9238795325112869605, 1.000000000000000000, 0.9238795325112869605, 1.000000000000000000, 0.9238795325112869605, 1.000000000000000000, 0.9238795325112869605, 1.000000000000000000, 0.9238795325112869605, 1.000000000000000000, 0.9238795325112869605, 1.000000000000000000, 0.9238795325112869605, 1.000000000000000000, 0.9238795325112869605, 1.000000000000000000, 0.9238795325112869605, 1.000000000000000000, 0.9238795325112869605, 1.000000000000000000, 0.9238795325112869605, 1.000000000000000000, 0.9238795325112869605, 1.000000000000000000, 0.9238795325112869605, 1.000000000000000000, 0.9238795325112869605, 1.000000000000000000),
 ( 1.000000000000000000, 0.9238795325112869605, 1.000000000000000000, 0.9238795325112869605, 1.000000000000000000, 0.9238795325112869605, 1.000000000000000000, 0.9238795325112869605, 1.000000000000000000, 0.9238795325112869605, 1.000000000000000000, 0.9238795325112869605, 1.000000000000000000, 0.9238795325112869605, 1.000000000000000000, 0.9238795325112869605, 1.000000000000000000, 0.9238795325112869605, 1.000000000000000000, 0.9238795325112869605, 1.000000000000000000, 0.9238795325112869605, 1.000000000000000000, 0.9238795325112869605, 1.000000000000000000, 0.9238795325112869605, 1.000000000000000000, 0.9238795325112869605, 1.000000000000000000, 0.9238795325112869605, 1.000000000000000000, 0.9238795325112869605, 1.000000000000000000, 0.9238795325112869605, 1.000000000000000000, 0.9238795325112869605, 1.000000000000000000, 0.9238795325112869605, 1.000000000000000000, 0.9238795325112869605, 1.000000000000000000, 0.9238795325112869605, 1.000000000000000000, 0.9238795325112869605, 1.000000000000000000, 0.9238795325112869605, 1.000000000000000000, 0.9238795325112869605, 1.000000000000000000, 0.9238795325112869605, 1.000000000000000000, 0.9238795325112869605, 1.000000000000000000, 0.9238795325112869605, 1.000000000000000000, 0.9238795325112869605, 1.000000000000000000, 0.9238795325112869605, 1.000000000000000000, 0.9238795325112869605, 1.000000000000000000, 0.9238795325112869605, 1.000000000000000000, 0.9238795325112869605, 1.000000000000000000, 0.9238795325112869605, 1.000000000000000000, 0.9238795325112869605, 1.000000000000000000, 0.9238795325112869605, 1.000000000000000000, 0.9238795325112869605, 1.000000000000000000, 0.9238795325112869605, 1.000000000000000000, 0.9238795325112869605, 1.000000000000000000, 0.9238795325112869605, 1.000000000000000000, 0.9238795325112869605, 1.000000000000000000, 0.9238795325112869605, 1.000000000000000000, 0.9238795325112869605, 1.000000000000000000, 0.9238795325112869605, 1.000000000000000000, 0.9238795325112869605, 1.000000000000000000, 0.9238795325112869605, 1.000000000000000000, 0.9238795325112869605, 1.000000000000000000, 0.9238795325112869605, 1.000000000000000000, 0.9238795325112869605, 1.000000000000000000, 0.9238795325112869605, 1.000000000000000000, 0.9238795325112869605, 1.000000000000000000, 0.9238795325112869605, 1.000000000000000000, 0.9238795325112869605, 1.000000000000000000, 0.9238795325112869605, 1.000000000000000000, 0.9238795325112869605, 1.000000000000000000, 0.9238795325112869605, 1.000000000000000000, 0.9238795325112869605, 1.000000000000000000, 0.9238795325112869605, 1.000000000000000000, 0.9238795325112869605, 1.000000000000000000, 0.9238795325112869605, 1.000000000000000000, 0.9238795325112869605, 1.000000000000000000, 0.9238795325112869605, 1.000000000000000000, 0.9238795325112869605, 1.000000000000000000, 0.9238795325112869605, 1.000000000000000000, 0.9238795325112869605, 1.000000000000000000, 0.9238795325112869605, 1.000000000000000000, 0.9238795325112869605, 1.000000000000000000, 0.9238795325112869605, 1.000000000000000000, 0.9238795325112869605, 1.000000000000000000, 0.9238795325112869605, 1.000000000000000000, 0.9238795325112869605, 1.000000000000000000, 0.9238795325112869605, 1.000000000000000000, 0.9238795325112869605, 1.000000000000000000, 0.9238795325112869605, 1.000000000000000000, 0.9238795325112869605, 1.000000000000000000, 0.9238795325112869605, 1.000000000000000000, 0.9238795325112869605, 1.000000000000000000, 0.9238795325112869605, 1.000000000000000000, 0.9238795325112869605, 1.000000000000000000, 0.9238795325112869605, 1.000000000000000000, 0.9238795325112869605, 1.000000000000000000, 0.9238795325112869605, 1.000000000000000000, 0.9238795325112869605, 1.000000000000000000, 0.9238795325112869605, 1.000000000000000000, 0.9238795325112869605, 1.000000000000000000, 0.9238795325112869605, 1.000000000000000000, 0.9238795325112869605, 1.000000000000000000, 0.9238795325112869605, 1.000000000000000000, 0.9238795325112869605, 1.000000000000000000, 0.9238795325112869605, 1.000000000000000000, 0.9238795325112869605, 1.000000000000000000, 0.9238795325112869605, 1.000000000000000000, 0.9238795325112869605, 1.000000000000000000, 0.9238795325112869605, 1.000000000000000000, 0.9238795325112869605, 1.000000000000000000, 0.9238795325112869605, 1.000000000000000000, 0.9238795325112869605, 1.000000000000000000, 0.9238795325112869605, 1.000000000000000000, 0.9238795325112869605, 1.000000000000000000, 0.9238795325112869605, 1.000000000000000000, 0.9238795325112869605, 1.000000000000000000, 0.9238795325112869605, 1.000000000000000000, 0.9238795325112869605, 1.000000000000000000, 0.9238795325112869605, 1.000000000000000000, 0.9238795325112869605, 1.000000000000000000, 0.9238795325112869605, 1.000000000000000000, 0.9238795325112869605, 1.000000000000000000, 0.9238795325112869605, 1.000000000000000000, 0.9238795325112869605, 1.000000000000000000, 0.9238795325112869605, 1.000000000000000000, 0.9238795325112869605, 1.000000000000000000, 0.9238795325112869605, 1.000000000000000000, 0.9238795325112869605, 1.000000000000000000, 0.9238795325112869605, 1.000000000000000000, 0.9238795325112869605, 1.000000000000000000, 0.9238795325112869605, 1.000000000000000000, 0.9238795325112869605, 1.000000000000000000, 0.9238795325112869605, 1.000000000000000000, 0.9238795325112869605, 1.000000000000000000, 0.9238795325112869605, 1.000000000000000000, 0.9238795325112869605, 1.000000000000000000, 0.9238795325112869605, 1.000000000000000000, 0.9238795325112869605, 1.000000000000000000, 0.9238795325112869605, 1.000000000000000000, 0.9238795325112869605, 1.000000000000000000, 0.9238795325112869605, 1.000000000000000000, 0.9238795325112869605, 1.000000000000000000, 0.9238795325112869605, 1.000000000000000000, 0.9238795325112869605, 1.000000000000000000) ) ) 
 REPRESENTATION_ITEM ( '' )  SURFACE ( )  );
#32801 = CARTESIAN_POINT ( 'NONE',  ( 112.6260814775786514, -9.261995988541697145, -16.69588392320189030 ) ) ;
#32802 = EDGE_CURVE ( 'NONE', #14918, #34483, #27857, .T. ) ;
#32803 = ADVANCED_FACE ( 'NONE', ( #17741 ), #40223, .T. ) ;
#32804 = CARTESIAN_POINT ( 'NONE',  ( 126.1270281442452870, -10.30919188438810075, -12.61870101168855918 ) ) ;
#32805 = CARTESIAN_POINT ( 'NONE',  ( 78.93021946355167984, -3.662536865724447921, -14.39321520033831625 ) ) ;
#32806 = CARTESIAN_POINT ( 'NONE',  ( 125.2761281442453054, 0.4262465694468514643, -12.03445270309931736 ) ) ;
#32807 = ORIENTED_EDGE ( 'NONE', *, *, #31462, .T. ) ;
#32808 = CARTESIAN_POINT ( 'NONE',  ( 118.6958348109119754, -6.344957434206665248, -7.627207830600338134 ) ) ;
#32809 = LINE ( 'NONE', #18918, #30303 ) ;
#32810 = CARTESIAN_POINT ( 'NONE',  ( 74.47157298427187300, -3.053873105668316601, -16.39321520033831447 ) ) ;
#32811 = VECTOR ( 'NONE', #9138, 1000.000000000000114 ) ;
#32812 = CARTESIAN_POINT ( 'NONE',  ( 115.3968144685026829, 0.6938714319017630361, -14.64321520033829849 ) ) ;
#32813 = CARTESIAN_POINT ( 'NONE',  ( 111.4321701211256652, -2.490435581280318278, -17.80295943339125486 ) ) ;
#32814 = CARTESIAN_POINT ( 'NONE',  ( 112.5126281442453120, 0.1319031606808879209, -14.10382304977623669 ) ) ;
#32815 = DIRECTION ( 'NONE',  ( 0.000000000000000000, -0.3818493186865927203, 0.9242245927363029745 ) ) ;
#32816 = CARTESIAN_POINT ( 'NONE',  ( 124.9868051361299166, -1.575707845324203493, -20.23615509330177531 ) ) ;
#32817 = CARTESIAN_POINT ( 'NONE',  ( 113.6471614775786492, -4.153390946401321671, -8.397313243818183892 ) ) ;
#32818 = CARTESIAN_POINT ( 'NONE',  ( 125.7299414775786346, -10.15424416112533912, -14.75197769757731336 ) ) ;
#32819 = CARTESIAN_POINT ( 'NONE',  ( 116.7131856665309186, -6.970574376166484676, -18.05871830232659292 ) ) ;
#32820 = CARTESIAN_POINT ( 'NONE',  ( 125.2194014775786286, 0.1319031606808879209, -14.10382304977623669 ) ) ;
#32821 = CARTESIAN_POINT ( 'NONE',  ( 113.2500748109119968, -3.505236298600246325, -18.68346056562440793 ) ) ;
#32822 = CARTESIAN_POINT ( 'NONE',  ( 119.0929214775786278, -5.638512984488999180, -18.83840828888717311 ) ) ;
#32823 = CARTESIAN_POINT ( 'NONE',  ( 121.5888948109119809, -10.30919188438810075, -12.61870101168855918 ) ) ;
#32824 = ORIENTED_EDGE ( 'NONE', *, *, #10180, .T. ) ;
#32825 = CARTESIAN_POINT ( 'NONE',  ( -1.307700928565892706, -16.07486664983353819, -8.593215200338315540 ) ) ;
#32826 = CARTESIAN_POINT ( 'NONE',  ( 114.3024890045248156, 0.8980012041604421569, -15.77991374673208469 ) ) ;
#32827 = EDGE_CURVE ( 'NONE', #13151, #1972, #20944, .T. ) ;
#32828 = CARTESIAN_POINT ( 'NONE',  ( 112.2188952545247531, -9.868328341294098749, -15.46607636864997204 ) ) ;
#32829 = CARTESIAN_POINT ( 'NONE',  ( 109.0935046295247872, -4.863998795839590272, -18.39754474579285315 ) ) ;
#32830 = AXIS2_PLACEMENT_3D ( 'NONE', #43286, #19113, #25735 ) ;
#32831 = CARTESIAN_POINT ( 'NONE',  ( 126.8396850857652396, -9.909566493429444733, -11.73595350948055582 ) ) ;
#32832 = CARTESIAN_POINT ( 'NONE',  ( 116.0864081442453113, -9.988377603198976828, -10.36322818467138340 ) ) ;
#32833 = ORIENTED_EDGE ( 'NONE', *, *, #27537, .T. ) ;
#32834 = CARTESIAN_POINT ( 'NONE',  ( 107.9128015045248219, -2.477300249445798297, -7.631215200338321125 ) ) ;
#32835 = DIRECTION ( 'NONE',  ( -1.000000000000000000, 0.000000000000000000, 0.000000000000000000 ) ) ;
#32836 = CARTESIAN_POINT ( 'NONE',  ( 121.9470836909669913, -25.99489077589524300, -13.39321520033831447 ) ) ;
#32837 = EDGE_CURVE ( 'NONE', #16463, #12130, #6004, .T. ) ;
#32838 = CARTESIAN_POINT ( 'NONE',  ( 112.7395348109119766, -5.638512984488999180, -18.83840828888717311 ) ) ;
#32839 = CARTESIAN_POINT ( 'NONE',  ( 121.1350814775786233, 0.5811942927096110934, -14.16772938898807510 ) ) ;
#32840 = EDGE_CURVE ( 'NONE', #39890, #14756, #38041, .T. ) ;
#32841 = CARTESIAN_POINT ( 'NONE',  ( 110.1353015045248469, -2.477300249445798297, -7.631215200338321125 ) ) ;
#32842 = DIRECTION ( 'NONE',  ( 0.000000000000000000, 0.000000000000000000, -1.000000000000000000 ) ) ;
#32843 = ORIENTED_EDGE ( 'NONE', *, *, #2498, .T. ) ;
#32844 = CARTESIAN_POINT ( 'NONE',  ( 121.1918081442452859, -10.15424416112535155, -14.75197769757726185 ) ) ;
#32845 = CARTESIAN_POINT ( 'NONE',  ( 118.4689281442453392, -10.15424416112533912, -14.75197769757731336 ) ) ;
#32846 = CARTESIAN_POINT ( 'NONE',  ( 117.5613014775786525, 0.9020085738987339008, -11.91225656197089222 ) ) ;
#32847 = CARTESIAN_POINT ( 'NONE',  ( 112.2857214775786474, -4.089484607189486809, -7.948022111789456723 ) ) ;
#32848 = DIRECTION ( 'NONE',  ( 1.000000000000000000, 0.000000000000000000, 0.000000000000000000 ) ) ;
#32849 = CARTESIAN_POINT ( 'NONE',  ( 125.0492214775786266, -3.505236298600246325, -18.68346056562440793 ) ) ;
#32850 = CARTESIAN_POINT ( 'NONE',  ( 114.4980614775786734, -2.084020599724406786, -8.691656652584148546 ) ) ;
#32851 = VERTEX_POINT ( 'NONE', #13876 ) ;
#32852 = CARTESIAN_POINT ( 'NONE',  ( 124.3273610609119686, -6.340755971794695078, -8.611740276972781771 ) ) ;
#32853 = DIRECTION ( 'NONE',  ( 0.9609149988134837450, -0.1028163501681639419, 0.2570431154366518145 ) ) ;
#32854 = CARTESIAN_POINT ( 'NONE',  ( 117.3911214775786505, -7.894159318335828068, -9.358103419637847864 ) ) ;
#32855 = VERTEX_POINT ( 'NONE', #20278 ) ;
#32856 = CARTESIAN_POINT ( 'NONE',  ( 120.4379860609119675, -3.387241619883791355, -18.17469012370385073 ) ) ;
#32857 = ADVANCED_FACE ( 'NONE', ( #2935 ), #27459, .F. ) ;
#32858 = CARTESIAN_POINT ( 'NONE',  ( 116.3133148109119759, -7.893985811506177619, -18.51759400769804742 ) ) ;
#32859 = CARTESIAN_POINT ( 'NONE',  ( 107.6349890045248401, -9.868328341294098749, -11.32035403202665869 ) ) ;
#32860 = CARTESIAN_POINT ( 'NONE',  ( 113.3068014775786594, -1.833838273342658809, -17.42832698103878286 ) ) ;
#32861 = VERTEX_POINT ( 'NONE', #9056 ) ;
#32862 = ORIENTED_EDGE ( 'NONE', *, *, #3022, .T. ) ;
#32863 = CARTESIAN_POINT ( 'NONE',  ( 122.0427081442452817, -9.859900752359378018, -12.68260735090039759 ) ) ;
#32864 = B_SPLINE_CURVE_WITH_KNOTS ( 'NONE', 3,
 ( #20681, #31593, #34558, #21337, #7647, #21562, #24541, #3342, #31151, #20901, #10637, #362, #45071, #13831, #3996, #17918, #27746, #10419, #24326, #34775, #3557, #17471, #31368, #140, #41876, #21788, #36127, #36578, #39786, #43215, #43442, #22680, #22231, #15620, #8332, #5354, #25663, #11754, #18593, #26104, #25884, #36350, #8555 ),
 .UNSPECIFIED., .F., .F.,
 ( 4, 2, 2, 1, 2, 2, 2, 2, 1, 1, 2, 2, 2, 2, 1, 1, 1, 2, 2, 2, 1, 1, 1, 2, 2, 4 ),
 ( 0.000000000000000000, 0.1249999999999658051, 0.1874999999999473199, 0.2187499999999395206, 0.2343749999999356071, 0.2499999999999317213, 0.3749999999998905320, 0.4374999999998702149, 0.4687499999998600564, 0.4843749999998577249, 0.4921874999998566147, 0.4999999999998554490, 0.6249999999998734346, 0.6874999999998797628, 0.7187499999998828715, 0.7343749999998823164, 0.7421874999998844258, 0.7460937499998878675, 0.7499999999998911981, 0.8124999999999091838, 0.8437499999999180655, 0.8593749999999241718, 0.8671874999999273914, 0.8710937499999307221, 0.8749999999999339417, 1.000000000000000000 ),
 .UNSPECIFIED. ) ;
#32865 = CARTESIAN_POINT ( 'NONE',  ( 117.0507614775786465, 0.1319031606808879209, -14.10382304977623669 ) ) ;
#32866 = CARTESIAN_POINT ( 'NONE',  ( 85.82015659721905365, -26.75858941326842810, -11.54476601486570964 ) ) ;
#32867 = ORIENTED_EDGE ( 'NONE', *, *, #33364, .T. ) ;
#32868 = DIRECTION ( 'NONE',  ( -1.000000000000000000, 0.000000000000000000, 0.000000000000000000 ) ) ;
#32869 = CARTESIAN_POINT ( 'NONE',  ( 62.10597993692722696, -65.36243247205813134, -44.73744814048375673 ) ) ;
#32870 = CARTESIAN_POINT ( 'NONE',  ( 107.8433483795247838, -0.7896495226426338832, -9.318865927141430916 ) ) ;
#32871 = CARTESIAN_POINT ( 'NONE',  ( 117.6747548109119919, -1.834011780172310813, -8.268836392978581529 ) ) ;
#32873 = CARTESIAN_POINT ( 'NONE',  ( 116.9373081442452929, -1.833838273342659253, -17.42832698103878286 ) ) ;
#32872 = CARTESIAN_POINT ( 'NONE',  ( 115.9162281442453235, -4.089484607189486809, -7.948022111789456723 ) ) ;
#32874 = CARTESIAN_POINT ( 'NONE',  ( 121.7590748109119687, -2.084020599724406786, -8.691656652584148546 ) ) ;
#32875 = CARTESIAN_POINT ( 'NONE',  ( 79.05243529145373316, 4.793396140045460108, -12.14321520033831625 ) ) ;
#32876 = VERTEX_POINT ( 'NONE', #22956 ) ;
#32877 = CARTESIAN_POINT ( 'NONE',  ( 120.7947214775786193, -0.8288870151387760510, -10.36305467784173118 ) ) ;
#32878 = CARTESIAN_POINT ( 'NONE',  ( 125.7299414775786346, -10.15424416112533912, -14.75197769757731336 ) ) ;
#32879 = CARTESIAN_POINT ( 'NONE',  ( 111.1770983795247787, -0.7896495226426338832, -9.318865927141430916 ) ) ;
#32880 = CARTESIAN_POINT ( 'NONE',  ( 135.3184548109119874, 0.7167481258041168424, -11.18974888642104659 ) ) ;
#32881 = CARTESIAN_POINT ( 'NONE',  ( 110.2742077545248094, -7.250697342233347165, -7.631215200338321125 ) ) ;
#32882 = CARTESIAN_POINT ( 'NONE',  ( 120.3409081442453044, -0.4660016031367893996, -10.09054647747474043 ) ) ;
#32883 = ORIENTED_EDGE ( 'NONE', *, *, #3646, .F. ) ;
#32884 = CARTESIAN_POINT ( 'NONE',  ( 121.4754414775786131, -8.166667518702819706, -8.995218007635861213 ) ) ;
#32885 = DIRECTION ( 'NONE',  ( 0.000000000000000000, -0.3818493186865927203, 0.9242245927363029745 ) ) ;
#32886 = CARTESIAN_POINT ( 'NONE',  ( 106.2459265045248173, -7.250697342233347165, -19.15521520033831138 ) ) ;
#32887 = CARTESIAN_POINT ( 'NONE',  ( 116.0296814775786345, -8.166667518702817929, -8.995218007635861213 ) ) ;
#32888 = CARTESIAN_POINT ( 'NONE',  ( 119.0361948109119652, -7.893985811506177619, -18.51759400769804742 ) ) ;
#32889 = CARTESIAN_POINT ( 'NONE',  ( 117.1901992640912908, -11.08276418064105862, -5.403345540909042732 ) ) ;
#32890 = EDGE_LOOP ( 'NONE', ( #33826, #19271, #19553, #31185, #5415, #27956 ) ) ;
#32891 = CARTESIAN_POINT ( 'NONE',  ( -2.105898499509477162, -6.916383580925556274, -7.785241425804852788 ) ) ;
#32892 = CARTESIAN_POINT ( 'NONE',  ( 109.2295201380737097, -10.43748051877606464, -13.15408167448229193 ) ) ;
#32893 = CARTESIAN_POINT ( 'NONE',  ( 119.8303681442453126, 0.4262465694468514643, -12.03445270309931736 ) ) ;
#32894 = CARTESIAN_POINT ( 'NONE',  ( 110.4825671295247815, 0.1403307496149613920, -13.39321520033831447 ) ) ;
#32895 = CARTESIAN_POINT ( 'NONE',  ( 115.3442858795247759, -8.402594152722688392, -9.854619843455216355 ) ) ;
#32896 = CARTESIAN_POINT ( 'NONE',  ( 115.1787814775786387, -0.1624402480850797581, -16.17319339645315424 ) ) ;
#32897 = DIRECTION ( 'NONE',  ( 0.000000000000000000, 0.000000000000000000, -1.000000000000000000 ) ) ;
#32898 = CARTESIAN_POINT ( 'NONE',  ( 70.76896822304256318, -26.49227693691338814, -5.467054258871666406 ) ) ;
#32899 = CARTESIAN_POINT ( 'NONE',  ( 112.9664414775786412, -9.859900752359374465, -12.68260735090039404 ) ) ;
#32900 = CARTESIAN_POINT ( 'NONE',  ( 119.8303681442453126, -10.63000616557722466, -14.87417383870573495 ) ) ;
#32902 = ORIENTED_EDGE ( 'NONE', *, *, #35208, .T. ) ;
#32901 = EDGE_CURVE ( 'NONE', #36847, #14451, #12482, .T. ) ;
#32903 = CARTESIAN_POINT ( 'NONE',  ( 119.2631014775786298, -9.565557343593413364, -10.61323700422348004 ) ) ;
#32904 = AXIS2_PLACEMENT_3D ( 'NONE', #2786, #20961, #7050 ) ;
#32905 = CARTESIAN_POINT ( 'NONE',  ( 113.8173414775786512, 0.2603800115204892296, -16.42320221600525088 ) ) ;
#32906 = CARTESIAN_POINT ( 'NONE',  ( 122.1561614775786353, -0.4660016031367893996, -10.09054647747474043 ) ) ;
#32907 = CARTESIAN_POINT ( 'NONE',  ( 120.5110881442453206, -3.505236298600246325, -18.68346056562440793 ) ) ;
#32908 = ORIENTED_EDGE ( 'NONE', *, *, #26446, .T. ) ;
#32909 = CARTESIAN_POINT ( 'NONE',  ( 125.6164881442453094, -9.565557343593413364, -10.61323700422348004 ) ) ;
#32910 = CARTESIAN_POINT ( 'NONE',  ( 118.8660148109119774, -10.30919188438810075, -12.61870101168855918 ) ) ;
#32911 = CARTESIAN_POINT ( 'NONE',  ( 113.0231681442453180, -10.15424416112533912, -14.75197769757731336 ) ) ;
#32912 = CARTESIAN_POINT ( 'NONE',  ( 122.4397948109119767, -9.988377603198976828, -10.36322818467138340 ) ) ;
#32913 = EDGE_CURVE ( 'NONE', #36261, #27061, #27140, .T. ) ;
#32914 = CARTESIAN_POINT ( 'NONE',  ( 105.4819421295248247, 0.8980012041604618078, -13.39321520033831447 ) ) ;
#32915 = DIRECTION ( 'NONE',  ( 0.9609149988134837450, -0.1028163501681639419, 0.2570431154366518145 ) ) ;
#32916 = AXIS2_PLACEMENT_3D ( 'NONE', #26928, #5043, #12353 ) ;
#32917 = CARTESIAN_POINT ( 'NONE',  ( 118.9672361498677162, -2.324775150319212891, -18.02356106541841640 ) ) ;
#32918 = CARTESIAN_POINT ( 'NONE',  ( 112.1494421295248003, -9.868328341294093420, -13.39321520033831447 ) ) ;
#32919 = VECTOR ( 'NONE', #23315, 1000.000000000000114 ) ;
#32920 = CARTESIAN_POINT ( 'NONE',  ( 122.9382985609119743, -0.08252387247370887580, -11.91645802438286417 ) ) ;
#32921 = CARTESIAN_POINT ( 'NONE',  ( 137.4282737236217145, -9.806850323706933992, -12.17485108655606929 ) ) ;
#32922 = CARTESIAN_POINT ( 'NONE',  ( 119.2631014775786298, -9.565557343593413364, -10.61323700422348004 ) ) ;
#32923 = CARTESIAN_POINT ( 'NONE',  ( 123.8012348109119642, 0.2603800115204892296, -16.42320221600525088 ) ) ;
#32924 = DIRECTION ( 'NONE',  ( -1.000000000000000000, 0.000000000000000000, 0.000000000000000000 ) ) ;
#32925 = VERTEX_POINT ( 'NONE', #39841 ) ;
#32926 = CARTESIAN_POINT ( 'NONE',  ( 117.0837890045247747, 0.1360012041604422017, -15.46428301220378998 ) ) ;
#32927 = CARTESIAN_POINT ( 'NONE',  ( 110.6214733795247867, -1.325403438956436419, -9.854619843455211026 ) ) ;
#32928 = CARTESIAN_POINT ( 'NONE',  ( 115.4056881442453459, -2.084020599724406786, -8.691656652584148546 ) ) ;
#32929 = CARTESIAN_POINT ( 'NONE',  ( 86.48169505875749508, -25.99489077589524300, -13.39321520033831625 ) ) ;
#32930 = AXIS2_PLACEMENT_3D ( 'NONE', #42384, #11148, #25052 ) ;
#32931 = DIRECTION ( 'NONE',  ( 1.000000000000000000, 0.000000000000000000, -0.000000000000000000 ) ) ;
#32932 = CARTESIAN_POINT ( 'NONE',  ( 123.7637130757767352, -0.9924539043446216624, -17.29976612834909133 ) ) ;
#32934 = CARTESIAN_POINT ( 'NONE',  ( 122.9503348109119827, 0.5811942927096110934, -14.16772938898807510 ) ) ;
#32933 = CARTESIAN_POINT ( 'NONE',  ( 64.76452260854006227, -13.87123648633732031, -9.027055449389660424 ) ) ;
#32935 = CARTESIAN_POINT ( 'NONE',  ( 123.1772414775786189, -5.574606645277164318, -18.38911715685844683 ) ) ;
#32936 = EDGE_LOOP ( 'NONE', ( #21655, #22063, #41967, #4067 ) ) ;
#32937 = DIRECTION ( 'NONE',  ( -1.000000000000000000, -2.775557561562889810E-17, 0.000000000000000000 ) ) ;
#32938 = CARTESIAN_POINT ( 'NONE',  ( 109.6491296295247793, -4.863998795839590272, -8.388885654883775800 ) ) ;
#32939 = CARTESIAN_POINT ( 'NONE',  ( 124.0281414775786146, -7.643976991954077427, -18.09477374809248928 ) ) ;
#32940 = CARTESIAN_POINT ( 'NONE',  ( 123.4041481442452834, 0.1319031606808879209, -14.10382304977623669 ) ) ;
#32941 = CARTESIAN_POINT ( 'NONE',  ( 116.9940348109119839, -0.1624402480850797581, -16.17319339645315424 ) ) ;
#32942 = DIRECTION ( 'NONE',  ( 0.9609149988134839671, -0.1028163501681660097, 0.2570431154366504822 ) ) ;
#32943 = CARTESIAN_POINT ( 'NONE',  ( 108.3295202545248657, -10.62599879583958717, -15.77991374673208469 ) ) ;
#32944 = CARTESIAN_POINT ( 'NONE',  ( 61.69189222814998175, -69.76310523276724496, -0.9932152003383157846 ) ) ;
#32945 = PLANE ( 'NONE',  #15781 ) ;
#32946 = CARTESIAN_POINT ( 'NONE',  ( 151.2860562277021472, -4.863998795839242995, -13.39321520033831447 ) ) ;
#32947 = CARTESIAN_POINT ( 'NONE',  ( 112.6356140045247827, -10.62599879583958717, -11.00651665394454604 ) ) ;
#32948 = DIRECTION ( 'NONE',  ( 1.000000000000000000, 0.000000000000000000, -0.000000000000000000 ) ) ;
#32949 = CARTESIAN_POINT ( 'NONE',  ( 83.86184402137078564, -31.76396917189504521, -22.70990857689603004 ) ) ;
#32950 = CARTESIAN_POINT ( 'NONE',  ( 120.5110881442453206, -6.344957434206665248, -7.627207830600338134 ) ) ;
#32951 = CARTESIAN_POINT ( 'NONE',  ( 117.5613014775786525, 0.9020085738987339008, -11.91225656197089222 ) ) ;
#32952 = CARTESIAN_POINT ( 'NONE',  ( 106.4542858795248179, -0.7896495226426338832, -17.46756447353520159 ) ) ;
#32953 = CARTESIAN_POINT ( 'NONE',  ( 117.6180281442453150, -0.4660016031367893996, -10.09054647747474043 ) ) ;
#32954 = LINE ( 'NONE', #15429, #27231 ) ;
#32955 = ORIENTED_EDGE ( 'NONE', *, *, #15006, .F. ) ;
#32956 = CARTESIAN_POINT ( 'NONE',  ( 83.44708369096697709, -25.38011337280982715, -14.88121679464376257 ) ) ;
#32957 = VECTOR ( 'NONE', #2979, 1000.000000000000000 ) ;
#32958 = CARTESIAN_POINT ( 'NONE',  ( 122.0427081442452817, 0.5811942927096110934, -14.16772938898807510 ) ) ;
#32959 = VECTOR ( 'NONE', #11272, 1000.000000000000000 ) ;
#32960 = CARTESIAN_POINT ( 'NONE',  ( 120.6812681442452941, -10.30919188438810075, -12.61870101168855918 ) ) ;
#32961 = CARTESIAN_POINT ( 'NONE',  ( 123.8579614775786126, -9.859900752359378018, -12.68260735090039759 ) ) ;
#32962 = DIRECTION ( 'NONE',  ( 1.000000000000000000, 0.000000000000000000, 0.000000000000000000 ) ) ;
#32963 = CARTESIAN_POINT ( 'NONE',  ( 113.8740681442453138, -9.859900752359374465, -12.68260735090039404 ) ) ;
#32964 = CARTESIAN_POINT ( 'NONE',  ( 111.8886348109120092, -6.222761293078241884, -8.102969835052219238 ) ) ;
#32965 = CARTESIAN_POINT ( 'NONE',  ( 107.2877233795247776, -8.938348069036489818, -17.46756447353520159 ) ) ;
#32966 = AXIS2_PLACEMENT_3D ( 'NONE', #11298, #18367, #1251 ) ;
#32967 = EDGE_CURVE ( 'NONE', #5058, #19198, #3843, .T. ) ;
#32968 = CARTESIAN_POINT ( 'NONE',  ( 120.1140014775786398, -7.894159318335828068, -9.358103419637847864 ) ) ;
#32969 = CARTESIAN_POINT ( 'NONE',  ( 115.8999108795247821, -8.938348069036489818, -9.318865927141430916 ) ) ;
#32970 = ORIENTED_EDGE ( 'NONE', *, *, #8952, .F. ) ;
#32971 = CARTESIAN_POINT ( 'NONE',  ( 122.3826735609119680, -9.645473719204776586, -14.86997237629376656 ) ) ;
#32972 = CARTESIAN_POINT ( 'NONE',  ( 122.7801548109119665, -3.383040157471821630, -19.15922257007629170 ) ) ;
#32973 = CARTESIAN_POINT ( 'NONE',  ( 122.4218349628857254, -6.095137211460710525, -18.44441274085890115 ) ) ;
#32974 = CARTESIAN_POINT ( 'NONE',  ( -13.46067391278434400, -4.920719406499494575, -8.640382031922472450 ) ) ;
#32975 = CARTESIAN_POINT ( 'NONE',  ( 46.84966980880212617, -19.07391775237791620, -18.19321520033831519 ) ) ;
#32976 = CARTESIAN_POINT ( 'NONE',  ( 118.4122014775786340, -9.859900752359374465, -12.68260735090039404 ) ) ;
#32977 = CARTESIAN_POINT ( 'NONE',  ( 65.41915898433887833, -0.3267878074046857706, -16.39321520033831447 ) ) ;
#32978 = CARTESIAN_POINT ( 'NONE',  ( 124.1773369107181821, -2.467220198592779301, -17.83387418641524391 ) ) ;
#32979 = CARTESIAN_POINT ( 'NONE',  ( 124.5954081442453116, -6.222761293078241884, -8.102969835052219238 ) ) ;
#32980 = CARTESIAN_POINT ( 'NONE',  ( 111.9645664091100912, -0.9924539043446216624, -17.29976612834909133 ) ) ;
#32981 = VECTOR ( 'NONE', #18951, 1000.000000000000114 ) ;
#32982 = CARTESIAN_POINT ( 'NONE',  ( 125.4463081442452932, -4.153390946401325223, -8.397313243818185668 ) ) ;
#32983 = AXIS2_PLACEMENT_3D ( 'NONE', #42218, #41166, #27023 ) ;
#32984 = DIRECTION ( 'NONE',  ( 1.000000000000000000, 0.000000000000000000, 0.000000000000000000 ) ) ;
#32985 = CARTESIAN_POINT ( 'NONE',  ( 121.1918081442452859, 0.9020085738987339008, -11.91225656197089222 ) ) ;
#32986 = CARTESIAN_POINT ( 'NONE',  ( 119.2063748109119814, -7.894159318335828068, -9.358103419637847864 ) ) ;
#32987 = CARTESIAN_POINT ( 'NONE',  ( 121.7023481442452777, -0.8288870151387760510, -10.36305467784173118 ) ) ;
#32988 = ORIENTED_EDGE ( 'NONE', *, *, #42307, .T. ) ;
#32989 = CARTESIAN_POINT ( 'NONE',  ( 123.8012348109119642, 0.2603800115204892296, -16.42320221600525088 ) ) ;
#32990 = CARTESIAN_POINT ( 'NONE',  ( 117.1642148109119859, -9.261995988541697145, -16.69588392320189030 ) ) ;
#32991 = CARTESIAN_POINT ( 'NONE',  ( 115.4137390045248566, -9.868328341294098749, -11.32035403202665869 ) ) ;
#32992 = DIRECTION ( 'NONE',  ( 0.000000000000000000, 0.6004852223388321697, -0.7996358532186279566 ) ) ;
#32993 = CARTESIAN_POINT ( 'NONE',  ( 123.2906948109119867, -1.833838273342659697, -17.42832698103878286 ) ) ;
#32994 = CARTESIAN_POINT ( 'NONE',  ( 119.9438214775786378, -7.893985811506177619, -18.51759400769804742 ) ) ;
#32995 = CARTESIAN_POINT ( 'NONE',  ( 114.7886608795247696, -8.938348069036489818, -9.318865927141430916 ) ) ;
#32996 = CARTESIAN_POINT ( 'NONE',  ( 108.3989733795248753, -1.325403438956436419, -9.854619843455211026 ) ) ;
#32997 = CYLINDRICAL_SURFACE ( 'NONE', #34990, 1.999999999999998890 ) ;
#32998 = CONICAL_SURFACE ( 'NONE', #40317, 2.999999999999999556, 0.9599310885968830309 ) ;
#32999 = CARTESIAN_POINT ( 'NONE',  ( 114.7249681442453237, -9.565557343593413364, -10.61323700422348004 ) ) ;
#33000 = CARTESIAN_POINT ( 'NONE',  ( 137.5143514225471222, -2.492992885558165561, -17.79955400039792934 ) ) ;
#33001 = CARTESIAN_POINT ( 'NONE',  ( 124.8790414775786246, -0.4660016031367893996, -10.09054647747474043 ) ) ;
#33002 = VERTEX_POINT ( 'NONE', #8603 ) ;
#33003 = CARTESIAN_POINT ( 'NONE',  ( 123.9714148109119805, -8.899110576539710493, -16.42337572283490132 ) ) ;
#33004 = CARTESIAN_POINT ( 'NONE',  ( 122.3826735609119680, 0.6414057260225851653, -11.69287257290600657 ) ) ;
#33005 = CARTESIAN_POINT ( 'NONE',  ( 121.5492360609119800, -6.564341423271550902, -7.887810678476487425 ) ) ;
#33006 = CARTESIAN_POINT ( 'NONE',  ( 107.2294421295247844, -9.051693226400931991, -21.89321520033831447 ) ) ;
#33007 = CARTESIAN_POINT ( 'NONE',  ( 108.9545983795247821, -8.402594152722688392, -16.93181055722141792 ) ) ;
#33008 = ORIENTED_EDGE ( 'NONE', *, *, #30040, .T. ) ;
#33009 = CARTESIAN_POINT ( 'NONE',  ( 115.7460481442453357, 0.9020085738987339008, -11.91225656197089222 ) ) ;
#33010 = CARTESIAN_POINT ( 'NONE',  ( 113.1366214775786432, -1.834011780172310591, -8.268836392978581529 ) ) ;
#33011 = B_SPLINE_CURVE_WITH_KNOTS ( 'NONE', 3,
 ( #4691, #21353, #7896, #11550, #38665, #35924, #4472, #39129, #7433, #24559, #18610, #18159, #29092, #38445, #35237, #11099, #42117, #28654, #28427, #25232, #32055, #1276, #10877, #32502, #15188, #42340, #43003, #822, #35003, #14291, #14964, #3786, #38895, #21803, #39361, #4013, #14743, #7216, #21128, #1049, #42560, #28877, #17936, #18392, #42789 ),
 .UNSPECIFIED., .F., .F.,
 ( 4, 2, 2, 1, 1, 1, 2, 2, 2, 2, 1, 1, 1, 2, 2, 2, 2, 1, 1, 1, 2, 2, 2, 2, 2, 2, 4 ),
 ( 0.000000000000000000, 0.06250000000006793177, 0.09375000000010108581, 0.1093750000001167677, 0.1171875000001246087, 0.1210937500001285361, 0.1230468750001315892, 0.1250000000001346423, 0.1875000000002185752, 0.2187500000002587930, 0.2343750000002789158, 0.2421875000002898515, 0.2460937500002960687, 0.2480468750002971789, 0.2500000000002982614, 0.3750000000003029799, 0.4375000000003045897, 0.4687500000003050338, 0.4843750000003049228, 0.4921875000003033129, 0.4960937500003007039, 0.5000000000002979839, 0.6250000000002219336, 0.6875000000001831868, 0.7187500000001638689, 0.7500000000001444400, 1.000000000000000000 ),
 .UNSPECIFIED. ) ;
#33012 = CARTESIAN_POINT ( 'NONE',  ( 123.7445081442452874, -7.894159318335828068, -9.358103419637847864 ) ) ;
#33013 = CARTESIAN_POINT ( 'NONE',  ( 114.2711548109119803, -0.1624402480850797581, -16.17319339645315424 ) ) ;
#33014 = DIRECTION ( 'NONE',  ( 0.7202110682883375858, 0.2576522076061144029, -0.6441361323747234469 ) ) ;
#33015 = CARTESIAN_POINT ( 'NONE',  ( 123.8579614775786126, 0.5811942927096084288, -14.16772938898809642 ) ) ;
#33016 = CARTESIAN_POINT ( 'NONE',  ( 113.6471614775786492, -5.638512984488999180, -18.83840828888717311 ) ) ;
#33017 = PRESENTATION_LAYER_ASSIGNMENT (  '', '', ( #25756 ) ) ;
#33018 = CARTESIAN_POINT ( 'NONE',  ( 112.8439733795247832, -1.325403438956436419, -9.854619843455211026 ) ) ;
#33019 = CARTESIAN_POINT ( 'NONE',  ( 124.8790414775786246, -0.4660016031367893996, -10.09054647747474043 ) ) ;
#33020 = DIRECTION ( 'NONE',  ( 0.000000000000000000, 0.3818493186865927203, -0.9242245927363029745 ) ) ;
#33021 = VERTEX_POINT ( 'NONE', #22504 ) ;
#33022 = CARTESIAN_POINT ( 'NONE',  ( 114.0442481442453300, -1.834011780172310813, -8.268836392978581529 ) ) ;
#33023 = CARTESIAN_POINT ( 'NONE',  ( 112.2857214775786474, -5.574606645277164318, -18.38911715685844683 ) ) ;
#33024 = DIRECTION ( 'NONE',  ( -1.000000000000000000, 0.000000000000000000, 0.000000000000000000 ) ) ;
#33025 = CARTESIAN_POINT ( 'NONE',  ( 112.8529881442453302, -1.561330072975668060, -17.79121239304076596 ) ) ;
#33026 = AXIS2_PLACEMENT_3D ( 'NONE', #42319, #14723, #17695 ) ;
#33027 = ORIENTED_EDGE ( 'NONE', *, *, #26712, .T. ) ;
#33028 = CARTESIAN_POINT ( 'NONE',  ( 118.1285681442453068, -7.893985811506177619, -18.51759400769804742 ) ) ;
#33029 = CARTESIAN_POINT ( 'NONE',  ( 89.01247232317646763, -25.99489077589524300, -13.39321520033831447 ) ) ;
#33030 = CARTESIAN_POINT ( 'NONE',  ( 65.49983523453742862, -18.16718729050178993, -4.893215200338314474 ) ) ;
#33031 = CARTESIAN_POINT ( 'NONE',  ( 65.19189222814998175, -41.76310523276723785, -24.39321520033831447 ) ) ;
#33032 = CARTESIAN_POINT ( 'NONE',  ( 123.6431847287616534, -4.480430082091682920, -15.15308252923503751 ) ) ;
#33033 = CARTESIAN_POINT ( 'NONE',  ( 114.8384214775786489, -10.15424416112533912, -14.75197769757731336 ) ) ;
#33034 = DIRECTION ( 'NONE',  ( 0.9609149988134837450, -0.1028163501681639419, 0.2570431154366518145 ) ) ;
#33035 = CARTESIAN_POINT ( 'NONE',  ( 121.4069907289968313, -6.032552146994438758, -18.32589373581284420 ) ) ;
#33036 = CARTESIAN_POINT ( 'NONE',  ( 111.7751814775786556, -2.084020599724406786, -8.691656652584148546 ) ) ;
#33037 = CARTESIAN_POINT ( 'NONE',  ( 112.6260814775786514, -9.261995988541697145, -16.69588392320189030 ) ) ;
#33038 = CARTESIAN_POINT ( 'NONE',  ( 116.7263990467714194, -6.377543297015642487, -18.31558037743933909 ) ) ;
#33039 = CARTESIAN_POINT ( 'NONE',  ( 122.8936081442453059, -9.565557343593413364, -10.61323700422348004 ) ) ;
#33040 = CARTESIAN_POINT ( 'NONE',  ( 86.48169505875749508, -25.23119213852205789, -15.24166438581092109 ) ) ;
#33041 = CARTESIAN_POINT ( 'NONE',  ( 124.1415948109119540, -6.344957434206665248, -7.627207830600338134 ) ) ;
#33042 = CIRCLE ( 'NONE', #38881, 2.999999999999999556 ) ;
#33043 = CARTESIAN_POINT ( 'NONE',  ( 121.3052614775786111, -1.834011780172310813, -8.268836392978581529 ) ) ;
#33044 = ORIENTED_EDGE ( 'NONE', *, *, #5695, .F. ) ;
#33045 = CARTESIAN_POINT ( 'NONE',  ( 127.0553483106877621, -8.467588782543378656, -17.43966488234757506 ) ) ;
#33046 = CARTESIAN_POINT ( 'NONE',  ( 113.1912390045248031, 0.8980012041604421569, -15.77991374673208469 ) ) ;
#33047 = CARTESIAN_POINT ( 'NONE',  ( 111.5938171295247940, 0.1403307496149613920, -13.39321520033831447 ) ) ;
#33048 = CARTESIAN_POINT ( 'NONE',  ( 109.4407702545248355, 0.1403307496149616695, -11.32035403202665336 ) ) ;
#33049 = CARTESIAN_POINT ( 'NONE',  ( 127.0066334553000615, -9.957176252831715146, -11.61677030087517792 ) ) ;
#33050 = CARTESIAN_POINT ( 'NONE',  ( 114.4980614775786592, -7.893985811506177619, -18.51759400769804742 ) ) ;
#33051 = ORIENTED_EDGE ( 'NONE', *, *, #8952, .T. ) ;
#33052 = CARTESIAN_POINT ( 'NONE',  ( 123.6776560953690591, -6.001247023715324147, -18.26661038929047010 ) ) ;
#33053 = FACE_OUTER_BOUND ( 'NONE', #31161, .T. ) ;
#33054 = CARTESIAN_POINT ( 'NONE',  ( 115.4056881442453459, -2.084020599724406786, -8.691656652584148546 ) ) ;
#33055 = ADVANCED_FACE ( 'NONE', ( #36398 ), #1748, .T. ) ;
#33056 = CARTESIAN_POINT ( 'NONE',  ( 112.8337832127138682, -2.191907684172563986, -18.20049396185734025 ) ) ;
#33057 = CARTESIAN_POINT ( 'NONE',  ( 120.3976348109119812, -1.834011780172310813, -8.268836392978581529 ) ) ;
#33058 = CARTESIAN_POINT ( 'NONE',  ( 109.4407702545248355, -10.62599879583958717, -15.77991374673208469 ) ) ;
#33059 = CARTESIAN_POINT ( 'NONE',  ( 66.06194382436763135, -14.97931106434683635, -4.893215200338314474 ) ) ;
#33060 = ORIENTED_EDGE ( 'NONE', *, *, #28100, .T. ) ;
#33061 = CARTESIAN_POINT ( 'NONE',  ( 120.7379948109119709, 0.4262465694468476896, -12.03445270309931381 ) ) ;
#33062 = CARTESIAN_POINT ( 'NONE',  ( 117.7314814775786260, -5.574606645277164318, -18.38911715685844683 ) ) ;
#33063 = CARTESIAN_POINT ( 'NONE',  ( 115.3489614775786407, -9.261995988541697145, -16.69588392320189030 ) ) ;
#33064 = EDGE_CURVE ( 'NONE', #11695, #22801, #23539, .T. ) ;
#33065 = CARTESIAN_POINT ( 'NONE',  ( 115.7460481442453357, 0.9020085738987339008, -11.91225656197089222 ) ) ;
#33066 = FACE_OUTER_BOUND ( 'NONE', #26827, .T. ) ;
#33067 =( BOUNDED_CURVE ( )  B_SPLINE_CURVE ( 3, ( #23365, #27468, #40930, #13339 ),
 .UNSPECIFIED., .F., .T. ) 
 B_SPLINE_CURVE_WITH_KNOTS ( ( 4, 4 ),
 ( 0.000000000000000000, 3.141592653589795336 ),
 .UNSPECIFIED. ) 
 CURVE ( )  GEOMETRIC_REPRESENTATION_ITEM ( )  RATIONAL_B_SPLINE_CURVE ( ( 1.000000000000000000, 0.3333333333333335369, 0.3333333333333335369, 1.000000000000000000 ) ) 
 REPRESENTATION_ITEM ( '' )  );
#33068 = CARTESIAN_POINT ( 'NONE',  ( 122.8936081442453059, -9.565557343593413364, -10.61323700422348004 ) ) ;
#33069 = CARTESIAN_POINT ( 'NONE',  ( 117.6747548109119919, -7.643976991954077427, -18.09477374809248928 ) ) ;
#33070 = VERTEX_POINT ( 'NONE', #5617 ) ;
#33071 = CIRCLE ( 'NONE', #12731, 3.000000000000003997 ) ;
#33072 = CARTESIAN_POINT ( 'NONE',  ( 122.3132204359119868, 1.345710702986147034, -13.97328579221134426 ) ) ;
#33073 = CARTESIAN_POINT ( 'NONE',  ( 113.8740681442453138, 0.5811942927096154232, -14.16772938898807155 ) ) ;
#33074 = CARTESIAN_POINT ( 'NONE',  ( 116.1431348109119881, 0.1319031606808879209, -14.10382304977623669 ) ) ;
#33075 = ORIENTED_EDGE ( 'NONE', *, *, #16974, .T. ) ;
#33076 = CARTESIAN_POINT ( 'NONE',  ( 120.7157985609119635, -0.08252387247370887580, -11.91645802438286417 ) ) ;
#33077 = CARTESIAN_POINT ( 'NONE',  ( 114.5547881442453217, -5.638512984488999180, -18.83840828888717311 ) ) ;
#33078 = VECTOR ( 'NONE', #39454, 1000.000000000000227 ) ;
#33079 = CARTESIAN_POINT ( 'NONE',  ( 115.3442858795247759, -0.7896495226426338832, -17.46756447353520159 ) ) ;
#33080 = CARTESIAN_POINT ( 'NONE',  ( 114.4980614775786734, -2.084020599724406786, -8.691656652584148546 ) ) ;
#33081 = ADVANCED_FACE ( 'NONE', ( #33417 ), #15196, .T. ) ;
#33082 = VERTEX_POINT ( 'NONE', #10412 ) ;
#33083 = VERTEX_POINT ( 'NONE', #9968 ) ;
#33084 = CARTESIAN_POINT ( 'NONE',  ( 121.2485348109119769, -8.899110576539710493, -16.42337572283490132 ) ) ;
#33085 = CARTESIAN_POINT ( 'NONE',  ( 121.0783548109119749, -9.565557343593413364, -10.61323700422348004 ) ) ;
#33086 = PRESENTATION_STYLE_ASSIGNMENT (( #29919 ) ) ;
#33087 = EDGE_CURVE ( 'NONE', #26262, #18481, #22055, .T. ) ;
#33088 = ORIENTED_EDGE ( 'NONE', *, *, #495, .F. ) ;
#33089 = CARTESIAN_POINT ( 'NONE',  ( 94.20708369096698220, -25.99489077589524300, -13.39321520033831447 ) ) ;
#33090 = CARTESIAN_POINT ( 'NONE',  ( 61.80337255853385869, -65.85056717495680800, -43.64372168240947758 ) ) ;
#33091 = EDGE_CURVE ( 'NONE', #20113, #34097, #3153, .T. ) ;
#33092 = CARTESIAN_POINT ( 'NONE',  ( 70.19189222814998175, -59.11650476797663600, -36.84940499091918298 ) ) ;
#33093 = CARTESIAN_POINT ( 'NONE',  ( 116.5402214775786405, 0.2603800115204892296, -16.42320221600525088 ) ) ;
#33095 = CARTESIAN_POINT ( 'NONE',  ( 117.5045748109119756, -9.859900752359374465, -12.68260735090039404 ) ) ;
#33094 = CARTESIAN_POINT ( 'NONE',  ( 116.1998614775786507, -10.63000616557722466, -14.87417383870573495 ) ) ;
#33096 = CARTESIAN_POINT ( 'NONE',  ( 121.5321681442453183, -0.1624402480850797581, -16.17319339645315424 ) ) ;
#33097 = LINE ( 'NONE', #14900, #3629 ) ;
#33098 = VERTEX_POINT ( 'NONE', #44853 ) ;
#33099 = CARTESIAN_POINT ( 'NONE',  ( 120.5678148109119832, -1.833838273342659253, -17.42832698103878286 ) ) ;
#33100 = EDGE_CURVE ( 'NONE', #31200, #40221, #17036, .T. ) ;
#33101 = LINE ( 'NONE', #23557, #37301 ) ;
#33102 = CIRCLE ( 'NONE', #17134, 1.610000000000000986 ) ;
#33103 = CARTESIAN_POINT ( 'NONE',  ( 110.7603796295247918, -4.863998795839590272, -19.15521520033831493 ) ) ;
#33104 = CARTESIAN_POINT ( 'NONE',  ( 113.8531398611596046, -1.036737761566196570, -17.24079555149560505 ) ) ;
#33105 = CARTESIAN_POINT ( 'NONE',  ( 109.7880358795247986, -0.7896495226426338832, -17.46756447353520159 ) ) ;
#33106 = CARTESIAN_POINT ( 'NONE',  ( 119.0929214775786278, -5.638512984488999180, -18.83840828888717311 ) ) ;
#33107 = ORIENTED_EDGE ( 'NONE', *, *, #11905, .F. ) ;
#33108 = ADVANCED_FACE ( 'NONE', ( #13391 ), #3336, .F. ) ;
#33109 = CARTESIAN_POINT ( 'NONE',  ( 122.4397948109119767, -9.988377603198976828, -10.36322818467138340 ) ) ;
#33110 = CARTESIAN_POINT ( 'NONE',  ( 63.14350240710648876, -37.75742606650420896, -4.969760221102785813 ) ) ;
#33111 = CARTESIAN_POINT ( 'NONE',  ( 108.6073327545248048, -2.477300249445798297, -19.15521520033831138 ) ) ;
#33112 = CARTESIAN_POINT ( 'NONE',  ( 119.7169148109119874, -9.988377603198976828, -10.36322818467138340 ) ) ;
#33113 = ADVANCED_FACE ( 'NONE', ( #20453 ), #9692, .T. ) ;
#33114 = EDGE_CURVE ( 'NONE', #28792, #40778, #24320, .T. ) ;
#33115 = CARTESIAN_POINT ( 'NONE',  ( 118.2987481442453088, -1.561330072975668504, -17.79121239304076951 ) ) ;
#33117 = CIRCLE ( 'NONE', #9852, 4.999999999999998224 ) ;
#33116 = DIRECTION ( 'NONE',  ( 0.000000000000000000, 0.000000000000000000, -1.000000000000000000 ) ) ;
#33118 = CARTESIAN_POINT ( 'NONE',  ( 116.7327219861001879, -11.78583009060342413, -6.254644069865828548 ) ) ;
#33119 = ORIENTED_EDGE ( 'NONE', *, *, #16104, .F. ) ;
#33120 = CARTESIAN_POINT ( 'NONE',  ( 109.2294424962575050, -10.05627679606856795, -15.17422528748209665 ) ) ;
#33121 = CARTESIAN_POINT ( 'NONE',  ( 121.2485348109119769, -8.899110576539710493, -16.42337572283490132 ) ) ;
#33122 = CARTESIAN_POINT ( 'NONE',  ( 113.4690515045247992, -6.936859964151250502, -18.39754474579286025 ) ) ;
#33123 = CARTESIAN_POINT ( 'NONE',  ( 109.5102233795247884, -1.325403438956436419, -9.854619843455211026 ) ) ;
#33124 = CARTESIAN_POINT ( 'NONE',  ( 117.0507614775786465, 0.1319031606808879209, -14.10382304977623669 ) ) ;
#33125 = FACE_OUTER_BOUND ( 'NONE', #34638, .T. ) ;
#33126 = CARTESIAN_POINT ( 'NONE',  ( 69.77898898320889032, -25.66191150022318723, -5.787138065658675501 ) ) ;
#33127 = CARTESIAN_POINT ( 'NONE',  ( 112.0020881442453344, -9.565557343593413364, -10.61323700422348004 ) ) ;
#33128 = CARTESIAN_POINT ( 'NONE',  ( 124.0848681442452772, -4.089484607189486809, -7.948022111789456723 ) ) ;
#33129 = ORIENTED_EDGE ( 'NONE', *, *, #29317, .T. ) ;
#33130 = CARTESIAN_POINT ( 'NONE',  ( 117.2776681442452968, -4.153390946401325223, -8.397313243818185668 ) ) ;
#33131 = CARTESIAN_POINT ( 'NONE',  ( 113.8740681442453138, 0.5811942927096154232, -14.16772938898807155 ) ) ;
#33132 = CARTESIAN_POINT ( 'NONE',  ( 122.2696148109119889, -4.089484607189486809, -7.948022111789456723 ) ) ;
#33133 = CARTESIAN_POINT ( 'NONE',  ( 122.0427081442452817, -9.859900752359378018, -12.68260735090039759 ) ) ;
#33134 = ORIENTED_EDGE ( 'NONE', *, *, #27538, .F. ) ;
#33135 = CARTESIAN_POINT ( 'NONE',  ( 124.6521348109119884, -7.894159318335828068, -9.358103419637847864 ) ) ;
#33136 = AXIS2_PLACEMENT_3D ( 'NONE', #31041, #44971, #13728 ) ;
#33137 = CARTESIAN_POINT ( 'NONE',  ( 123.8012348109119642, 0.2603800115204892296, -16.42320221600525088 ) ) ;
#33138 = DIRECTION ( 'NONE',  ( 0.7871354856660167654, -0.6167752151498625546, -0.002461946824136807422 ) ) ;
#33139 = CARTESIAN_POINT ( 'NONE',  ( 125.7299414775786346, 0.9020085738987339008, -11.91225656197089222 ) ) ;
#33140 = CARTESIAN_POINT ( 'NONE',  ( 117.4502108535611313, -2.239543233855014748, -18.13706010537466895 ) ) ;
#33141 = CIRCLE ( 'NONE', #12051, 2.000000000000000444 ) ;
#33142 = FACE_OUTER_BOUND ( 'NONE', #10903, .T. ) ;
#33143 = CARTESIAN_POINT ( 'NONE',  ( 137.9312451099349914, -1.677599621188868406, -16.38739216894681050 ) ) ;
#33144 = CARTESIAN_POINT ( 'NONE',  ( 110.4131140045248287, 0.1403307496149616695, -15.46607636864997204 ) ) ;
#33145 = CARTESIAN_POINT ( 'NONE',  ( 70.19189222814998175, -59.11650476797663600, -36.84940499091918298 ) ) ;
#33146 = CARTESIAN_POINT ( 'NONE',  ( 123.2184548109119788, -4.863998795839242995, -13.39321520033831447 ) ) ;
#33147 = CARTESIAN_POINT ( 'NONE',  ( 120.1707281442453166, -9.565557343593413364, -10.61323700422348004 ) ) ;
#33148 = CARTESIAN_POINT ( 'NONE',  ( 125.5030348109119558, -3.383040157471821630, -19.15922257007629170 ) ) ;
#33149 = CARTESIAN_POINT ( 'NONE',  ( 87.44708369096657918, -25.99489077589583630, -8.393215200338314474 ) ) ;
#33150 = ORIENTED_EDGE ( 'NONE', *, *, #9845, .T. ) ;
#33151 = CARTESIAN_POINT ( 'NONE',  ( 116.2503515045248719, -2.792930983974093007, -8.393215200338321580 ) ) ;
#33152 = CARTESIAN_POINT ( 'NONE',  ( 108.4684265045247997, -2.791137627527939813, -8.388885654883777576 ) ) ;
#33153 = CARTESIAN_POINT ( 'NONE',  ( 115.5191414775786569, -6.222761293078241884, -8.102969835052219238 ) ) ;
#33154 = CARTESIAN_POINT ( 'NONE',  ( 113.5947781477680110, -2.280480477428486363, -18.08254604495228435 ) ) ;
#33155 = ADVANCED_FACE ( 'NONE', ( #37990 ), #6535, .T. ) ;
#33156 = CARTESIAN_POINT ( 'NONE',  ( 70.19189222814998175, -60.04498257489500190, -37.22079287717834717 ) ) ;
#33158 = CARTESIAN_POINT ( 'NONE',  ( 121.1918081442452859, 0.9020085738987339008, -11.91225656197089222 ) ) ;
#33157 = CARTESIAN_POINT ( 'NONE',  ( 86.75477599865929790, -25.38011337280982715, -14.88121679464376257 ) ) ;
#33159 = CIRCLE ( 'NONE', #6243, 4.000000000000000000 ) ;
#33160 = CARTESIAN_POINT ( 'NONE',  ( 124.1983214775786166, -1.833838273342659697, -17.42832698103878286 ) ) ;
#33161 = ORIENTED_EDGE ( 'NONE', *, *, #767, .F. ) ;
#33162 = CARTESIAN_POINT ( 'NONE',  ( 96.21525317080913453, -24.76111397052472540, -15.03073773834309179 ) ) ;
#33163 = CARTESIAN_POINT ( 'NONE',  ( 126.2275303246284608, 0.07306257752206567202, -14.21277131990163767 ) ) ;
#33164 = CARTESIAN_POINT ( 'NONE',  ( 110.9687390045248350, -9.868328341294098749, -11.32035403202665869 ) ) ;
#33165 = EDGE_CURVE ( 'NONE', #22218, #17767, #27516, .T. ) ;
#33166 = CARTESIAN_POINT ( 'NONE',  ( 120.4543614775786295, -5.574606645277164318, -18.38911715685844683 ) ) ;
#33167 = CARTESIAN_POINT ( 'NONE',  ( 120.7379948109119709, 0.4262465694468514643, -12.03445270309931736 ) ) ;
#33168 = CARTESIAN_POINT ( 'NONE',  ( 125.0302870206147503, 2.248781333534738636, -15.92343447212006957 ) ) ;
#33169 = CARTESIAN_POINT ( 'NONE',  ( 107.0099108795247815, -8.938348069036489818, -9.318865927141430916 ) ) ;
#33170 = CARTESIAN_POINT ( 'NONE',  ( 41.72636039845269096, -11.37347657059392070, -17.89321520033831447 ) ) ;
#33171 = EDGE_CURVE ( 'NONE', #29815, #12393, #34113, .T. ) ;
#33172 = CARTESIAN_POINT ( 'NONE',  ( 111.9410827545248708, -2.477300249445798297, -19.15521520033831138 ) ) ;
#33173 = CARTESIAN_POINT ( 'NONE',  ( -13.90346626007465147, -4.337920376228211694, -18.05487786542591166 ) ) ;
#33174 = CARTESIAN_POINT ( 'NONE',  ( 117.2294421295248270, 0.5103437856549055684, -21.89321520033831803 ) ) ;
#33175 = CARTESIAN_POINT ( 'NONE',  ( 119.7169148109119874, -9.988377603198976828, -10.36322818467138340 ) ) ;
#33176 = CARTESIAN_POINT ( 'NONE',  ( 123.8012348109119642, 0.2603800115204892296, -16.42320221600525088 ) ) ;
#33177 = CARTESIAN_POINT ( 'NONE',  ( 108.3295202545248657, -10.62599879583958717, -15.77991374673208469 ) ) ;
#33178 = EDGE_CURVE ( 'NONE', #34283, #6949, #38424, .T. ) ;
#33179 = CARTESIAN_POINT ( 'NONE',  ( 115.0653281442453277, -6.344957434206662583, -7.627207830600332805 ) ) ;
#33180 = CARTESIAN_POINT ( 'NONE',  ( 61.69189222814998175, -49.76310523276723785, -13.39321520033831447 ) ) ;
#33181 = ORIENTED_EDGE ( 'NONE', *, *, #39514, .F. ) ;
#33182 = DIRECTION ( 'NONE',  ( 0.000000000000000000, 0.000000000000000000, -1.000000000000000000 ) ) ;
#33183 = CIRCLE ( 'NONE', #15725, 2.999999999999999556 ) ;
#33184 = CARTESIAN_POINT ( 'NONE',  ( 124.4819548109119722, -7.893985811506177619, -18.51759400769804742 ) ) ;
#33185 = CARTESIAN_POINT ( 'NONE',  ( 118.9227414775786400, -10.63000616557722466, -14.87417383870573495 ) ) ;
#33186 = CONICAL_SURFACE ( 'NONE', #10658, 1.610000000000000986, 0.9599310885968765916 ) ;
#33187 = CARTESIAN_POINT ( 'NONE',  ( 126.6942948109119840, -8.899110576539710493, -16.42337572283490132 ) ) ;
#33188 = CONTEXT_DEPENDENT_SHAPE_REPRESENTATION ( #4380, #38674 ) ;
#33189 = DIRECTION ( 'NONE',  ( -1.224775218828351862E-16, 0.9242245927363029745, 0.3818493186865928868 ) ) ;
#33190 = CARTESIAN_POINT ( 'NONE',  ( 112.2857214775786474, -5.574606645277164318, -18.38911715685844683 ) ) ;
#33191 = CARTESIAN_POINT ( 'NONE',  ( 125.6732148109119862, 0.5811942927096110934, -14.16772938898807510 ) ) ;
#33192 = CARTESIAN_POINT ( 'NONE',  ( 110.4131140045248287, -10.62599879583958717, -11.00651665394454604 ) ) ;
#33193 = CARTESIAN_POINT ( 'NONE',  ( 118.8660148109119774, 0.1319031606808879209, -14.10382304977623669 ) ) ;
#33194 = CARTESIAN_POINT ( 'NONE',  ( 116.7654395844541284, -4.393248286083126786, -18.55097782704973497 ) ) ;
#33195 = VECTOR ( 'NONE', #38134, 1000.000000000000000 ) ;
#33196 = DIRECTION ( 'NONE',  ( -0.8636456077245080465, 0.5040994586965603652, 0.000000000000000000 ) ) ;
#33197 = ORIENTED_EDGE ( 'NONE', *, *, #1035, .T. ) ;
#33198 = APPLICATION_CONTEXT ( 'automotive_design' ) ;
#33199 = CARTESIAN_POINT ( 'NONE',  ( 122.3132204359119868, -10.25716656981731489, -12.88942061488890545 ) ) ;
#33200 = CARTESIAN_POINT ( 'NONE',  ( 121.3052614775786111, -1.834011780172310813, -8.268836392978581529 ) ) ;
#33201 = CIRCLE ( 'NONE', #13579, 2.541999999999999371 ) ;
#33202 = DIRECTION ( 'NONE',  ( 1.000000000000000000, 0.000000000000000000, -0.000000000000000000 ) ) ;
#33203 = CARTESIAN_POINT ( 'NONE',  ( 124.9009360172564556, 2.024339171940786386, -10.02384774242203136 ) ) ;
#33204 = CARTESIAN_POINT ( 'NONE',  ( 115.1139883310706722, 0.1843591316377651834, -12.14321520033831625 ) ) ;
#33205 = CARTESIAN_POINT ( 'NONE',  ( 117.7882081442453170, -3.505236298600246325, -18.68346056562440793 ) ) ;
#33206 = CARTESIAN_POINT ( 'NONE',  ( 68.13072346129467860, -0.9465212610118308723, -16.39321520033831447 ) ) ;
#33207 = DIRECTION ( 'NONE',  ( 0.000000000000000000, -0.3818493186865927203, 0.9242245927363029745 ) ) ;
#33208 = CARTESIAN_POINT ( 'NONE',  ( 124.4819548109119722, -2.084020599724406786, -8.691656652584148546 ) ) ;
#33209 = EDGE_CURVE ( 'NONE', #35524, #24941, #34769, .T. ) ;
#33210 = CARTESIAN_POINT ( 'NONE',  ( 109.7922320646196823, 0.6269505268395592079, -14.64321520033831447 ) ) ;
#33211 = AXIS2_PLACEMENT_3D ( 'NONE', #15559, #36295, #4842 ) ;
#33212 = DIRECTION ( 'NONE',  ( -1.000000000000000000, 0.000000000000000000, -0.000000000000000000 ) ) ;
#33213 = CYLINDRICAL_SURFACE ( 'NONE', #24509, 5.000000000000000888 ) ;
#33214 = CARTESIAN_POINT ( 'NONE',  ( 124.3685014775786328, -10.63000616557722466, -14.87417383870573495 ) ) ;
#33215 = CARTESIAN_POINT ( 'NONE',  ( 116.4834948109119779, -7.894159318335828068, -9.358103419637847864 ) ) ;
#33216 = CARTESIAN_POINT ( 'NONE',  ( 123.6877814775786533, -6.222761293078241884, -8.102969835052219238 ) ) ;
#33217 = ORIENTED_EDGE ( 'NONE', *, *, #32152, .F. ) ;
#33218 = CARTESIAN_POINT ( 'NONE',  ( 122.1561614775786353, -0.4660016031367893996, -10.09054647747474043 ) ) ;
#33219 = CARTESIAN_POINT ( 'NONE',  ( 114.8384214775786489, 0.9020085738987339008, -11.91225656197089222 ) ) ;
#33220 = CARTESIAN_POINT ( 'NONE',  ( 116.9417077545247992, -2.791137627527939813, -18.39754474579286025 ) ) ;
#33221 = CYLINDRICAL_SURFACE ( 'NONE', #27768, 1.999999999999998890 ) ;
#33222 = CARTESIAN_POINT ( 'NONE',  ( 123.6877814775786533, -6.222761293078241884, -8.102969835052219238 ) ) ;
#33223 = CARTESIAN_POINT ( 'NONE',  ( 124.7088614775786226, 0.2603800115204892296, -16.42320221600525088 ) ) ;
#33224 = CARTESIAN_POINT ( 'NONE',  ( 113.3995983795247895, -0.7896495226426338832, -9.318865927141430916 ) ) ;
#33225 = CARTESIAN_POINT ( 'NONE',  ( 108.4684265045248424, -2.791137627527939813, -8.388885654883777576 ) ) ;
#33226 = CARTESIAN_POINT ( 'NONE',  ( 83.44708369096697709, -25.99489077589524300, -13.39321520033831625 ) ) ;
#33227 = CARTESIAN_POINT ( 'NONE',  ( 113.8740681442453138, -9.859900752359374465, -12.68260735090039404 ) ) ;
#33228 = EDGE_CURVE ( 'NONE', #24205, #17200, #26340, .T. ) ;
#33229 = DIRECTION ( 'NONE',  ( 1.000000000000000000, 0.000000000000000000, -0.000000000000000000 ) ) ;
#33230 = VECTOR ( 'NONE', #25798, 1000.000000000000000 ) ;
#33231 = CARTESIAN_POINT ( 'NONE',  ( 113.7468640045248236, 0.1403307496149616695, -15.46607636864997204 ) ) ;
#33232 = VERTEX_POINT ( 'NONE', #3989 ) ;
#33233 = CARTESIAN_POINT ( 'NONE',  ( 126.1837548109119496, 0.4262465694468514643, -12.03445270309931736 ) ) ;
#33234 = CARTESIAN_POINT ( 'NONE',  ( 123.0077516859119839, -9.665098340737509730, -17.37397104707595474 ) ) ;
#33235 = CARTESIAN_POINT ( 'NONE',  ( 121.8270485609119760, -10.36940331770106916, -15.09355782777062061 ) ) ;
#33236 = VERTEX_POINT ( 'NONE', #32476 ) ;
#33237 = DIRECTION ( 'NONE',  ( -1.000000000000000000, 0.000000000000000000, 0.000000000000000000 ) ) ;
#33238 = CARTESIAN_POINT ( 'NONE',  ( 109.7185827545247889, -6.936859964151250502, -8.388885654883777576 ) ) ;
#33239 = AXIS2_PLACEMENT_3D ( 'NONE', #9478, #41629, #17010 ) ;
#33240 = ORIENTED_EDGE ( 'NONE', *, *, #25993, .F. ) ;
#33241 = CARTESIAN_POINT ( 'NONE',  ( 118.8660148109119774, -10.30919188438810075, -12.61870101168855918 ) ) ;
#33242 = CARTESIAN_POINT ( 'NONE',  ( 124.4252281442452812, -0.8288870151387760510, -10.36305467784173118 ) ) ;
#33243 = CARTESIAN_POINT ( 'NONE',  ( 116.3700414775786527, -4.153390946401321671, -8.397313243818183892 ) ) ;
#33244 = DIRECTION ( 'NONE',  ( 0.8636456077245086016, -0.5040994586965593660, 0.000000000000000000 ) ) ;
#33245 = CARTESIAN_POINT ( 'NONE',  ( 124.2550481442452792, -9.988377603198980381, -10.36322818467138518 ) ) ;
#33246 = CARTESIAN_POINT ( 'NONE',  ( 115.2355081442453155, -10.30919188438810075, -12.61870101168855918 ) ) ;
#33247 = AXIS2_PLACEMENT_3D ( 'NONE', #4047, #14103, #858 ) ;
#33248 = CARTESIAN_POINT ( 'NONE',  ( 112.6356140045247827, 0.1403307496149616695, -15.46607636864997204 ) ) ;
#33249 = EDGE_CURVE ( 'NONE', #31523, #37055, #7641, .T. ) ;
#33250 = CARTESIAN_POINT ( 'NONE',  ( 123.9714148109119805, -0.4660016031367893996, -10.09054647747474043 ) ) ;
#33251 =( NAMED_UNIT ( * ) PLANE_ANGLE_UNIT ( ) SI_UNIT ( $, .RADIAN. ) );
#33252 = VERTEX_POINT ( 'NONE', #24976 ) ;
#33253 = CARTESIAN_POINT ( 'NONE',  ( 115.1787814775786387, -9.988377603198976828, -10.36322818467138340 ) ) ;
#33254 = CARTESIAN_POINT ( 'NONE',  ( 113.1933481442453058, -5.574606645277164318, -18.38911715685844683 ) ) ;
#33255 = FACE_OUTER_BOUND ( 'NONE', #20437, .T. ) ;
#33256 = CARTESIAN_POINT ( 'NONE',  ( 126.2972081442452890, -2.084020599724406786, -8.691656652584148546 ) ) ;
#33257 = ORIENTED_EDGE ( 'NONE', *, *, #35618, .F. ) ;
#33258 = CARTESIAN_POINT ( 'NONE',  ( 122.7234281442452755, -5.638512984488999180, -18.83840828888717311 ) ) ;
#33260 = DIRECTION ( 'NONE',  ( -1.000000000000000000, 0.000000000000000000, 0.000000000000000000 ) ) ;
#33259 = AXIS2_PLACEMENT_3D ( 'NONE', #8485, #42922, #11686 ) ;
#33261 = DIRECTION ( 'NONE',  ( 1.000000000000000000, 0.000000000000000000, -0.000000000000000000 ) ) ;
#33262 = DIRECTION ( 'NONE',  ( 1.000000000000000000, 0.000000000000000000, 0.000000000000000000 ) ) ;
#33263 = CARTESIAN_POINT ( 'NONE',  ( 113.5337081442453240, -0.8288870151387760510, -10.36305467784173118 ) ) ;
#33264 = DIRECTION ( 'NONE',  ( 0.000000000000000000, -0.3818493186865927203, 0.9242245927363029745 ) ) ;
#33265 = CARTESIAN_POINT ( 'NONE',  ( 125.3328280236779904, -3.140424913533931939, -20.28213322351574277 ) ) ;
#33266 = CARTESIAN_POINT ( 'NONE',  ( 125.7299414775786346, 0.9020085738987339008, -11.91225656197089222 ) ) ;
#33267 = CARTESIAN_POINT ( 'NONE',  ( 112.0020881442453344, 0.2603800115204892296, -16.42320221600525088 ) ) ;
#33268 = CARTESIAN_POINT ( 'NONE',  ( 124.5357204359119550, -10.25716656981731489, -12.88942061488890545 ) ) ;
#33269 = CARTESIAN_POINT ( 'NONE',  ( 113.0798948109119948, -0.4660016031367893996, -10.09054647747474043 ) ) ;
#33270 = CARTESIAN_POINT ( 'NONE',  ( 116.9940348109119839, -0.1624402480850797581, -16.17319339645315424 ) ) ;
#33271 = CARTESIAN_POINT ( 'NONE',  ( 124.3685014775786328, -10.63000616557722466, -14.87417383870573495 ) ) ;
#33272 = VECTOR ( 'NONE', #20236, 1000.000000000000227 ) ;
#33273 = CARTESIAN_POINT ( 'NONE',  ( 121.1918081442452859, 0.9020085738987339008, -11.91225656197089222 ) ) ;
#33274 = ORIENTED_EDGE ( 'NONE', *, *, #33228, .F. ) ;
#33275 = CARTESIAN_POINT ( 'NONE',  ( 117.6302601386228730, -1.125321370491268125, -17.12283323191015327 ) ) ;
#33276 = CARTESIAN_POINT ( 'NONE',  ( 113.3995983795247895, -0.7896495226426338832, -9.318865927141430916 ) ) ;
#33277 = CARTESIAN_POINT ( 'NONE',  ( 110.7603796295247918, -4.863998795839590272, -8.388885654883775800 ) ) ;
#33278 = CARTESIAN_POINT ( 'NONE',  ( 107.9128015045248219, -6.936859964151250502, -18.39754474579286025 ) ) ;
#33279 = CARTESIAN_POINT ( 'NONE',  ( 126.6390922358717717, -9.857170889351081655, -11.90331356446383282 ) ) ;
#33280 = CARTESIAN_POINT ( 'NONE',  ( 119.8303681442453126, -10.63000616557722466, -14.87417383870573495 ) ) ;
#33281 = ORIENTED_EDGE ( 'NONE', *, *, #5077, .T. ) ;
#33282 = CARTESIAN_POINT ( 'NONE',  ( 124.9357681442453014, -1.834011780172310813, -8.268836392978581529 ) ) ;
#33283 = LINE ( 'NONE', #36929, #32811 ) ;
#33284 = DIRECTION ( 'NONE',  ( 1.000000000000000000, 0.000000000000000000, 0.000000000000000000 ) ) ;
#33285 = CARTESIAN_POINT ( 'NONE',  ( 113.7606148109119886, -7.894159318335828068, -9.358103419637847864 ) ) ;
#33286 = CARTESIAN_POINT ( 'NONE',  ( 118.9227414775786400, -10.63000616557722466, -14.87417383870573495 ) ) ;
#33287 = CARTESIAN_POINT ( 'NONE',  ( 110.2742077545248094, -7.250697342233347165, -7.631215200338321125 ) ) ;
#33288 = DIRECTION ( 'NONE',  ( 0.000000000000000000, 0.000000000000000000, 1.000000000000000000 ) ) ;
#33289 = ORIENTED_EDGE ( 'NONE', *, *, #22336, .F. ) ;
#33290 = CARTESIAN_POINT ( 'NONE',  ( 121.0216281442452981, -7.894159318335803199, -9.358103419637831877 ) ) ;
#33291 = CARTESIAN_POINT ( 'NONE',  ( 122.1561614775786353, -8.899110576539710493, -16.42337572283490132 ) ) ;
#33292 = CARTESIAN_POINT ( 'NONE',  ( 120.3976348109119812, -1.834011780172310813, -8.268836392978581529 ) ) ;
#33293 = CARTESIAN_POINT ( 'NONE',  ( 114.9518748109119883, -7.643976991954077427, -18.09477374809248928 ) ) ;
#33294 = CARTESIAN_POINT ( 'NONE',  ( 116.1431348109119881, -10.30919188438810075, -12.61870101168855918 ) ) ;
#33295 = DIRECTION ( 'NONE',  ( -1.000000000000000000, 0.000000000000000000, 0.000000000000000000 ) ) ;
#33296 = CARTESIAN_POINT ( 'NONE',  ( 123.2339681442453241, -3.505236298600246325, -18.68346056562440793 ) ) ;
#33297 = CARTESIAN_POINT ( 'NONE',  ( 121.1350814775786233, -9.859900752359378018, -12.68260735090039759 ) ) ;
#33298 = EDGE_LOOP ( 'NONE', ( #31108, #43586, #10467, #10790 ) ) ;
#33299 = CARTESIAN_POINT ( 'NONE',  ( 119.2255797424434149, -0.9924539043446216624, -17.29976612834909133 ) ) ;
#33300 = CARTESIAN_POINT ( 'NONE',  ( 112.5126281442453120, -10.30919188438810075, -12.61870101168855918 ) ) ;
#33301 = CARTESIAN_POINT ( 'NONE',  ( 120.2274548109119934, -9.859900752359378018, -12.68260735090039759 ) ) ;
#33302 = EDGE_LOOP ( 'NONE', ( #9266, #25767, #10542, #40022 ) ) ;
#33303 = CARTESIAN_POINT ( 'NONE',  ( 122.7993923109119692, -0.4387604401700512802, -15.73000352943951619 ) ) ;
#33304 = CARTESIAN_POINT ( 'NONE',  ( 120.1140014775786398, -1.561330072975668504, -17.79121239304076951 ) ) ;
#33305 = AXIS2_PLACEMENT_3D ( 'NONE', #22685, #36583, #5359 ) ;
#33306 = CARTESIAN_POINT ( 'NONE',  ( 112.7745202545247878, -10.62599879583958717, -15.77991374673208469 ) ) ;
#33307 = CARTESIAN_POINT ( 'NONE',  ( 116.4267681442453153, -6.222761293078241884, -8.102969835052219238 ) ) ;
#33308 = ORIENTED_EDGE ( 'NONE', *, *, #3698, .T. ) ;
#33309 = ORIENTED_EDGE ( 'NONE', *, *, #22838, .F. ) ;
#33310 = CARTESIAN_POINT ( 'NONE',  ( 125.7866681442452688, -8.899110576539710493, -16.42337572283490132 ) ) ;
#33311 = CARTESIAN_POINT ( 'NONE',  ( 122.2128881442453263, -7.643976991954077427, -18.09477374809248928 ) ) ;
#33312 =( NAMED_UNIT ( * ) SI_UNIT ( $, .STERADIAN. ) SOLID_ANGLE_UNIT ( ) );
#33313 = DIRECTION ( 'NONE',  ( 0.000000000000000000, 1.000000000000000000, 1.069961080215129965E-32 ) ) ;
#33314 = CARTESIAN_POINT ( 'NONE',  ( 117.1642148109119859, -9.261995988541697145, -16.69588392320189030 ) ) ;
#33315 = CARTESIAN_POINT ( 'NONE',  ( 105.6208483795248299, -0.7896495226426338832, -9.318865927141430916 ) ) ;
#33316 = VECTOR ( 'NONE', #3568, 1000.000000000000000 ) ;
#33317 = CARTESIAN_POINT ( 'NONE',  ( 114.5547881442453217, -5.638512984488999180, -18.83840828888717311 ) ) ;
#33319 = CARTESIAN_POINT ( 'NONE',  ( 117.8449348109119938, -1.833838273342659253, -17.42832698103878286 ) ) ;
#33318 = CARTESIAN_POINT ( 'NONE',  ( 114.3278814775786429, -10.30919188438810075, -12.61870101168855918 ) ) ;
#33320 = CARTESIAN_POINT ( 'NONE',  ( 124.7655881442452852, -9.859900752359378018, -12.68260735090039759 ) ) ;
#33321 = CARTESIAN_POINT ( 'NONE',  ( 143.3676850761856940, -59.27884951796255564, -42.87418841894956500 ) ) ;
#33322 = ORIENTED_EDGE ( 'NONE', *, *, #30301, .T. ) ;
#33323 = CARTESIAN_POINT ( 'NONE',  ( 124.5954081442453116, -6.222761293078241884, -8.102969835052219238 ) ) ;
#33324 = CARTESIAN_POINT ( 'NONE',  ( 114.0486636525450450, -2.378957183258581853, -17.95140958770220152 ) ) ;
#33325 = CARTESIAN_POINT ( 'NONE',  ( 112.0105358795247810, -0.7896495226426338832, -17.46756447353520159 ) ) ;
#33326 = CARTESIAN_POINT ( 'NONE',  ( 114.7192077545248594, -2.791137627527939813, -18.39754474579286025 ) ) ;
#33327 = CARTESIAN_POINT ( 'NONE',  ( 113.1217858795247935, -0.7896495226426338832, -17.46756447353520159 ) ) ;
#33328 = CARTESIAN_POINT ( 'NONE',  ( 119.2631014775786298, 0.2603800115204892296, -16.42320221600525088 ) ) ;
#33329 = ORIENTED_EDGE ( 'NONE', *, *, #43752, .T. ) ;
#33330 = CARTESIAN_POINT ( 'NONE',  ( 120.9081748109119872, -5.638512984488999180, -18.83840828888717311 ) ) ;
#33331 = CARTESIAN_POINT ( 'NONE',  ( 70.19189222814998175, -58.90901798090458641, -36.76641099935233825 ) ) ;
#33332 = CARTESIAN_POINT ( 'NONE',  ( 107.0099108795247815, -8.938348069036489818, -9.318865927141430916 ) ) ;
#33333 = CARTESIAN_POINT ( 'NONE',  ( 119.6601881442453106, -8.166667518702819706, -8.995218007635861213 ) ) ;
#33334 = CARTESIAN_POINT ( 'NONE',  ( 120.9081748109119872, -5.638512984488999180, -18.83840828888717311 ) ) ;
#33335 = CARTESIAN_POINT ( 'NONE',  ( 63.88436160695720645, -2.978941093719386757, -18.88846529135332020 ) ) ;
#33336 = CARTESIAN_POINT ( 'NONE',  ( 120.6550937114597275, -6.208002839291213881, -18.65814938918611077 ) ) ;
#33337 = EDGE_CURVE ( 'NONE', #38926, #1783, #41723, .T. ) ;
#33338 = ORIENTED_EDGE ( 'NONE', *, *, #27263, .T. ) ;
#33339 = CARTESIAN_POINT ( 'NONE',  ( -2.667303743122483528, -7.084803291745695120, -7.454506892862497125 ) ) ;
#33340 = CARTESIAN_POINT ( 'NONE',  ( 109.2292810560890786, -10.43422423177587000, -12.93205439691941017 ) ) ;
#33341 = CARTESIAN_POINT ( 'NONE',  ( 123.4041481442452834, 0.1319031606808879209, -14.10382304977623669 ) ) ;
#33342 = CARTESIAN_POINT ( 'NONE',  ( 112.4967077545247633, -2.791137627527939813, -18.39754474579286025 ) ) ;
#33343 = CARTESIAN_POINT ( 'NONE',  ( 111.8716296295247901, -4.863998795839590272, -8.388885654883775800 ) ) ;
#33344 = CARTESIAN_POINT ( 'NONE',  ( 116.8238548109119819, -5.574606645277164318, -18.38911715685844683 ) ) ;
#33345 = FACE_OUTER_BOUND ( 'NONE', #23647, .T. ) ;
#33346 = CARTESIAN_POINT ( 'NONE',  ( 69.68376945742858197, -25.46719311063753466, -5.786137840895125173 ) ) ;
#33347 = CARTESIAN_POINT ( 'NONE',  ( 125.8433948109119456, -1.834011780172310813, -8.268836392978581529 ) ) ;
#33348 = CARTESIAN_POINT ( 'NONE',  ( 124.6521348109119884, -1.561330072975668948, -17.79121239304076951 ) ) ;
#33349 = ORIENTED_EDGE ( 'NONE', *, *, #6638, .F. ) ;
#33350 = EDGE_CURVE ( 'NONE', #43627, #22284, #28632, .T. ) ;
#33351 = CARTESIAN_POINT ( 'NONE',  ( 120.9649014775786355, -6.222761293078241884, -8.102969835052219238 ) ) ;
#33352 = CARTESIAN_POINT ( 'NONE',  ( 116.5402214775786405, 0.2603800115204892296, -16.42320221600525088 ) ) ;
#33353 = CARTESIAN_POINT ( 'NONE',  ( 122.3830681442452857, -8.166667518702819706, -8.995218007635861213 ) ) ;
#33354 = CIRCLE ( 'NONE', #19543, 0.1999999999999988731 ) ;
#33355 = CARTESIAN_POINT ( 'NONE',  ( 124.3685014775786328, 0.4262465694468514643, -12.03445270309931736 ) ) ;
#33356 = ORIENTED_EDGE ( 'NONE', *, *, #17301, .T. ) ;
#33357 = CARTESIAN_POINT ( 'NONE',  ( 121.2019704359119885, -10.25716656981731489, -12.88942061488890545 ) ) ;
#33358 = CARTESIAN_POINT ( 'NONE',  ( 124.9357681442453014, -1.834011780172310813, -8.268836392978581529 ) ) ;
#33359 = CARTESIAN_POINT ( 'NONE',  ( 125.3303382280772382, -6.508808502060079881, -6.467457712844120188 ) ) ;
#33360 = CARTESIAN_POINT ( 'NONE',  ( 123.8579614775786126, 0.5811942927096110934, -14.16772938898807510 ) ) ;
#33361 = ADVANCED_FACE ( 'NONE', ( #39561 ), #21554, .T. ) ;
#33362 = CARTESIAN_POINT ( 'NONE',  ( 107.9128015045248219, -2.477300249445798297, -7.631215200338321125 ) ) ;
#33363 = EDGE_CURVE ( 'NONE', #31639, #32385, #20938, .T. ) ;
#33364 = EDGE_CURVE ( 'NONE', #8089, #2933, #11870, .T. ) ;
#33365 = CARTESIAN_POINT ( 'NONE',  ( 67.19031194842951038, -1.707697914625855296, -12.39321520033831447 ) ) ;
#33366 = CARTESIAN_POINT ( 'NONE',  ( 127.9202185846628481, -3.082963570468182812, -14.51592808579281701 ) ) ;
#33367 = CARTESIAN_POINT ( 'NONE',  ( 110.6214733795247867, -1.325403438956436419, -9.854619843455211026 ) ) ;
#33368 = DIRECTION ( 'NONE',  ( 1.000000000000000000, 0.000000000000000000, -0.000000000000000000 ) ) ;
#33369 = DIRECTION ( 'NONE',  ( 0.9609149988134843001, -0.1028163501681632064, 0.2570431154366505933 ) ) ;
#33370 = CARTESIAN_POINT ( 'NONE',  ( 117.9016614775786280, -0.1624402480850797581, -16.17319339645315424 ) ) ;
#33371 = CARTESIAN_POINT ( 'NONE',  ( 111.3213681442453264, -7.643976991954077427, -18.09477374809248928 ) ) ;
#33372 = DIRECTION ( 'NONE',  ( 0.9609149988134837450, -0.1028163501681639419, 0.2570431154366518145 ) ) ;
#33373 = ORIENTED_EDGE ( 'NONE', *, *, #3466, .F. ) ;
#33374 = CARTESIAN_POINT ( 'NONE',  ( 115.8639169858783617, -2.378957183258571639, -17.95140958770219086 ) ) ;
#33375 = CARTESIAN_POINT ( 'NONE',  ( 116.7104014775786425, -8.899110576539710493, -16.42337572283490132 ) ) ;
#33376 = CYLINDRICAL_SURFACE ( 'NONE', #33305, 1.999999999999998890 ) ;
#33377 = CARTESIAN_POINT ( 'NONE',  ( 68.15423470349523427, -1.018375365046214620, -10.39321520033831803 ) ) ;
#33378 = CARTESIAN_POINT ( 'NONE',  ( 123.9103448073892508, -1.081026697600536046, -17.18181821144402832 ) ) ;
#33380 = CARTESIAN_POINT ( 'NONE',  ( 123.2906948109119867, -8.166667518702819706, -8.995218007635861213 ) ) ;
#33379 = CARTESIAN_POINT ( 'NONE',  ( 70.79387962571317416, -26.49875194020793501, -5.426084794384776977 ) ) ;
#33381 = CARTESIAN_POINT ( 'NONE',  ( 122.0427081442452817, -9.859900752359378018, -12.68260735090039759 ) ) ;
#33382 = ORIENTED_EDGE ( 'NONE', *, *, #19468, .T. ) ;
#33383 = CYLINDRICAL_SURFACE ( 'NONE', #11312, 5.999999999999997335 ) ;
#33384 = CARTESIAN_POINT ( 'NONE',  ( 66.09777208604641885, -15.19992928687715761, -10.39321520033831625 ) ) ;
#33385 = CARTESIAN_POINT ( 'NONE',  ( 111.6632702545248605, 0.1403307496149616695, -11.32035403202665336 ) ) ;
#33386 = CARTESIAN_POINT ( 'NONE',  ( 122.0994348109119443, -10.15424416112533912, -14.75197769757731336 ) ) ;
#33387 = CARTESIAN_POINT ( 'NONE',  ( 120.9649014775786355, -6.222761293078241884, -8.102969835052219238 ) ) ;
#33388 = CARTESIAN_POINT ( 'NONE',  ( 124.9774582099995683, 1.254580239582103962, -17.90916344451578368 ) ) ;
#33389 = CARTESIAN_POINT ( 'NONE',  ( 115.8304577545247582, -2.791137627527939813, -18.39754474579286025 ) ) ;
#33390 = CARTESIAN_POINT ( 'NONE',  ( 74.66232006577804725, -2.500611837642884527, -9.893215200338316251 ) ) ;
#33391 = CARTESIAN_POINT ( 'NONE',  ( 88.07785292173620917, -25.99489077589524300, -13.39321520033831625 ) ) ;
#33392 = CARTESIAN_POINT ( 'NONE',  ( 61.69189222814998175, -40.21211973637273474, -19.39321520033831447 ) ) ;
#33393 = CARTESIAN_POINT ( 'NONE',  ( 111.1770983795247787, -0.7896495226426338832, -9.318865927141430916 ) ) ;
#33394 = CARTESIAN_POINT ( 'NONE',  ( -13.40747672045794481, -4.990737039574640654, -19.30361446747916787 ) ) ;
#33395 = CARTESIAN_POINT ( 'NONE',  ( 113.0523327545247838, -2.477300249445798297, -19.15521520033831138 ) ) ;
#33396 = CARTESIAN_POINT ( 'NONE',  ( 120.4543614775786295, -4.089484607189486809, -7.948022111789456723 ) ) ;
#33397 = CARTESIAN_POINT ( 'NONE',  ( 122.6099748109119929, -9.261995988541697145, -16.69588392320189030 ) ) ;
#33398 = CARTESIAN_POINT ( 'NONE',  ( 106.7320983795247855, -0.7896495226426338832, -9.318865927141430916 ) ) ;
#33399 = CARTESIAN_POINT ( 'NONE',  ( 115.0086014775786509, -4.089484607189486809, -7.948022111789456723 ) ) ;
#33400 = CARTESIAN_POINT ( 'NONE',  ( 114.1577014775786552, -6.344957434206662583, -7.627207830600332805 ) ) ;
#33401 = VERTEX_POINT ( 'NONE', #28628 ) ;
#33402 = EDGE_CURVE ( 'NONE', #19524, #22169, #22225, .T. ) ;
#33403 = CARTESIAN_POINT ( 'NONE',  ( 112.2289948109119848, -7.643976991954077427, -18.09477374809248928 ) ) ;
#33404 = CARTESIAN_POINT ( 'NONE',  ( 120.0005481442453146, -5.638512984488999180, -18.83840828888717311 ) ) ;
#33405 = CARTESIAN_POINT ( 'NONE',  ( 112.0020881442453344, 0.2603800115204892296, -16.42320221600525088 ) ) ;
#33406 = CARTESIAN_POINT ( 'NONE',  ( 114.0442481442453300, -7.643976991954077427, -18.09477374809248928 ) ) ;
#33407 = EDGE_LOOP ( 'NONE', ( #40505, #8567, #26049, #22615, #36971 ) ) ;
#33408 = CARTESIAN_POINT ( 'NONE',  ( 112.5126281442453120, 0.1319031606808879209, -14.10382304977623669 ) ) ;
#33409 = CARTESIAN_POINT ( 'NONE',  ( 125.2194014775786286, -10.30919188438810075, -12.61870101168855918 ) ) ;
#33410 = CARTESIAN_POINT ( 'NONE',  ( 108.3989733795248753, -8.938348069036489818, -17.46756447353520159 ) ) ;
#33411 = CARTESIAN_POINT ( 'NONE',  ( 118.4689281442453250, -10.15424416112533912, -14.75197769757731336 ) ) ;
#33412 = CARTESIAN_POINT ( 'NONE',  ( 116.7902762465598840, -3.170093105002864231, -18.30519083512918854 ) ) ;
#33413 = CARTESIAN_POINT ( 'NONE',  ( 64.80455967515507609, -63.24213094532785107, -47.38765000594077037 ) ) ;
#33414 = ORIENTED_EDGE ( 'NONE', *, *, #5784, .F. ) ;
#33415 = CIRCLE ( 'NONE', #17434, 2.445500000000004448 ) ;
#33416 = ADVANCED_FACE ( 'NONE', ( #4218 ), #18134, .T. ) ;
#33417 = FACE_OUTER_BOUND ( 'NONE', #22835, .T. ) ;
#33418 = CARTESIAN_POINT ( 'NONE',  ( 121.5321681442453183, -9.988377603198976828, -10.36322818467138340 ) ) ;
#33419 = LINE ( 'NONE', #12940, #38576 ) ;
#33420 = DIRECTION ( 'NONE',  ( 0.5735764363510499342, 0.3127926500124801890, -0.7570804645221008711 ) ) ;
#33421 = CARTESIAN_POINT ( 'NONE',  ( 68.08131077845983725, -0.7911846277411741513, -16.39321520033831447 ) ) ;
#33422 = ADVANCED_FACE ( 'NONE', ( #31586 ), #42537, .T. ) ;
#33423 = DIRECTION ( 'NONE',  ( 0.000000000000000000, 0.000000000000000000, 1.000000000000000000 ) ) ;
#33424 = CARTESIAN_POINT ( 'NONE',  ( 105.6208483795248299, -8.402594152722688392, -16.93181055722141792 ) ) ;
#33425 = CARTESIAN_POINT ( 'NONE',  ( 121.6881423109119709, -9.959231468620755479, -10.70263013195267021 ) ) ;
#33426 = CARTESIAN_POINT ( 'NONE',  ( 124.1983214775786166, -1.833838273342659697, -17.42832698103878286 ) ) ;
#33427 = DIRECTION ( 'NONE',  ( -0.000000000000000000, -0.9284778069183718952, -0.3713878862591649677 ) ) ;
#33428 = CARTESIAN_POINT ( 'NONE',  ( 124.5386814775786206, -5.638512984488999180, -18.83840828888717311 ) ) ;
#33429 = CARTESIAN_POINT ( 'NONE',  ( 117.2209414775786485, -2.084020599724406786, -8.691656652584148546 ) ) ;
#33430 = CARTESIAN_POINT ( 'NONE',  ( 119.7434548109119703, -1.219197665648892759, -17.48381333488896061 ) ) ;
#33431 = ORIENTED_EDGE ( 'NONE', *, *, #31150, .T. ) ;
#33432 = CARTESIAN_POINT ( 'NONE',  ( 123.1205148109119563, -1.834011780172310813, -8.268836392978581529 ) ) ;
#33433 = CARTESIAN_POINT ( 'NONE',  ( 115.9729548109119861, -6.344957434206662583, -7.627207830600332805 ) ) ;
#33434 = CARTESIAN_POINT ( 'NONE',  ( 113.9552233795247815, -1.325403438956436419, -9.854619843455211026 ) ) ;
#33435 = DIRECTION ( 'NONE',  ( 1.000000000000000000, 0.000000000000000000, 0.000000000000000000 ) ) ;
#33436 = CARTESIAN_POINT ( 'NONE',  ( 123.1772414775786189, -5.574606645277164318, -18.38911715685844683 ) ) ;
#33437 = CARTESIAN_POINT ( 'NONE',  ( 124.0281414775786146, -1.834011780172310813, -8.268836392978581529 ) ) ;
#33438 = CARTESIAN_POINT ( 'NONE',  ( 115.1359265045248605, -7.250697342233347165, -19.15521520033831138 ) ) ;
#33439 = CARTESIAN_POINT ( 'NONE',  ( 107.2182702545248105, 0.1403307496149616695, -11.32035403202665336 ) ) ;
#33440 = CARTESIAN_POINT ( 'NONE',  ( 83.23380393269211197, -31.93623664265597739, -23.45566856608283501 ) ) ;
#33441 = CARTESIAN_POINT ( 'NONE',  ( 114.3278814775786429, 0.1319031606808879209, -14.10382304977623669 ) ) ;
#33442 = CARTESIAN_POINT ( 'NONE',  ( 115.8027748109119841, -8.899110576539710493, -16.42337572283490132 ) ) ;
#33443 = VECTOR ( 'NONE', #14698, 1000.000000000000000 ) ;
#33444 = DIRECTION ( 'NONE',  ( 1.000000000000000000, 0.000000000000000000, -0.000000000000000000 ) ) ;
#33445 = CARTESIAN_POINT ( 'NONE',  ( 111.3854577545248645, -2.791137627527939813, -18.39754474579286025 ) ) ;
#33446 = ORIENTED_EDGE ( 'NONE', *, *, #8696, .F. ) ;
#33447 = CARTESIAN_POINT ( 'NONE',  ( 109.2296023670620571, -0.1266929509688458910, -15.29689100126300083 ) ) ;
#33448 = CARTESIAN_POINT ( 'NONE',  ( 125.9001214775786224, -5.574606645277164318, -18.38911715685844683 ) ) ;
#33449 = CARTESIAN_POINT ( 'NONE',  ( 120.5074391859119913, -1.406689858478933353, -17.56299727309130887 ) ) ;
#33450 = CARTESIAN_POINT ( 'NONE',  ( 122.7299391859119737, -8.844754642576884152, -8.592115655440050404 ) ) ;
#33451 = ORIENTED_EDGE ( 'NONE', *, *, #522, .T. ) ;
#33452 = CARTESIAN_POINT ( 'NONE',  ( 143.3676850761856940, -55.76602098829192755, -2.607500914624014232 ) ) ;
#33453 = CARTESIAN_POINT ( 'NONE',  ( 116.9052633095559770, -11.62205044407607879, -21.51620027165634497 ) ) ;
#33454 = ORIENTED_EDGE ( 'NONE', *, *, #29, .F. ) ;
#33455 = CARTESIAN_POINT ( 'NONE',  ( 119.0361948109119652, -7.893985811506177619, -18.51759400769804742 ) ) ;
#33456 = CIRCLE ( 'NONE', #45146, 2.000000000000000444 ) ;
#33457 = CARTESIAN_POINT ( 'NONE',  ( 122.5532481442453019, 0.4262465694468514643, -12.03445270309931736 ) ) ;
#33458 = CARTESIAN_POINT ( 'NONE',  ( 114.3278814775786429, 0.1319031606808879209, -14.10382304977623669 ) ) ;
#33459 = SHAPE_REPRESENTATION_RELATIONSHIP ( 'NONE' , 'NONE' ,  #10805, #16689 ) ;
#33460 = CIRCLE ( 'NONE', #18930, 35.00000000000000000 ) ;
#33461 = CYLINDRICAL_SURFACE ( 'NONE', #30049, 3.000000000000001332 ) ;
#33462 = CARTESIAN_POINT ( 'NONE',  ( 71.83824405425508530, -26.34469659010723674, -4.893215200338314474 ) ) ;
#33463 = CARTESIAN_POINT ( 'NONE',  ( 114.5547881442453217, -5.638512984488999180, -18.83840828888717311 ) ) ;
#33464 = ADVANCED_FACE ( 'NONE', ( #356 ), #14267, .F. ) ;
#33465 = CARTESIAN_POINT ( 'NONE',  ( 113.8163171295247764, 0.1403307496149613920, -13.39321520033831447 ) ) ;
#33466 = CARTESIAN_POINT ( 'NONE',  ( 122.8368814775786291, -1.561330072975668948, -17.79121239304076951 ) ) ;
#33467 = CARTESIAN_POINT ( 'NONE',  ( 121.9470836909669913, -25.99489077589524300, -13.39321520033831447 ) ) ;
#33468 = ORIENTED_EDGE ( 'NONE', *, *, #45086, .T. ) ;
#33469 = CARTESIAN_POINT ( 'NONE',  ( 113.5904348109119866, -7.893985811506177619, -18.51759400769804742 ) ) ;
#33470 = CARTESIAN_POINT ( 'NONE',  ( 115.0086014775786509, -5.574606645277164318, -18.38911715685844683 ) ) ;
#33471 = CARTESIAN_POINT ( 'NONE',  ( 126.2184548109120072, -5.454730531075203004, -18.35951656919957742 ) ) ;
#33472 = CARTESIAN_POINT ( 'NONE',  ( 125.3895814775786448, -2.084020599724406786, -8.691656652584148546 ) ) ;
#33473 = ORIENTED_EDGE ( 'NONE', *, *, #26253, .F. ) ;
#33474 = CARTESIAN_POINT ( 'NONE',  ( 123.0070614775786169, 0.9020085738987339008, -11.91225656197089222 ) ) ;
#33475 = EDGE_CURVE ( 'NONE', #38699, #40576, #7874, .T. ) ;
#33476 = CIRCLE ( 'NONE', #36386, 2.999999999999999556 ) ;
#33477 = DIRECTION ( 'NONE',  ( -0.000000000000000000, -0.9284778069183718952, -0.3713878862591649677 ) ) ;
#33478 = EDGE_CURVE ( 'NONE', #28936, #26194, #44912, .T. ) ;
#33479 = LINE ( 'NONE', #41044, #27699 ) ;
#33480 = CARTESIAN_POINT ( 'NONE',  ( 114.8834831777918879, -0.01829820670803256055, -14.64321520033831447 ) ) ;
#33481 = CARTESIAN_POINT ( 'NONE',  ( 136.8192643132354931, -2.859499808723217296, -8.184084197783032977 ) ) ;
#33482 = CARTESIAN_POINT ( 'NONE',  ( 112.9664414775786412, -9.859900752359374465, -12.68260735090039404 ) ) ;
#33483 = DIRECTION ( 'NONE',  ( -0.9609149988134837450, 0.1028163501681639419, -0.2570431154366518145 ) ) ;
#33484 = AXIS2_PLACEMENT_3D ( 'NONE', #11663, #25572, #1388 ) ;
#33485 = DIRECTION ( 'NONE',  ( 0.000000000000000000, 0.000000000000000000, -1.000000000000000000 ) ) ;
#33486 = CARTESIAN_POINT ( 'NONE',  ( 114.5547881442453217, -4.153390946401321671, -8.397313243818183892 ) ) ;
#33487 = CARTESIAN_POINT ( 'NONE',  ( 111.8886348109120092, -3.383040157471821630, -19.15922257007629170 ) ) ;
#33488 = CARTESIAN_POINT ( 'NONE',  ( 122.5215798109119874, -7.200787124940443817, -17.81845355600750835 ) ) ;
#33489 = CARTESIAN_POINT ( 'NONE',  ( 126.4673881442452910, -7.894159318335828068, -9.358103419637847864 ) ) ;
#33490 = CARTESIAN_POINT ( 'NONE',  ( 117.2776681442452968, -4.153390946401321671, -8.397313243818183892 ) ) ;
#33491 = CARTESIAN_POINT ( 'NONE',  ( 124.8790414775786246, -0.4660016031367893996, -10.09054647747474043 ) ) ;
#33492 = CARTESIAN_POINT ( 'NONE',  ( 122.9503348109119827, 0.5811942927096110934, -14.16772938898807510 ) ) ;
#33493 = ORIENTED_EDGE ( 'NONE', *, *, #16277, .F. ) ;
#33494 = CARTESIAN_POINT ( 'NONE',  ( 113.2500748109119968, -6.344957434206662583, -7.627207830600332805 ) ) ;
#33495 = CARTESIAN_POINT ( 'NONE',  ( 113.9552233795247815, -8.938348069036489818, -17.46756447353520159 ) ) ;
#33496 = CARTESIAN_POINT ( 'NONE',  ( 109.2324108795247923, -1.325403438956436419, -16.93181055722141792 ) ) ;
#33497 = CARTESIAN_POINT ( 'NONE',  ( 107.7738952545248310, -9.868328341294098749, -15.46607636864997204 ) ) ;
#33498 = CARTESIAN_POINT ( 'NONE',  ( 64.25426170852544772, -36.05670985702485609, -5.755590974858822761 ) ) ;
#33499 = CARTESIAN_POINT ( 'NONE',  ( 119.7736414775786358, -10.30919188438810075, -12.61870101168855918 ) ) ;
#33500 = ORIENTED_EDGE ( 'NONE', *, *, #12796, .T. ) ;
#33501 = CARTESIAN_POINT ( 'NONE',  ( 124.7088614775786226, 0.2603800115204892296, -16.42320221600525088 ) ) ;
#33502 = CARTESIAN_POINT ( 'NONE',  ( 109.2294601086458954, -8.543441930476365798, -8.974638458010995024 ) ) ;
#33503 = CARTESIAN_POINT ( 'NONE',  ( 120.9291030939976821, -2.236191541394346061, -18.14152338500401029 ) ) ;
#33504 = CARTESIAN_POINT ( 'NONE',  ( 113.9307948109119764, -10.15424416112533912, -14.75197769757731336 ) ) ;
#33505 = CARTESIAN_POINT ( 'NONE',  ( 105.9681140045248355, 0.1403307496149616695, -15.46607636864997204 ) ) ;
#33506 = CARTESIAN_POINT ( 'NONE',  ( 118.6391081442452986, -4.089484607189486809, -7.948022111789456723 ) ) ;
#33507 = CARTESIAN_POINT ( 'NONE',  ( 108.1211608795247798, -8.938348069036489818, -9.318865927141430916 ) ) ;
#33508 = CARTESIAN_POINT ( 'NONE',  ( 74.64594387179452895, -42.43939829949535181, -16.39321520033831447 ) ) ;
#33509 = ORIENTED_EDGE ( 'NONE', *, *, #27537, .F. ) ;
#33510 = CARTESIAN_POINT ( 'NONE',  ( 120.6812681442452941, 0.1319031606808905299, -14.10382304977622248 ) ) ;
#33511 = CARTESIAN_POINT ( 'NONE',  ( 123.0070614775786169, -10.15424416112533912, -14.75197769757731336 ) ) ;
#33512 = CARTESIAN_POINT ( 'NONE',  ( 120.0572748109119772, -3.383040157471821630, -19.15922257007629170 ) ) ;
#33513 = VECTOR ( 'NONE', #16138, 1000.000000000000000 ) ;
#33514 = CARTESIAN_POINT ( 'NONE',  ( 115.1787814775786387, -0.1624402480850797581, -16.17319339645315424 ) ) ;
#33515 = CARTESIAN_POINT ( 'NONE',  ( 116.7104014775786425, -0.4660016031367893996, -10.09054647747474043 ) ) ;
#33516 = CARTESIAN_POINT ( 'NONE',  ( 89.33740294208338639, -9.098375579515472822, -9.893215200338316251 ) ) ;
#33517 = CARTESIAN_POINT ( 'NONE',  ( 126.8137406967790071, -1.239144018213914622, -9.529331767162547706 ) ) ;
#33518 = CARTESIAN_POINT ( 'NONE',  ( 120.2841814775786276, -10.15424416112533912, -14.75197769757731336 ) ) ;
#33519 = ORIENTED_EDGE ( 'NONE', *, *, #35056, .F. ) ;
#33520 = CARTESIAN_POINT ( 'NONE',  ( 119.6034614775786196, -6.344957434206651037, -7.627207830600339911 ) ) ;
#33521 = AXIS2_PLACEMENT_3D ( 'NONE', #33623, #12916, #20653 ) ;
#33522 = CARTESIAN_POINT ( 'NONE',  ( 112.3424481442453384, -6.344957434206662583, -7.627207830600332805 ) ) ;
#33523 = CARTESIAN_POINT ( 'NONE',  ( 121.7023481442452777, -0.8288870151387760510, -10.36305467784173118 ) ) ;
#33524 = ORIENTED_EDGE ( 'NONE', *, *, #26991, .F. ) ;
#33525 = CIRCLE ( 'NONE', #13894, 2.000000000000003109 ) ;
#33526 = CARTESIAN_POINT ( 'NONE',  ( 120.0907204359119760, 1.345710702986147034, -13.97328579221134426 ) ) ;
#33527 = B_SPLINE_CURVE_WITH_KNOTS ( 'NONE', 3,
 ( #5109, #22894, #25654, #29968, #12423, #5342, #12654, #25871, #36118, #43205, #19478, #36789, #32695, #4662, #5559, #8764, #29066, #8998, #29291, #33359, #19259, #26094, #11746, #1689, #8544, #1249, #15388, #22670, #8320, #35893, #39998, #15608, #22446, #39560, #29515, #11972 ),
 .UNSPECIFIED., .F., .F.,
 ( 4, 2, 2, 2, 2, 1, 2, 2, 2, 2, 2, 2, 2, 1, 2, 2, 2, 2, 4 ),
 ( 0.000000000000000000, 0.06250000000006282475, 0.1250000000001256495, 0.1875000000001884604, 0.2187500000002227940, 0.2343750000002370326, 0.2421875000002444156, 0.2500000000002517986, 0.3750000000002657874, 0.5000000000002797762, 0.6250000000002938760, 0.6875000000003008704, 0.7187500000003042011, 0.7343750000003009815, 0.7421875000002994271, 0.7500000000002977618, 0.8125000000002214895, 0.8750000000001452172, 1.000000000000000000 ),
 .UNSPECIFIED. ) ;
#33528 = CARTESIAN_POINT ( 'NONE',  ( 120.3976348109119812, -1.834011780172310813, -8.268836392978581529 ) ) ;
#33529 = CARTESIAN_POINT ( 'NONE',  ( 114.1635827545248389, -2.477300249445798297, -19.15521520033831138 ) ) ;
#33530 = CARTESIAN_POINT ( 'NONE',  ( 114.7249681442453237, -9.565557343593413364, -10.61323700422348004 ) ) ;
#33531 = EDGE_LOOP ( 'NONE', ( #12598, #2690, #35951, #43266, #32106 ) ) ;
#33532 = ORIENTED_EDGE ( 'NONE', *, *, #16934, .T. ) ;
#33533 = CARTESIAN_POINT ( 'NONE',  ( 126.4673881442452910, -7.894159318335828068, -9.358103419637847864 ) ) ;
#33534 = EDGE_CURVE ( 'NONE', #32851, #34946, #25655, .T. ) ;
#33535 = CARTESIAN_POINT ( 'NONE',  ( 121.1918081442452859, -10.15424416112533912, -14.75197769757731336 ) ) ;
#33536 = CYLINDRICAL_SURFACE ( 'NONE', #20022, 5.000000000000000888 ) ;
#33537 = CARTESIAN_POINT ( 'NONE',  ( 69.36136150295220659, -101.1685209014307674, -50.56525720990386219 ) ) ;
#33538 = CARTESIAN_POINT ( 'NONE',  ( 120.1140014775786398, -1.561330072975668504, -17.79121239304076951 ) ) ;
#33539 = CARTESIAN_POINT ( 'NONE',  ( 106.0375671295248310, -10.62599879583958540, -13.39321520033831447 ) ) ;
#33540 = CIRCLE ( 'NONE', #43764, 2.000000000000000444 ) ;
#33541 = CARTESIAN_POINT ( 'NONE',  ( 117.9016614775786280, -9.988377603198976828, -10.36322818467138340 ) ) ;
#33543 = CARTESIAN_POINT ( 'NONE',  ( 115.5191414775786569, -6.222761293078241884, -8.102969835052219238 ) ) ;
#33542 = CARTESIAN_POINT ( 'NONE',  ( 116.9373081442452929, -8.166667518702817929, -8.995218007635861213 ) ) ;
#33544 = CARTESIAN_POINT ( 'NONE',  ( 124.8790414775786246, -8.899110576539710493, -16.42337572283490132 ) ) ;
#33545 = CARTESIAN_POINT ( 'NONE',  ( 111.7751814775786556, -7.893985811506177619, -18.51759400769804742 ) ) ;
#33546 = ORIENTED_EDGE ( 'NONE', *, *, #6115, .F. ) ;
#33547 = CARTESIAN_POINT ( 'NONE',  ( 124.6521348109119884, -7.894159318335828068, -9.358103419637847864 ) ) ;
#33548 = DIRECTION ( 'NONE',  ( -4.625929269271481378E-15, 1.156482317317870344E-15, 1.000000000000000000 ) ) ;
#33549 = DIRECTION ( 'NONE',  ( -1.000000000000000000, 0.000000000000000000, -0.000000000000000000 ) ) ;
#33550 = CARTESIAN_POINT ( 'NONE',  ( 113.3995983795247895, -0.7896495226426338832, -9.318865927141430916 ) ) ;
#33551 = CIRCLE ( 'NONE', #34287, 2.000000000000000444 ) ;
#33552 = CARTESIAN_POINT ( 'NONE',  ( 111.8716296295247901, -4.863998795839590272, -8.388885654883775800 ) ) ;
#33553 = CARTESIAN_POINT ( 'NONE',  ( 113.8163171295247764, -10.62599879583958540, -13.39321520033831447 ) ) ;
#33554 = CARTESIAN_POINT ( 'NONE',  ( 121.8158014775786171, -5.638512984488999180, -18.83840828888717311 ) ) ;
#33555 = ORIENTED_EDGE ( 'NONE', *, *, #37683, .T. ) ;
#33556 = VECTOR ( 'NONE', #30810, 1000.000000000000114 ) ;
#33557 = CARTESIAN_POINT ( 'NONE',  ( 121.5321681442453183, -9.988377603198976828, -10.36322818467138340 ) ) ;
#33558 = CARTESIAN_POINT ( 'NONE',  ( 119.7434548109119703, -2.613043214085062793, -8.928554074455437473 ) ) ;
#33559 = FACE_OUTER_BOUND ( 'NONE', #7759, .T. ) ;
#33560 = CARTESIAN_POINT ( 'NONE',  ( 119.3765548109119834, 0.9020085738987339008, -11.91225656197089222 ) ) ;
#33561 = CARTESIAN_POINT ( 'NONE',  ( 122.0427081442452817, 0.5811942927096110934, -14.16772938898807510 ) ) ;
#33562 = CARTESIAN_POINT ( 'NONE',  ( 123.2067687714537811, -6.306599966548167124, -18.84486539759072699 ) ) ;
#33563 = CARTESIAN_POINT ( 'NONE',  ( 123.9146881442452894, -10.15424416112533912, -14.75197769757731336 ) ) ;
#33564 = CARTESIAN_POINT ( 'NONE',  ( 125.4400992928798075, -8.599374347808629082, -17.74723756341217396 ) ) ;
#33565 = CARTESIAN_POINT ( 'NONE',  ( 120.8547048109119686, -2.527210466738041728, -8.967976844669124148 ) ) ;
#33566 = EDGE_LOOP ( 'NONE', ( #11577, #26313, #6636, #14571, #13044, #4039 ) ) ;
#33567 = CARTESIAN_POINT ( 'NONE',  ( 70.36267391504958368, -5.685877709920885259, -4.893215200338314474 ) ) ;
#33568 = CARTESIAN_POINT ( 'NONE',  ( 114.6490365460471992, -2.191907684172563986, -18.20049396185734025 ) ) ;
#33569 = CARTESIAN_POINT ( 'NONE',  ( 123.4608748109119745, 0.4262465694468514643, -12.03445270309931736 ) ) ;
#33570 = B_SPLINE_CURVE_WITH_KNOTS ( 'NONE', 3,
 ( #14573, #10491, #13905, #35295, #42172, #27814, #41728, #24393, #38281, #7061, #433, #42395, #17548, #34843, #20971, #10932, #38725, #28041, #14349, #3848, #17768, #10713, #17992, #38497, #11159, #38957, #7725, #24176, #7274, #28263, #44933 ),
 .UNSPECIFIED., .F., .F.,
 ( 4, 2, 2, 1, 1, 1, 2, 2, 2, 1, 1, 1, 2, 2, 2, 1, 2, 2, 4 ),
 ( 0.000000000000000000, 0.2499999999999587552, 0.3749999999999381606, 0.4374999999999273914, 0.4687499999999356626, 0.4843749999999260036, 0.4921874999999357181, 0.4999999999999454880, 0.6250000000000111022, 0.6875000000000333067, 0.7187500000000436318, 0.7343750000000371925, 0.7421875000000338618, 0.7500000000000305311, 0.8125000000000198730, 0.8437500000000134337, 0.8593750000000098810, 0.8750000000000063283, 1.000000000000000000 ),
 .UNSPECIFIED. ) ;
#33571 = CARTESIAN_POINT ( 'NONE',  ( 109.2324108795247923, -1.325403438956436419, -16.93181055722141792 ) ) ;
#33572 = CARTESIAN_POINT ( 'NONE',  ( 111.9410827545248708, -6.936859964151250502, -8.388885654883777576 ) ) ;
#33573 = CARTESIAN_POINT ( 'NONE',  ( 116.2565881442453133, -0.8288870151387760510, -10.36305467784173118 ) ) ;
#33574 = CYLINDRICAL_SURFACE ( 'NONE', #19750, 8.000000000000001776 ) ;
#33575 = CARTESIAN_POINT ( 'NONE',  ( 70.87679208027947197, -26.22245083233618601, -5.471004667883966555 ) ) ;
#33576 = CARTESIAN_POINT ( 'NONE',  ( 113.3635281442453504, -0.1624402480850797581, -16.17319339645315424 ) ) ;
#33577 = CARTESIAN_POINT ( 'NONE',  ( 122.5532481442453019, -10.63000616557722466, -14.87417383870573495 ) ) ;
#33578 = VERTEX_POINT ( 'NONE', #43207 ) ;
#33579 = CARTESIAN_POINT ( 'NONE',  ( 121.2485348109119769, -8.899110576539710493, -16.42337572283490132 ) ) ;
#33580 = CARTESIAN_POINT ( 'NONE',  ( 116.0864081442453113, -9.988377603198976828, -10.36322818467138340 ) ) ;
#33581 = AXIS2_PLACEMENT_3D ( 'NONE', #44348, #24272, #13108 ) ;
#33582 = CARTESIAN_POINT ( 'NONE',  ( 125.3328548109119964, -9.261995988541697145, -16.69588392320189030 ) ) ;
#33583 = PRODUCT_DEFINITION ( 'UNKNOWN', '', #3109, #36051 ) ;
#33584 = CARTESIAN_POINT ( 'NONE',  ( 123.5176014775786228, -0.8288870151387760510, -10.36305467784173118 ) ) ;
#33585 = EDGE_LOOP ( 'NONE', ( #43353, #30510 ) ) ;
#33586 = CARTESIAN_POINT ( 'NONE',  ( 123.6519830939976572, -2.236191541394346061, -18.14152338500401029 ) ) ;
#33587 = AXIS2_PLACEMENT_3D ( 'NONE', #39923, #22588, #33284 ) ;
#33588 = CARTESIAN_POINT ( 'NONE',  ( 124.1415948109119540, -6.344957434206665248, -7.627207830600338134 ) ) ;
#33589 = CARTESIAN_POINT ( 'NONE',  ( 113.5337081442453240, -0.8288870151387760510, -10.36305467784173118 ) ) ;
#33590 = CARTESIAN_POINT ( 'NONE',  ( 126.0135748109119902, -8.166667518702819706, -8.995218007635861213 ) ) ;
#33591 = CARTESIAN_POINT ( 'NONE',  ( 108.6073327545248048, -2.477300249445798297, -19.15521520033831138 ) ) ;
#33592 = CARTESIAN_POINT ( 'NONE',  ( 88.07785292173620917, -25.99489077589524300, -13.39321520033831625 ) ) ;
#33593 = VERTEX_POINT ( 'NONE', #12426 ) ;
#33594 = CARTESIAN_POINT ( 'NONE',  ( 127.9566280595583692, -3.013114159214123511, -14.60907972933637566 ) ) ;
#33595 = CARTESIAN_POINT ( 'NONE',  ( 110.9687390045248350, -9.868328341294098749, -11.32035403202665869 ) ) ;
#33596 = DIRECTION ( 'NONE',  ( 0.000000000000000000, 0.000000000000000000, -1.000000000000000000 ) ) ;
#33597 = CARTESIAN_POINT ( 'NONE',  ( 119.4900081442453086, -7.643976991954077427, -18.09477374809248928 ) ) ;
#33598 = CARTESIAN_POINT ( 'NONE',  ( 112.7962614775786676, -6.222761293078241884, -8.102969835052219238 ) ) ;
#33599 = CARTESIAN_POINT ( 'NONE',  ( 127.0150841466615930, -0.0006450967245569220066, -11.05022577389757465 ) ) ;
#33600 = ORIENTED_EDGE ( 'NONE', *, *, #31684, .F. ) ;
#33601 = DIRECTION ( 'NONE',  ( 0.000000000000000000, 0.7876185884367603585, -0.6161630946014904353 ) ) ;
#33602 = CARTESIAN_POINT ( 'NONE',  ( 115.3489614775786407, -0.8288870151387760510, -10.36305467784173118 ) ) ;
#33603 = DIRECTION ( 'NONE',  ( 1.000000000000000000, 0.000000000000000000, 0.000000000000000000 ) ) ;
#33605 = VECTOR ( 'NONE', #22186, 1000.000000000000000 ) ;
#33604 = CARTESIAN_POINT ( 'NONE',  ( 68.04603467680756523, -0.7145533168453219730, -10.39321520033831980 ) ) ;
#33606 = DIRECTION ( 'NONE',  ( -0.9908103287288504424, 0.1352586133457950590, 0.000000000000000000 ) ) ;
#33608 = CARTESIAN_POINT ( 'NONE',  ( 124.1983214775786166, -8.166667518702819706, -8.995218007635861213 ) ) ;
#33607 = FACE_OUTER_BOUND ( 'NONE', #23183, .T. ) ;
#33609 = CARTESIAN_POINT ( 'NONE',  ( 122.7234281442452755, -4.153390946401325223, -8.397313243818185668 ) ) ;
#33610 = ORIENTED_EDGE ( 'NONE', *, *, #25664, .F. ) ;
#33611 = CARTESIAN_POINT ( 'NONE',  ( 114.6460952706805756, 0.3193521225029610777, -14.64321520033831447 ) ) ;
#33612 = CARTESIAN_POINT ( 'NONE',  ( 89.70384154612264638, -12.43804770190545561, -8.143215200338314474 ) ) ;
#33613 = CARTESIAN_POINT ( 'NONE',  ( 109.5796765045248122, -2.791137627527939813, -8.388885654883777576 ) ) ;
#33614 = CARTESIAN_POINT ( 'NONE',  ( 126.6375681442452930, -10.15424416112533912, -14.75197769757731336 ) ) ;
#33615 = CARTESIAN_POINT ( 'NONE',  ( 118.5256548109119876, -8.899110576539710493, -16.42337572283490132 ) ) ;
#33616 = CARTESIAN_POINT ( 'NONE',  ( 124.8633137343444446, 2.423166897745142823, -15.87367557320988531 ) ) ;
#33617 = CARTESIAN_POINT ( 'NONE',  ( 106.0375671295248310, -10.62599879583958540, -13.39321520033831447 ) ) ;
#33618 = AXIS2_PLACEMENT_3D ( 'NONE', #30114, #44030, #33739 ) ;
#33619 = LINE ( 'NONE', #40953, #37540 ) ;
#33620 = CARTESIAN_POINT ( 'NONE',  ( 112.2857214775786474, -5.574606645277172312, -18.38911715685844683 ) ) ;
#33621 = CARTESIAN_POINT ( 'NONE',  ( 114.6115148109119986, -6.222761293078241884, -8.102969835052219238 ) ) ;
#33622 = CARTESIAN_POINT ( 'NONE',  ( 112.0105358795247810, -0.7896495226426338832, -17.46756447353520159 ) ) ;
#33623 = CARTESIAN_POINT ( 'NONE',  ( 119.7434548109119703, -4.863998795839242995, -13.39321520033831447 ) ) ;
#33624 = CARTESIAN_POINT ( 'NONE',  ( 113.1217858795247935, -0.7896495226426338832, -17.46756447353520159 ) ) ;
#33625 = CARTESIAN_POINT ( 'NONE',  ( 122.3263414775786373, -6.344957434206665248, -7.627207830600338134 ) ) ;
#33626 = CARTESIAN_POINT ( 'NONE',  ( 123.1772414775786189, -4.089484607189486809, -7.948022111789456723 ) ) ;
#33627 = CARTESIAN_POINT ( 'NONE',  ( 114.5803015045248259, -2.477300249445798297, -7.631215200338321125 ) ) ;
#33628 = CARTESIAN_POINT ( 'NONE',  ( 117.5045748109119756, 0.5811942927096110934, -14.16772938898807510 ) ) ;
#33629 = EDGE_CURVE ( 'NONE', #20112, #24167, #21333, .T. ) ;
#33630 = ADVANCED_FACE ( 'NONE', ( #18806 ), #33693, .T. ) ;
#33631 = CARTESIAN_POINT ( 'NONE',  ( 114.3846081442453197, -10.63000616557722466, -14.87417383870573495 ) ) ;
#33632 = VERTEX_POINT ( 'NONE', #30198 ) ;
#33633 = CARTESIAN_POINT ( 'NONE',  ( 114.7816948109119863, -9.859900752359374465, -12.68260735090039404 ) ) ;
#33634 = CARTESIAN_POINT ( 'NONE',  ( 113.0798948109119948, -8.899110576539710493, -16.42337572283490132 ) ) ;
#33635 = CARTESIAN_POINT ( 'NONE',  ( 121.4187148109119789, -6.344957434206665248, -7.627207830600338134 ) ) ;
#33636 = CARTESIAN_POINT ( 'NONE',  ( 124.7088614775786226, -9.565557343593413364, -10.61323700422348004 ) ) ;
#33637 = CARTESIAN_POINT ( 'NONE',  ( 113.3635281442453504, -0.1624402480850797581, -16.17319339645315424 ) ) ;
#33638 = ORIENTED_EDGE ( 'NONE', *, *, #5225, .F. ) ;
#33639 = CARTESIAN_POINT ( 'NONE',  ( 118.8660148109119774, 0.1319031606808879209, -14.10382304977623669 ) ) ;
#33640 = CARTESIAN_POINT ( 'NONE',  ( 124.1983214775786166, -8.166667518702819706, -8.995218007635861213 ) ) ;
#33641 = AXIS2_PLACEMENT_3D ( 'NONE', #3248, #31503, #14184 ) ;
#33642 = CARTESIAN_POINT ( 'NONE',  ( 111.2465515045248168, -2.477300249445798297, -7.631215200338321125 ) ) ;
#33643 = CIRCLE ( 'NONE', #42427, 1.999999999999998890 ) ;
#33644 = CARTESIAN_POINT ( 'NONE',  ( 119.2631014775786298, -9.565557343593413364, -10.61323700422348004 ) ) ;
#33645 = CARTESIAN_POINT ( 'NONE',  ( 128.2184548109119930, -4.105398160058917334, -19.34506575923121474 ) ) ;
#33646 = ORIENTED_EDGE ( 'NONE', *, *, #26167, .F. ) ;
#33647 = CARTESIAN_POINT ( 'NONE',  ( 123.2161110609119703, -6.340755971794695078, -8.611740276972781771 ) ) ;
#33648 = CARTESIAN_POINT ( 'NONE',  ( 122.7234281442452755, -5.638512984488999180, -18.83840828888717311 ) ) ;
#33649 = EDGE_CURVE ( 'NONE', #29947, #25821, #19482, .T. ) ;
#33650 = CARTESIAN_POINT ( 'NONE',  ( 113.6079577545248185, -2.791137627527887410, -18.39754474579284249 ) ) ;
#33651 = AXIS2_PLACEMENT_3D ( 'NONE', #6817, #6367, #31198 ) ;
#33652 = CARTESIAN_POINT ( 'NONE',  ( 112.5693548109119888, -10.63000616557722466, -14.87417383870573495 ) ) ;
#33653 = CARTESIAN_POINT ( 'NONE',  ( 94.20708369096698220, -25.56540164683820393, -12.65854514648976981 ) ) ;
#33654 = ADVANCED_FACE ( 'NONE', ( #43886 ), #29971, .F. ) ;
#33655 = CARTESIAN_POINT ( 'NONE',  ( 107.8433483795247838, -8.402594152722688392, -16.93181055722141792 ) ) ;
#33656 = CARTESIAN_POINT ( 'NONE',  ( 121.6186891859119754, -8.844754642576878823, -8.592115655440055733 ) ) ;
#33657 = CARTESIAN_POINT ( 'NONE',  ( 137.5058127635946335, -5.720712770326367824, -18.32462370007482377 ) ) ;
#33658 = ADVANCED_FACE ( 'NONE', ( #26553 ), #8975, .T. ) ;
#33659 = CARTESIAN_POINT ( 'NONE',  ( 125.1008810305878001, -2.476927793680328449, -17.82094707215535578 ) ) ;
#33660 = CARTESIAN_POINT ( 'NONE',  ( 124.0527235609119714, -0.08666061303663243065, -11.91773565553389425 ) ) ;
#33661 = CARTESIAN_POINT ( 'NONE',  ( 118.9227414775786542, 0.4262465694468514643, -12.03445270309931736 ) ) ;
#33662 = CARTESIAN_POINT ( 'NONE',  ( 119.7434548109119561, -0.09372932658121500837, -15.89155818700682943 ) ) ;
#33663 = ORIENTED_EDGE ( 'NONE', *, *, #24193, .F. ) ;
#33664 = CARTESIAN_POINT ( 'NONE',  ( 124.1415948109119540, -6.344957434206665248, -7.627207830600338134 ) ) ;
#33665 = CARTESIAN_POINT ( 'NONE',  ( 115.2355081442453155, -10.30919188438810075, -12.61870101168855918 ) ) ;
#33666 = CARTESIAN_POINT ( 'NONE',  ( 115.2053796295247849, -4.863998795839590272, -8.388885654883775800 ) ) ;
#33667 = CARTESIAN_POINT ( 'NONE',  ( 125.1309504620138284, -2.495269033102075262, -17.79652296963211455 ) ) ;
#33668 = CARTESIAN_POINT ( 'NONE',  ( 122.6667014775786413, -2.084020599724406786, -8.691656652584148546 ) ) ;
#33669 = EDGE_CURVE ( 'NONE', #25347, #22341, #44118, .T. ) ;
#33671 = CARTESIAN_POINT ( 'NONE',  ( 125.9001214775786224, -4.089484607189486809, -7.948022111789456723 ) ) ;
#33670 = AXIS2_PLACEMENT_3D ( 'NONE', #20320, #2752, #16677 ) ;
#33672 = CARTESIAN_POINT ( 'NONE',  ( 115.4137390045248566, 0.8980012041604421569, -15.77991374673208469 ) ) ;
#33673 = CARTESIAN_POINT ( 'NONE',  ( 108.6767858795247861, -8.402594152722688392, -9.854619843455216355 ) ) ;
#33674 = CARTESIAN_POINT ( 'NONE',  ( 124.1570456159114286, -12.80247570057301587, -14.38293432349187384 ) ) ;
#33675 = CARTESIAN_POINT ( 'NONE',  ( 115.8027748109119841, -8.899110576539710493, -16.42337572283490132 ) ) ;
#33676 = CONICAL_SURFACE ( 'NONE', #10405, 1.610000000000000986, 0.9599310885968765916 ) ;
#33677 = CARTESIAN_POINT ( 'NONE',  ( 116.0296814775786345, -1.833838273342658809, -17.42832698103878286 ) ) ;
#33678 = CARTESIAN_POINT ( 'NONE',  ( 70.19189222814998175, -42.69543048370626792, -27.04993751765913501 ) ) ;
#33679 = CARTESIAN_POINT ( 'NONE',  ( 115.2748327545248657, -6.936859964151250502, -8.388885654883777576 ) ) ;
#33680 = ORIENTED_EDGE ( 'NONE', *, *, #37017, .F. ) ;
#33681 = EDGE_CURVE ( 'NONE', #35835, #8254, #17691, .T. ) ;
#33682 = CYLINDRICAL_SURFACE ( 'NONE', #28406, 1.587500000000000577 ) ;
#33683 = CARTESIAN_POINT ( 'NONE',  ( 124.1983214775786166, -1.833838273342659697, -17.42832698103878286 ) ) ;
#33684 = CARTESIAN_POINT ( 'NONE',  ( 122.9382985609119743, -10.36940331770106916, -15.09355782777062061 ) ) ;
#33685 = CARTESIAN_POINT ( 'NONE',  ( 124.1884548109119777, -7.554583864224885481, -18.48844787311982785 ) ) ;
#33686 = ADVANCED_FACE ( 'NONE', ( #23360 ), #40248, .T. ) ;
#33687 = EDGE_CURVE ( 'NONE', #20823, #5058, #12597, .T. ) ;
#33688 = ORIENTED_EDGE ( 'NONE', *, *, #22078, .T. ) ;
#33689 =( GEOMETRIC_REPRESENTATION_CONTEXT ( 3 ) GLOBAL_UNCERTAINTY_ASSIGNED_CONTEXT ( ( #41585 ) ) GLOBAL_UNIT_ASSIGNED_CONTEXT ( ( #23464, #9782, #30746 ) ) REPRESENTATION_CONTEXT ( 'NONE', 'WORKASPACE' ) );
#33690 = CARTESIAN_POINT ( 'NONE',  ( 123.5827482314454926, -3.123236290774572321, -14.46231915649883959 ) ) ;
#33691 = CARTESIAN_POINT ( 'NONE',  ( 116.8978462035280330, -11.63045278355507328, -21.50838919663385340 ) ) ;
#33692 = ORIENTED_EDGE ( 'NONE', *, *, #20891, .T. ) ;
#33693 = CONICAL_SURFACE ( 'NONE', #27896, 2.999999999999999556, 0.9599310885968830309 ) ;
#33694 = CARTESIAN_POINT ( 'NONE',  ( 119.4900081442453086, -1.834011780172310813, -8.268836392978581529 ) ) ;
#33695 = CARTESIAN_POINT ( 'NONE',  ( 123.4608748109119745, 0.4262465694468514643, -12.03445270309931736 ) ) ;
#33696 = CARTESIAN_POINT ( 'NONE',  ( 115.6893214775786447, -9.859900752359374465, -12.68260735090039404 ) ) ;
#33697 =( LENGTH_UNIT ( ) NAMED_UNIT ( * ) SI_UNIT ( .MILLI., .METRE. ) );
#33698 = CARTESIAN_POINT ( 'NONE',  ( 70.89841814381148311, -68.89136543047671069, -37.69090763720760151 ) ) ;
#33699 = CARTESIAN_POINT ( 'NONE',  ( 122.9503348109119827, 0.5811942927096110934, -14.16772938898807510 ) ) ;
#33700 = CARTESIAN_POINT ( 'NONE',  ( 114.6682414775786469, -1.561330072975668060, -17.79121239304076596 ) ) ;
#33701 = CARTESIAN_POINT ( 'NONE',  ( 113.3301452545248083, -9.868328341294098749, -15.46607636864997204 ) ) ;
#33702 = CARTESIAN_POINT ( 'NONE',  ( 125.7299414775786346, 0.9020085738987339008, -11.91225656197089222 ) ) ;
#33703 = DIRECTION ( 'NONE',  ( 0.000000000000000000, 0.000000000000000000, -1.000000000000000000 ) ) ;
#33704 = ORIENTED_EDGE ( 'NONE', *, *, #38175, .T. ) ;
#33705 = CARTESIAN_POINT ( 'NONE',  ( 114.7249681442453237, 0.2603800115204892296, -16.42320221600525088 ) ) ;
#33706 = CARTESIAN_POINT ( 'NONE',  ( 115.4624148109119943, -4.153390946401321671, -8.397313243818183892 ) ) ;
#33707 = TOROIDAL_SURFACE ( 'NONE', #43926, 7.132259260909269649, 2.000000000000000000 ) ;
#33708 = DIRECTION ( 'NONE',  ( 0.000000000000000000, -0.9284778069183718952, -0.3713878862591650232 ) ) ;
#33709 = CARTESIAN_POINT ( 'NONE',  ( 113.6471614775786492, -5.638512984488999180, -18.83840828888717311 ) ) ;
#33710 = ORIENTED_EDGE ( 'NONE', *, *, #41595, .T. ) ;
#33711 = AXIS2_PLACEMENT_3D ( 'NONE', #764, #18783, #7612 ) ;
#33712 = CARTESIAN_POINT ( 'NONE',  ( 121.3619881442452879, -4.089484607189486809, -7.948022111789456723 ) ) ;
#33713 = PLANE ( 'NONE',  #38327 ) ;
#33714 = CARTESIAN_POINT ( 'NONE',  ( 110.0658483795247804, -8.402594152722633325, -16.93181055722145345 ) ) ;
#33715 = CARTESIAN_POINT ( 'NONE',  ( 124.8179714740559234, -1.081026697600536934, -17.18181821144403187 ) ) ;
#33716 = CARTESIAN_POINT ( 'NONE',  ( 116.6536748109119941, -10.15424416112533912, -14.75197769757731336 ) ) ;
#33717 = CARTESIAN_POINT ( 'NONE',  ( 68.14371629974728251, -1.351251493923715685, -16.39321520033831447 ) ) ;
#33718 = CARTESIAN_POINT ( 'NONE',  ( 115.4624148109119943, -4.153390946401321671, -8.397313243818183892 ) ) ;
#33719 = DIRECTION ( 'NONE',  ( 0.000000000000000000, 0.9284778069183720062, 0.3713878862591650232 ) ) ;
#33720 = CIRCLE ( 'NONE', #28673, 2.000000000000000444 ) ;
#33721 = CARTESIAN_POINT ( 'NONE',  ( 125.2103759035168338, -1.921298038565348199, -20.10252925763280984 ) ) ;
#33722 = CARTESIAN_POINT ( 'NONE',  ( 115.4624148109119943, -4.153390946401321671, -8.397313243818183892 ) ) ;
#33723 = CARTESIAN_POINT ( 'NONE',  ( 116.3700414775786527, -5.638512984488999180, -18.83840828888717311 ) ) ;
#33724 = CARTESIAN_POINT ( 'NONE',  ( 119.7434548109119703, -7.554583864224885481, -18.48844787311982785 ) ) ;
#33725 = CARTESIAN_POINT ( 'NONE',  ( 126.0135748109119902, -1.833838273342660141, -17.42832698103878286 ) ) ;
#33726 = CARTESIAN_POINT ( 'NONE',  ( 113.8740681442453138, -9.859900752359374465, -12.68260735090039404 ) ) ;
#33727 = CARTESIAN_POINT ( 'NONE',  ( 124.9924948109119924, -4.089484607189486809, -7.948022111789456723 ) ) ;
#33728 = ADVANCED_FACE ( 'NONE', ( #33142 ), #2381, .T. ) ;
#33729 = CARTESIAN_POINT ( 'NONE',  ( 121.0216281442452981, -1.561330072975668948, -17.79121239304076951 ) ) ;
#33730 = ORIENTED_EDGE ( 'NONE', *, *, #857, .T. ) ;
#33731 = CARTESIAN_POINT ( 'NONE',  ( 113.1933481442453058, -4.089484607189486809, -7.948022111789456723 ) ) ;
#33732 = CARTESIAN_POINT ( 'NONE',  ( 112.7050671295247923, -10.62599879583958540, -13.39321520033831447 ) ) ;
#33733 = CARTESIAN_POINT ( 'NONE',  ( 105.4819421295248247, -9.868328341294093420, -13.39321520033831447 ) ) ;
#33734 = DIRECTION ( 'NONE',  ( -1.000000000000000000, 0.000000000000000000, -0.000000000000000000 ) ) ;
#33735 = CARTESIAN_POINT ( 'NONE',  ( 128.1232624476561739, -3.897116775730919080, -15.92989199573930925 ) ) ;
#33736 = CARTESIAN_POINT ( 'NONE',  ( 118.7525614775786380, -8.166667518702819706, -8.995218007635861213 ) ) ;
#33737 = EDGE_LOOP ( 'NONE', ( #19639, #19227, #16884, #34803, #6942 ) ) ;
#33738 = CARTESIAN_POINT ( 'NONE',  ( 125.2194014775786286, -10.30919188438810075, -12.61870101168855918 ) ) ;
#33739 = DIRECTION ( 'NONE',  ( 0.000000000000000000, -0.9242245927363028635, -0.3818493186865930533 ) ) ;
#33740 = CARTESIAN_POINT ( 'NONE',  ( 114.4980614775786734, -2.084020599724406786, -8.691656652584148546 ) ) ;
#33741 =( BOUNDED_CURVE ( )  B_SPLINE_CURVE ( 2, ( #19676, #14351, #13079, #31225, #16270, #38283, #6226, #33798, #10493, #9651, #7063, #8216, #20973, #42174, #34845, #24616, #17550 ),
 .UNSPECIFIED., .F., .T. ) 
 B_SPLINE_CURVE_WITH_KNOTS ( ( 3, 2, 2, 2, 2, 2, 2, 2, 3 ),
 ( 0.2670046674808919662, 0.2734375000000000000, 0.2812500000000000000, 0.2890625000000000000, 0.2968750000000000000, 0.3046875000000000000, 0.3125000000000000000, 0.3203125000000000000, 0.3267453325190585178 ),
 .UNSPECIFIED. ) 
 CURVE ( )  GEOMETRIC_REPRESENTATION_ITEM ( )  RATIONAL_B_SPLINE_CURVE ( ( 0.9778625265006459788, 0.9373222120152210346, 1.000000000000000000, 0.9238795325112869605, 1.000000000000000000, 0.9238795325112869605, 1.000000000000000000, 0.9238795325112869605, 1.000000000000000000, 0.9238795325112869605, 1.000000000000000000, 0.9238795325112869605, 1.000000000000000000, 0.9238795325112869605, 1.000000000000000000, 0.9373222120157019832, 0.9778625265000240319 ) ) 
 REPRESENTATION_ITEM ( '' )  );
#33742 = DIRECTION ( 'NONE',  ( 1.000000000000000000, 0.000000000000000000, -0.000000000000000000 ) ) ;
#33743 = CARTESIAN_POINT ( 'NONE',  ( 120.4543614775786295, -4.089484607189486809, -7.948022111789456723 ) ) ;
#33744 = VECTOR ( 'NONE', #32735, 1000.000000000000114 ) ;
#33745 = CARTESIAN_POINT ( 'NONE',  ( 107.9822546295247889, -4.863998795839590272, -7.631215200338315796 ) ) ;
#33746 = FACE_OUTER_BOUND ( 'NONE', #39016, .T. ) ;
#33747 = ORIENTED_EDGE ( 'NONE', *, *, #35001, .T. ) ;
#33748 = CARTESIAN_POINT ( 'NONE',  ( 69.69189222815028018, -41.76310523276638520, -10.39321520033831625 ) ) ;
#33749 = CARTESIAN_POINT ( 'NONE',  ( 123.6310548109119765, -4.153390946401325223, -8.397313243818185668 ) ) ;
#33750 = AXIS2_PLACEMENT_3D ( 'NONE', #23748, #27613, #37857 ) ;
#33751 = CARTESIAN_POINT ( 'NONE',  ( 121.0216281442452981, -1.561330072975668948, -17.79121239304076951 ) ) ;
#33752 = CARTESIAN_POINT ( 'NONE',  ( 114.8951481442453115, -8.899110576539710493, -16.42337572283490132 ) ) ;
#33753 = CARTESIAN_POINT ( 'NONE',  ( 115.1787814775786387, -9.988377603198976828, -10.36322818467138340 ) ) ;
#33754 = LINE ( 'NONE', #12581, #3801 ) ;
#33755 = EDGE_CURVE ( 'NONE', #32861, #20113, #24255, .T. ) ;
#33756 = CARTESIAN_POINT ( 'NONE',  ( 127.0298367773230979, -1.258840796252208127, -9.365270548298379794 ) ) ;
#33757 = CARTESIAN_POINT ( 'NONE',  ( 120.7379948109119709, 0.4262465694468514643, -12.03445270309931736 ) ) ;
#33758 = ORIENTED_EDGE ( 'NONE', *, *, #41864, .F. ) ;
#33759 = CARTESIAN_POINT ( 'NONE',  ( 123.6328298109119714, -2.173413727453600508, -8.297982527556802879 ) ) ;
#33760 = AXIS2_PLACEMENT_3D ( 'NONE', #36302, #39517, #39288 ) ;
#33761 = CARTESIAN_POINT ( 'NONE',  ( 113.1933481442453058, -4.089484607189486809, -7.948022111789456723 ) ) ;
#33762 = CARTESIAN_POINT ( 'NONE',  ( 119.6601881442453106, -1.833838273342659253, -17.42832698103878286 ) ) ;
#33763 = ORIENTED_EDGE ( 'NONE', *, *, #2480, .F. ) ;
#33764 = CARTESIAN_POINT ( 'NONE',  ( 121.4103298109119748, -7.200787124940443817, -17.81845355600750835 ) ) ;
#33765 = CARTESIAN_POINT ( 'NONE',  ( 118.8660148109119774, -10.30919188438810075, -12.61870101168855918 ) ) ;
#33766 = CARTESIAN_POINT ( 'NONE',  ( 111.3160046295247838, -4.863998795839590272, -7.631215200338315796 ) ) ;
#33767 = CARTESIAN_POINT ( 'NONE',  ( 117.7314814775786260, -5.574606645277164318, -18.38911715685844683 ) ) ;
#33768 = VERTEX_POINT ( 'NONE', #36341 ) ;
#33769 = ORIENTED_EDGE ( 'NONE', *, *, #2761, .T. ) ;
#33770 = CARTESIAN_POINT ( 'NONE',  ( 112.2289948109119848, -1.834011780172310813, -8.268836392978581529 ) ) ;
#33771 = CARTESIAN_POINT ( 'NONE',  ( 121.4754414775786131, -1.833838273342659697, -17.42832698103878286 ) ) ;
#33772 = CARTESIAN_POINT ( 'NONE',  ( 85.04324155394569118, -27.84333996136784961, -14.15691383771150136 ) ) ;
#33773 = CARTESIAN_POINT ( 'NONE',  ( 69.69189222815028018, -41.76310523276638520, -16.39321520033831447 ) ) ;
#33774 = CARTESIAN_POINT ( 'NONE',  ( 118.1285681442453068, -7.893985811506177619, -18.51759400769804742 ) ) ;
#33775 = CARTESIAN_POINT ( 'NONE',  ( 105.8292077545248446, -7.250697342233347165, -7.631215200338321125 ) ) ;
#33776 = CARTESIAN_POINT ( 'NONE',  ( 120.9649014775786355, -3.383040157471821630, -19.15922257007629170 ) ) ;
#33778 = CARTESIAN_POINT ( 'NONE',  ( 119.4332814775786318, -8.899110576539710493, -16.42337572283490132 ) ) ;
#33777 = CARTESIAN_POINT ( 'NONE',  ( 115.6325948109119821, 0.2603800115204892296, -16.42320221600525088 ) ) ;
#33779 = CARTESIAN_POINT ( 'NONE',  ( 123.9714148109119805, -8.899110576539710493, -16.42337572283490132 ) ) ;
#33780 = FACE_OUTER_BOUND ( 'NONE', #19572, .T. ) ;
#33781 = ORIENTED_EDGE ( 'NONE', *, *, #15292, .T. ) ;
#33782 = CARTESIAN_POINT ( 'NONE',  ( 124.7655881442452852, -9.859900752359378018, -12.68260735090039759 ) ) ;
#33783 = CARTESIAN_POINT ( 'NONE',  ( 123.7253032127138397, -2.191907684172563986, -18.20049396185734025 ) ) ;
#33784 = CARTESIAN_POINT ( 'NONE',  ( 125.8328548109119964, -8.862178061931794915, -16.39564131203325559 ) ) ;
#33785 = CARTESIAN_POINT ( 'NONE',  ( 108.3989733795248753, -8.938348069036489818, -17.46756447353520159 ) ) ;
#33786 = CARTESIAN_POINT ( 'NONE',  ( 111.1770983795247787, -8.402594152722688392, -16.93181055722141792 ) ) ;
#33787 = CARTESIAN_POINT ( 'NONE',  ( 112.0799890045248475, 0.8980012041604421569, -15.77991374673208469 ) ) ;
#33788 = CARTESIAN_POINT ( 'NONE',  ( 121.0783548109119749, 0.2603800115204892296, -16.42320221600525088 ) ) ;
#33789 = CARTESIAN_POINT ( 'NONE',  ( 123.8579614775786126, -9.859900752359378018, -12.68260735090039759 ) ) ;
#33790 = VERTEX_POINT ( 'NONE', #43435 ) ;
#33791 = CARTESIAN_POINT ( 'NONE',  ( 124.9924948109119924, -4.089484607189486809, -7.948022111789456723 ) ) ;
#33792 = CARTESIAN_POINT ( 'NONE',  ( 113.8740681442453138, -9.859900752359374465, -12.68260735090039404 ) ) ;
#33793 = FACE_OUTER_BOUND ( 'NONE', #15043, .T. ) ;
#33794 = CARTESIAN_POINT ( 'NONE',  ( 120.6245414775786458, -9.988377603198976828, -10.36322818467138340 ) ) ;
#33795 = CARTESIAN_POINT ( 'NONE',  ( 122.4965214775786251, -10.30919188438810075, -12.61870101168855918 ) ) ;
#33796 = CARTESIAN_POINT ( 'NONE',  ( 123.1158699480702552, -6.365377317481717867, -18.95617363400926081 ) ) ;
#33797 = CARTESIAN_POINT ( 'NONE',  ( 122.3263414775786373, -3.505236298600246325, -18.68346056562440793 ) ) ;
#33798 = CARTESIAN_POINT ( 'NONE',  ( 115.9729548109120003, -6.344957434206662583, -7.627207830600333693 ) ) ;
#33799 = DIRECTION ( 'NONE',  ( 0.1352586133457981954, 0.9908103287288499983, 0.000000000000000000 ) ) ;
#33800 = ORIENTED_EDGE ( 'NONE', *, *, #37354, .F. ) ;
#33801 = CARTESIAN_POINT ( 'NONE',  ( -2.065049201022524539, -6.904086573307711916, -7.826012730671462414 ) ) ;
#33802 = CARTESIAN_POINT ( 'NONE',  ( 112.3991748109119868, -1.833838273342658809, -17.42832698103878286 ) ) ;
#33803 = CARTESIAN_POINT ( 'NONE',  ( 123.6877814775786533, -6.222761293078241884, -8.102969835052219238 ) ) ;
#33804 = ADVANCED_FACE ( 'NONE', ( #9227 ), #38477, .F. ) ;
#33805 = CARTESIAN_POINT ( 'NONE',  ( 106.7320983795247855, -8.402594152722688392, -16.93181055722141792 ) ) ;
#33806 = CARTESIAN_POINT ( 'NONE',  ( 110.4131140045248287, 0.1403307496149616695, -15.46607636864997204 ) ) ;
#33807 = CARTESIAN_POINT ( 'NONE',  ( 117.2776681442452968, -4.153390946401325223, -8.397313243818185668 ) ) ;
#33808 = CARTESIAN_POINT ( 'NONE',  ( 70.72798458804651034, -25.12338242182658732, -5.471004667884126427 ) ) ;
#33809 = CARTESIAN_POINT ( 'NONE',  ( 114.8384214775786489, -10.15424416112533912, -14.75197769757731336 ) ) ;
#33810 = CARTESIAN_POINT ( 'NONE',  ( 123.1205148109119563, -1.834011780172310813, -8.268836392978581529 ) ) ;
#33811 = ORIENTED_EDGE ( 'NONE', *, *, #9220, .F. ) ;
#33812 = AXIS2_PLACEMENT_3D ( 'NONE', #27797, #41710, #10475 ) ;
#33813 = CARTESIAN_POINT ( 'NONE',  ( 121.8725281442453223, -6.222761293078241884, -8.102969835052219238 ) ) ;
#33814 = CARTESIAN_POINT ( 'NONE',  ( 117.5613014775786525, 0.9020085738987339008, -11.91225656197089222 ) ) ;
#33815 = CARTESIAN_POINT ( 'NONE',  ( 125.2194014775786286, -10.30919188438810075, -12.61870101168855918 ) ) ;
#33816 = CARTESIAN_POINT ( 'NONE',  ( 124.9357681442453014, -7.643976991954077427, -18.09477374809248928 ) ) ;
#33817 = ORIENTED_EDGE ( 'NONE', *, *, #6423, .T. ) ;
#33818 = DIRECTION ( 'NONE',  ( -0.9609149988134837450, 0.1028163501681639419, -0.2570431154366518145 ) ) ;
#33819 = CARTESIAN_POINT ( 'NONE',  ( 124.9924948109119924, -4.089484607189486809, -7.948022111789456723 ) ) ;
#33820 = EDGE_CURVE ( 'NONE', #26936, #11048, #25384, .T. ) ;
#33821 = CARTESIAN_POINT ( 'NONE',  ( 115.9162281442453235, -5.574606645277164318, -18.38911715685844683 ) ) ;
#33822 =( BOUNDED_CURVE ( )  B_SPLINE_CURVE ( 2, ( #18688, #4990, #33015, #15715, #40107, #29617, #26651, #18902, #9326, #33245, #43986, #43532, #39884, #8647, #30075, #32577, #25754 ),
 .UNSPECIFIED., .F., .F. ) 
 B_SPLINE_CURVE_WITH_KNOTS ( ( 3, 2, 2, 2, 2, 2, 2, 2, 3 ),
 ( 0.8295046674808920217, 0.8359375000000000000, 0.8437500000000000000, 0.8515625000000000000, 0.8593750000000000000, 0.8671875000000000000, 0.8750000000000000000, 0.8828125000000000000, 0.8892453325190590174 ),
 .UNSPECIFIED. ) 
 CURVE ( )  GEOMETRIC_REPRESENTATION_ITEM ( )  RATIONAL_B_SPLINE_CURVE ( ( 0.9778625265006459788, 0.9373222120152210346, 1.000000000000000000, 0.9238795325112869605, 1.000000000000000000, 0.9238795325112869605, 1.000000000000000000, 0.9238795325112869605, 1.000000000000000000, 0.9238795325112869605, 1.000000000000000000, 0.9238795325112869605, 1.000000000000000000, 0.9238795325112869605, 1.000000000000000000, 0.9373222120156999848, 0.9778625265000260303 ) ) 
 REPRESENTATION_ITEM ( '' )  );
#33823 = CARTESIAN_POINT ( 'NONE',  ( 123.9146881442452894, 0.9020085738987339008, -11.91225656197089222 ) ) ;
#33824 = CARTESIAN_POINT ( 'NONE',  ( 70.19189222814998175, -61.33395589173652951, -37.73637771078367109 ) ) ;
#33825 = CARTESIAN_POINT ( 'NONE',  ( 121.7575954359119805, 0.5291689781388270175, -13.89700978578772705 ) ) ;
#33826 = ORIENTED_EDGE ( 'NONE', *, *, #24355, .F. ) ;
#33827 = CARTESIAN_POINT ( 'NONE',  ( 59.95220766929363521, -14.75932518950456185, -7.413731407758326952 ) ) ;
#33828 = B_SPLINE_CURVE_WITH_KNOTS ( 'NONE', 3,
 ( #11194, #3884, #249, #31698, #916, #39453, #7763, #28294, #31476, #17805 ),
 .UNSPECIFIED., .F., .F.,
 ( 4, 3, 3, 4 ),
 ( 0.000000000000000000, 0.0001671877560958099957, 0.0003343755126086554838, 0.0006438490228505469159 ),
 .UNSPECIFIED. ) ;
#33829 = COLOUR_RGB ( '',0.7921568627450980005, 0.8196078431372548767, 0.9333333333333333481 ) ;
#33830 = CARTESIAN_POINT ( 'NONE',  ( 109.1629577545248395, -2.791137627527939813, -18.39754474579286025 ) ) ;
#33831 = CARTESIAN_POINT ( 'NONE',  ( 117.8632207241439289, -2.443475742715334853, -17.86549347949429389 ) ) ;
#33832 = CARTESIAN_POINT ( 'NONE',  ( 117.6747548109119919, -7.643976991954077427, -18.09477374809248928 ) ) ;
#33833 = CARTESIAN_POINT ( 'NONE',  ( 115.8027748109119841, -8.899110576539710493, -16.42337572283490132 ) ) ;
#33834 = CARTESIAN_POINT ( 'NONE',  ( 127.0066334552966651, -0.006442243401518138457, -11.04793111752537094 ) ) ;
#33835 = ORIENTED_EDGE ( 'NONE', *, *, #5573, .T. ) ;
#33836 = LINE ( 'NONE', #34293, #29490 ) ;
#33837 = CARTESIAN_POINT ( 'NONE',  ( 118.9227414775786542, 0.4262465694468514643, -12.03445270309931736 ) ) ;
#33838 = AXIS2_PLACEMENT_3D ( 'NONE', #39570, #4455, #17696 ) ;
#33839 = CARTESIAN_POINT ( 'NONE',  ( 113.3635281442453504, -0.1624402480850797581, -16.17319339645315424 ) ) ;
#33840 = FACE_OUTER_BOUND ( 'NONE', #177, .T. ) ;
#33841 = CARTESIAN_POINT ( 'NONE',  ( -2.517858533981217395, -7.040069435492971373, -19.27574816075459552 ) ) ;
#33843 = CARTESIAN_POINT ( 'NONE',  ( 122.6099748109119929, -9.261995988541697145, -16.69588392320189030 ) ) ;
#33842 = PLANE ( 'NONE',  #1772 ) ;
#33844 = CARTESIAN_POINT ( 'NONE',  ( 125.9001214775786224, -5.574606645277164318, -18.38911715685844683 ) ) ;
#33845 = ORIENTED_EDGE ( 'NONE', *, *, #7441, .F. ) ;
#33846 = DIRECTION ( 'NONE',  ( 0.000000000000000000, 0.000000000000000000, 1.000000000000000000 ) ) ;
#33847 = CARTESIAN_POINT ( 'NONE',  ( 113.3277860444392076, -1.267766418764742165, -16.93314635290707315 ) ) ;
#33848 = CARTESIAN_POINT ( 'NONE',  ( 115.6220983795247861, -0.7896495226426338832, -9.318865927141430916 ) ) ;
#33849 = CARTESIAN_POINT ( 'NONE',  ( 111.8319081442453182, -5.638512984488999180, -18.83840828888717311 ) ) ;
#33850 = CARTESIAN_POINT ( 'NONE',  ( 119.7736414775786358, 0.1319031606808879209, -14.10382304977623669 ) ) ;
#33851 = CARTESIAN_POINT ( 'NONE',  ( 112.2188952545247531, -9.868328341294102302, -15.46607636865001645 ) ) ;
#33852 = CARTESIAN_POINT ( 'NONE',  ( 115.1359265045248605, -2.791137627527939813, -8.388885654883777576 ) ) ;
#33853 = DIRECTION ( 'NONE',  ( -0.6836572958096076569, 0.7298031939408696767, 0.000000000000000000 ) ) ;
#33854 = DIRECTION ( 'NONE',  ( -0.8949343913984424415, -0.4123869368673878655, -0.1703803081152052423 ) ) ;
#33855 = CARTESIAN_POINT ( 'NONE',  ( 112.8529881442453302, -7.894159318335828068, -9.358103419637847864 ) ) ;
#33856 = CARTESIAN_POINT ( 'NONE',  ( 111.2465515045248168, -2.477300249445798297, -7.631215200338321125 ) ) ;
#33857 = CARTESIAN_POINT ( 'NONE',  ( 117.4585358072985315, 0.3208234527006367798, -15.99825685930877839 ) ) ;
#33858 = CARTESIAN_POINT ( 'NONE',  ( 112.2188952545247531, 0.8980012041604421569, -11.00651665394454071 ) ) ;
#33859 = CARTESIAN_POINT ( 'NONE',  ( 125.5597614775786326, -1.561330072975669392, -17.79121239304076951 ) ) ;
#33860 = CARTESIAN_POINT ( 'NONE',  ( 122.8936081442453059, 0.2603800115204892296, -16.42320221600525088 ) ) ;
#33861 = CARTESIAN_POINT ( 'NONE',  ( 114.8581140045248361, -10.62599879583958540, -11.00651665394454604 ) ) ;
#33862 = CARTESIAN_POINT ( 'NONE',  ( 121.2485348109119769, -0.4660016031367893996, -10.09054647747474043 ) ) ;
#33863 = CARTESIAN_POINT ( 'NONE',  ( 112.5126281442453120, -10.30919188438810075, -12.61870101168855918 ) ) ;
#33864 = ORIENTED_EDGE ( 'NONE', *, *, #15526, .F. ) ;
#33865 = CARTESIAN_POINT ( 'NONE',  ( 114.5547881442453217, -4.153390946401321671, -8.397313243818183892 ) ) ;
#33866 = AXIS2_PLACEMENT_3D ( 'NONE', #19372, #5006, #12317 ) ;
#33867 = CARTESIAN_POINT ( 'NONE',  ( 111.4348214775786801, -3.505236298600246325, -18.68346056562440793 ) ) ;
#33868 = CARTESIAN_POINT ( 'NONE',  ( 124.7088614775786226, 0.2603800115204892296, -16.42320221600525088 ) ) ;
#33869 = CARTESIAN_POINT ( 'NONE',  ( 115.6325948109119821, 0.2603800115204892296, -16.42320221600525088 ) ) ;
#33870 = CARTESIAN_POINT ( 'NONE',  ( 113.0798948109119948, -8.899110576539710493, -16.42337572283490132 ) ) ;
#33871 = ORIENTED_EDGE ( 'NONE', *, *, #1919, .F. ) ;
#33872 = CARTESIAN_POINT ( 'NONE',  ( 116.3133148109120043, -2.084020599724406786, -8.691656652584148546 ) ) ;
#33873 = CIRCLE ( 'NONE', #20777, 2.999999999999999556 ) ;
#33874 = FACE_OUTER_BOUND ( 'NONE', #28777, .T. ) ;
#33875 = CARTESIAN_POINT ( 'NONE',  ( 111.6632702545248605, 0.1403307496149616695, -11.32035403202665336 ) ) ;
#33876 = CARTESIAN_POINT ( 'NONE',  ( 123.3474214775786209, -0.1624402480850797581, -16.17319339645315424 ) ) ;
#33877 = CARTESIAN_POINT ( 'NONE',  ( 116.8415777867357406, -0.9725888463086822533, -16.91308624977476072 ) ) ;
#33878 = CARTESIAN_POINT ( 'NONE',  ( 116.5944421295247793, 0.8980012041604618078, -13.39321520033831447 ) ) ;
#33879 = ORIENTED_EDGE ( 'NONE', *, *, #20073, .F. ) ;
#33880 = CARTESIAN_POINT ( 'NONE',  ( 122.2437673109119629, -9.289237151508434209, -11.05642687123711276 ) ) ;
#33881 = CARTESIAN_POINT ( 'NONE',  ( 125.6164881442453094, 0.2603800115204892296, -16.42320221600525088 ) ) ;
#33882 = CARTESIAN_POINT ( 'NONE',  ( 66.58723489636778936, -20.14619392353143112, -15.89321520033831447 ) ) ;
#33883 = CARTESIAN_POINT ( 'NONE',  ( 112.5126281442453120, -10.30919188438810075, -12.61870101168855918 ) ) ;
#33884 = CARTESIAN_POINT ( 'NONE',  ( 117.0283149730835959, 1.730878968199667245, -5.544651811887305826 ) ) ;
#33885 = CARTESIAN_POINT ( 'NONE',  ( 114.1406031537514849, 0.4930828106259610433, -14.64321520033831447 ) ) ;
#33886 = CARTESIAN_POINT ( 'NONE',  ( 105.6903015045248253, -6.936859964151250502, -18.39754474579286025 ) ) ;
#33887 = EDGE_CURVE ( 'NONE', #10182, #2987, #42933, .T. ) ;
#33888 = DIRECTION ( 'NONE',  ( -1.000000000000000000, 0.000000000000000000, 0.000000000000000000 ) ) ;
#33889 = CARTESIAN_POINT ( 'NONE',  ( 137.4419881480160370, -6.036542153170629810, -18.33154758575252430 ) ) ;
#33890 = CIRCLE ( 'NONE', #9873, 0.9999999999999952260 ) ;
#33891 = DIRECTION ( 'NONE',  ( 0.000000000000000000, 0.6004852223388321697, -0.7996358532186279566 ) ) ;
#33892 = CARTESIAN_POINT ( 'NONE',  ( 124.9357681442453014, -1.834011780172310813, -8.268836392978581529 ) ) ;
#33893 = CARTESIAN_POINT ( 'NONE',  ( 122.3263414775786373, -3.505236298600246325, -18.68346056562440793 ) ) ;
#33894 = CARTESIAN_POINT ( 'NONE',  ( 119.7434548109119845, -3.753605393790139466, -18.88744880365131351 ) ) ;
#33895 = ORIENTED_EDGE ( 'NONE', *, *, #40728, .T. ) ;
#33896 = CARTESIAN_POINT ( 'NONE',  ( 123.5176014775786228, -9.261995988541697145, -16.69588392320189030 ) ) ;
#33897 = CARTESIAN_POINT ( 'NONE',  ( 120.8514481442452961, -7.893985811506177619, -18.51759400769804742 ) ) ;
#33898 = CARTESIAN_POINT ( 'NONE',  ( 126.1270281442452870, -10.30919188438810075, -12.61870101168855918 ) ) ;
#33899 = CARTESIAN_POINT ( 'NONE',  ( 113.4769814775786614, -10.63000616557722466, -14.87417383870573495 ) ) ;
#33900 = CARTESIAN_POINT ( 'NONE',  ( 126.5241148109119393, -9.565557343593413364, -10.61323700422348004 ) ) ;
#33901 = CARTESIAN_POINT ( 'NONE',  ( 125.0492214775786266, -6.344957434206665248, -7.627207830600338134 ) ) ;
#33902 = CARTESIAN_POINT ( 'NONE',  ( 111.8716296295247901, -4.863998795839590272, -19.15521520033831493 ) ) ;
#33903 = DIRECTION ( 'NONE',  ( -1.224775218828351862E-16, 0.3818493186865896671, -0.9242245927363043068 ) ) ;
#33904 = CARTESIAN_POINT ( 'NONE',  ( 83.11819775781678743, -31.88128537155179743, -23.36558840204159537 ) ) ;
#33905 = CARTESIAN_POINT ( 'NONE',  ( 115.5191414775786569, -6.222761293078241884, -8.102969835052219238 ) ) ;
#33906 = CARTESIAN_POINT ( 'NONE',  ( 118.2420214775786320, -6.222761293078241884, -8.102969835052219238 ) ) ;
#33907 = CARTESIAN_POINT ( 'NONE',  ( 112.8439888068194819, 0.1168444861213632779, -12.14321520033831625 ) ) ;
#33908 = CARTESIAN_POINT ( 'NONE',  ( 115.6915515045247531, -6.936859964151250502, -18.39754474579286025 ) ) ;
#33909 = ORIENTED_EDGE ( 'NONE', *, *, #8308, .F. ) ;
#33910 = CARTESIAN_POINT ( 'NONE',  ( 94.20708369096698220, -24.88943055980569241, -13.49371108670732333 ) ) ;
#33911 = CARTESIAN_POINT ( 'NONE',  ( 113.7606148109119886, -1.561330072975668060, -17.79121239304076596 ) ) ;
#33912 = CARTESIAN_POINT ( 'NONE',  ( 90.33554924625337890, -25.99489077589524300, -13.39321520033831447 ) ) ;
#33913 = CARTESIAN_POINT ( 'NONE',  ( 122.7299391859119737, -8.844754642576884152, -8.592115655440050404 ) ) ;
#33914 = CARTESIAN_POINT ( 'NONE',  ( 121.9659548109119811, -2.527210466738041728, -8.967976844669124148 ) ) ;
#33915 = ORIENTED_EDGE ( 'NONE', *, *, #15579, .T. ) ;
#33916 = CARTESIAN_POINT ( 'NONE',  ( 123.3152181068994651, -2.449738653808077427, -15.35887260493897344 ) ) ;
#33917 = CARTESIAN_POINT ( 'NONE',  ( 116.5799884964095270, -11.88873078449987375, -21.18799803434260554 ) ) ;
#33918 = EDGE_CURVE ( 'NONE', #43250, #34606, #6028, .T. ) ;
#33919 = VERTEX_POINT ( 'NONE', #7362 ) ;
#33920 = CARTESIAN_POINT ( 'NONE',  ( 117.7882081442453170, -6.344957434206665248, -7.627207830600338134 ) ) ;
#33921 = CARTESIAN_POINT ( 'NONE',  ( 122.6667014775786413, -2.084020599724406786, -8.691656652584148546 ) ) ;
#33922 = CARTESIAN_POINT ( 'NONE',  ( 119.4900081442453086, -7.643976991954077427, -18.09477374809248928 ) ) ;
#33923 = B_SPLINE_CURVE_WITH_KNOTS ( 'NONE', 3,
 ( #37024, #40699, #44351, #34507, #41391, #10589, #11033, #14225, #17645, #17869 ),
 .UNSPECIFIED., .F., .F.,
 ( 4, 2, 2, 2, 4 ),
 ( 0.000000000000000000, 0.2500000000000000000, 0.5000000000000000000, 0.7500000000000000000, 1.000000000000000000 ),
 .UNSPECIFIED. ) ;
#33924 = CARTESIAN_POINT ( 'NONE',  ( 120.2515881224973100, -8.245590802997449842, -17.07726823302562025 ) ) ;
#33925 = CARTESIAN_POINT ( 'NONE',  ( 120.9649014775786355, -3.383040157471821630, -19.15922257007629170 ) ) ;
#33926 = EDGE_CURVE ( 'NONE', #20193, #44110, #32362, .T. ) ;
#33927 = CARTESIAN_POINT ( 'NONE',  ( 119.5467348109119712, -4.089484607189486809, -7.948022111789456723 ) ) ;
#33928 = ADVANCED_FACE ( 'NONE', ( #7437 ), #27991, .T. ) ;
#33929 = CARTESIAN_POINT ( 'NONE',  ( 110.1353015045248469, -6.936859964151250502, -18.39754474579286025 ) ) ;
#33930 = CARTESIAN_POINT ( 'NONE',  ( 111.6617281442453304, 0.4262465694468514643, -12.03445270309931736 ) ) ;
#33931 = B_SPLINE_CURVE_WITH_KNOTS ( 'NONE', 3,
 ( #1930, #15627, #15857, #19042, #36131, #2146, #12212, #33154, #22461, #39347 ),
 .UNSPECIFIED., .F., .F.,
 ( 4, 3, 3, 4 ),
 ( 0.000000000000000000, 0.0001671877548681235048, 0.0003343755096277620112, 0.0006463528481650609656 ),
 .UNSPECIFIED. ) ;
#33932 = CARTESIAN_POINT ( 'NONE',  ( 86.51169734173754478, -25.99489077589583630, -8.393215200338314474 ) ) ;
#33933 = ORIENTED_EDGE ( 'NONE', *, *, #31970, .F. ) ;
#33934 = CARTESIAN_POINT ( 'NONE',  ( 116.1998614775786507, -10.63000616557722466, -14.87417383870573495 ) ) ;
#33935 = CARTESIAN_POINT ( 'NONE',  ( 113.2500748109119968, -3.505236298600246325, -18.68346056562440793 ) ) ;
#33936 = VECTOR ( 'NONE', #27912, 1000.000000000000227 ) ;
#33937 = CARTESIAN_POINT ( 'NONE',  ( 75.95778847736514194, -3.256761025687008537, -16.39321520033831447 ) ) ;
#33938 = CARTESIAN_POINT ( 'NONE',  ( 113.8740681442453138, 0.5811942927096154232, -14.16772938898807155 ) ) ;
#33939 = VERTEX_POINT ( 'NONE', #21132 ) ;
#33940 = CARTESIAN_POINT ( 'NONE',  ( 120.7947214775786193, -9.261995988541697145, -16.69588392320189030 ) ) ;
#33941 = DIRECTION ( 'NONE',  ( 0.000000000000000000, -0.9242245927363034186, -0.3818493186865916655 ) ) ;
#33942 = CARTESIAN_POINT ( 'NONE',  ( 113.5337081442453240, -0.8288870151387760510, -10.36305467784173118 ) ) ;
#33943 = ADVANCED_FACE ( 'NONE', ( #11103 ), #17986, .F. ) ;
#33944 = CARTESIAN_POINT ( 'NONE',  ( 121.9470836909669913, -24.14644159042263993, -12.62951656296512937 ) ) ;
#33945 = CARTESIAN_POINT ( 'NONE',  ( 151.2860562277021472, -4.863998795839242995, -13.39321520033831447 ) ) ;
#33946 = CARTESIAN_POINT ( 'NONE',  ( 117.5613014775786525, -10.15424416112533912, -14.75197769757731336 ) ) ;
#33947 = ADVANCED_FACE ( 'NONE', ( #10881 ), #10659, .T. ) ;
#33948 = EDGE_CURVE ( 'NONE', #7036, #35580, #37011, .T. ) ;
#33949 = CARTESIAN_POINT ( 'NONE',  ( 123.6834074775628380, -4.587599304697977054, -15.01040869781757081 ) ) ;
#33950 = CARTESIAN_POINT ( 'NONE',  ( 116.7104014775786425, -8.899110576539710493, -16.42337572283490132 ) ) ;
#33951 = CARTESIAN_POINT ( 'NONE',  ( 73.60369002873177635, -5.846784287000932778, -9.893215200338316251 ) ) ;
#33952 = VECTOR ( 'NONE', #10557, 1000.000000000000000 ) ;
#33953 = CARTESIAN_POINT ( 'NONE',  ( 114.3278814775786429, 0.1319031606808879209, -14.10382304977623669 ) ) ;
#33954 = CARTESIAN_POINT ( 'NONE',  ( 115.4056881442453459, -7.893985811506177619, -18.51759400769804742 ) ) ;
#33955 = CARTESIAN_POINT ( 'NONE',  ( 124.6051735609119646, -9.645473719204776586, -14.86997237629376656 ) ) ;
#33956 = CARTESIAN_POINT ( 'NONE',  ( 113.0231681442453322, 0.9020085738987339008, -11.91225656197089222 ) ) ;
#33957 = CARTESIAN_POINT ( 'NONE',  ( 116.8805814775786445, -3.505236298600246325, -18.68346056562440793 ) ) ;
#33958 = CARTESIAN_POINT ( 'NONE',  ( 122.6667014775786413, -7.893985811506177619, -18.51759400769804742 ) ) ;
#33959 = CARTESIAN_POINT ( 'NONE',  ( 116.8805814775786445, -3.505236298600246325, -18.68346056562440793 ) ) ;
#33960 = ORIENTED_EDGE ( 'NONE', *, *, #37536, .F. ) ;
#33961 = CARTESIAN_POINT ( 'NONE',  ( 113.1366214775786432, -1.834011780172310813, -8.268836392978581529 ) ) ;
#33962 = CARTESIAN_POINT ( 'NONE',  ( 111.1076452545248259, 0.8980012041604421569, -11.00651665394454071 ) ) ;
#33963 = VECTOR ( 'NONE', #6547, 1000.000000000000000 ) ;
#33964 = CARTESIAN_POINT ( 'NONE',  ( 105.3430358795248338, -8.402594152722688392, -9.854619843455216355 ) ) ;
#33965 = CARTESIAN_POINT ( 'NONE',  ( 106.3153796295248412, -4.863998795839590272, -8.388885654883775800 ) ) ;
#33966 = DIRECTION ( 'NONE',  ( 0.9609149988134843001, -0.1028163501681632064, 0.2570431154366505933 ) ) ;
#33967 = CARTESIAN_POINT ( 'NONE',  ( 120.4543614775786295, -4.089484607189486809, -7.948022111789456723 ) ) ;
#33968 = VERTEX_POINT ( 'NONE', #24778 ) ;
#33969 = CARTESIAN_POINT ( 'NONE',  ( 124.5954081442453116, -3.383040157471821630, -19.15922257007629170 ) ) ;
#33970 = DIRECTION ( 'NONE',  ( -0.7871354856660162103, -0.4483307682966942709, -0.4235767337848251879 ) ) ;
#33971 = CARTESIAN_POINT ( 'NONE',  ( 114.5547881442453217, -4.153390946401321671, -8.397313243818183892 ) ) ;
#33972 = DIRECTION ( 'NONE',  ( 0.000000000000000000, -0.9242245927363028635, -0.3818493186865927758 ) ) ;
#33973 = VECTOR ( 'NONE', #6138, 1000.000000000000000 ) ;
#33974 = CARTESIAN_POINT ( 'NONE',  ( 123.8579614775786126, 0.5811942927096110934, -14.16772938898807510 ) ) ;
#33975 = CARTESIAN_POINT ( 'NONE',  ( 114.3719421295247827, -9.868328341294093420, -13.39321520033831447 ) ) ;
#33976 = CARTESIAN_POINT ( 'NONE',  ( 89.28011985346235235, -9.943418426816830191, -13.56419841707012708 ) ) ;
#33977 = ORIENTED_EDGE ( 'NONE', *, *, #42030, .T. ) ;
#33978 = FACE_OUTER_BOUND ( 'NONE', #3648, .T. ) ;
#33979 = CARTESIAN_POINT ( 'NONE',  ( 124.0281414775786146, -7.643976991954077427, -18.09477374809248928 ) ) ;
#33980 = CARTESIAN_POINT ( 'NONE',  ( 118.1285681442453068, -7.893985811506177619, -18.51759400769804742 ) ) ;
#33981 = DIRECTION ( 'NONE',  ( -0.2768435750659241079, -0.3568721902840695792, 0.8921882507333129819 ) ) ;
#33982 = CARTESIAN_POINT ( 'NONE',  ( 116.7671281442453335, -1.834011780172310813, -8.268836392978581529 ) ) ;
#33983 = DIRECTION ( 'NONE',  ( -0.9908103287288503314, 0.1352586133457956419, 0.000000000000000000 ) ) ;
#33984 = CARTESIAN_POINT ( 'NONE',  ( 125.5030348109119558, -6.222761293078241884, -8.102969835052219238 ) ) ;
#33985 = CARTESIAN_POINT ( 'NONE',  ( 119.6601881442453106, -1.833838273342659253, -17.42832698103878286 ) ) ;
#33986 = ORIENTED_EDGE ( 'NONE', *, *, #20300, .T. ) ;
#33987 = EDGE_CURVE ( 'NONE', #29206, #38146, #7055, .T. ) ;
#33988 = CARTESIAN_POINT ( 'NONE',  ( 120.0005481442453146, -5.638512984489026714, -18.83840828888716956 ) ) ;
#33989 = CIRCLE ( 'NONE', #27443, 5.999999999999997335 ) ;
#33990 = CARTESIAN_POINT ( 'NONE',  ( 113.4202548109119846, -10.30919188438810075, -12.61870101168855918 ) ) ;
#33991 = CARTESIAN_POINT ( 'NONE',  ( 121.1918081442452859, -10.15424416112533912, -14.75197769757731336 ) ) ;
#33992 = VERTEX_POINT ( 'NONE', #7220 ) ;
#33993 = CARTESIAN_POINT ( 'NONE',  ( 121.8965016859119856, -0.6942167230862511529, -9.935906262978006609 ) ) ;
#33994 = CARTESIAN_POINT ( 'NONE',  ( 136.7478768735744552, -1.263210933052332230, -9.073952808020385064 ) ) ;
#33995 = CARTESIAN_POINT ( 'NONE',  ( 119.4332814775786318, -0.4660016031367893996, -10.09054647747474043 ) ) ;
#33996 = CARTESIAN_POINT ( 'NONE',  ( 110.6214733795247867, -8.938348069036489818, -17.46756447353520159 ) ) ;
#33997 = CARTESIAN_POINT ( 'NONE',  ( 115.5191414775786569, -6.222761293078241884, -8.102969835052219238 ) ) ;
#33998 = VECTOR ( 'NONE', #16556, 1000.000000000000114 ) ;
#33999 = ORIENTED_EDGE ( 'NONE', *, *, #5527, .T. ) ;
#34000 = ORIENTED_EDGE ( 'NONE', *, *, #9401, .T. ) ;
#34001 = CARTESIAN_POINT ( 'NONE',  ( 125.1626748109119802, -0.1624402480850797581, -16.17319339645315424 ) ) ;
#34002 = CARTESIAN_POINT ( 'NONE',  ( 122.4965214775786251, 0.1319031606808879209, -14.10382304977623669 ) ) ;
#34003 = FACE_OUTER_BOUND ( 'NONE', #41206, .T. ) ;
#34004 = EDGE_CURVE ( 'NONE', #34659, #42684, #40479, .T. ) ;
#34005 = VERTEX_POINT ( 'NONE', #11326 ) ;
#34006 = CARTESIAN_POINT ( 'NONE',  ( 122.3830681442452857, -8.166667518702819706, -8.995218007635861213 ) ) ;
#34007 = DIRECTION ( 'NONE',  ( -1.000000000000000000, 0.000000000000000000, -0.000000000000000000 ) ) ;
#34008 = CARTESIAN_POINT ( 'NONE',  ( 120.6812681442452941, -10.30919188438810075, -12.61870101168855918 ) ) ;
#34010 = CARTESIAN_POINT ( 'NONE',  ( 119.8303681442453126, 0.4262465694468514643, -12.03445270309931736 ) ) ;
#34009 = CARTESIAN_POINT ( 'NONE',  ( 117.6180281442453150, -0.4660016031367893996, -10.09054647747474043 ) ) ;
#34011 = EDGE_CURVE ( 'NONE', #17200, #40452, #9068, .T. ) ;
#34012 =( BOUNDED_SURFACE ( )  B_SPLINE_SURFACE ( 1, 2, ( 
 ( #44645, #38009, #6783, #20693, #34571, #24338, #31380, #32497, #34999, #1045, #7212, #376, #28650, #11318, #25228, #18156, #24997, #17707, #31831, #3783, #11096, #42114, #42335, #31607, #10650, #4685, #8124, #14512, #22026, #10874, #24556, #35919, #7429, #38442, #35693, #4469, #39126, #14287, #21125, #28206, #24769, #38660, #38892, #39356, #42556, #819, #14961, #21350, #35234, #4010, #7893, #25454, #28424, #7661, #17932, #21799, #18389, #601, #32277, #28873, #14738, #29087, #42786, #11547, #21576, #1272, #35463, #4238, #32052, #18606, #15184, #19506, #16086, #16318, #19285, #40026, #42999, #1940, #2157, #33385, #1713, #29991, #43908, #12677, #2390, #5809, #26575, #40489, #12221, #33164, #11767, #29315, #26120, #8790, #15866, #15411, #43228, #25897, #15637, #36814, #9248, #23157, #25676, #29762, #37039, #11995, #19727, #22696, #32938, #33613, #36593, #32717, #43674, #26350, #39582, #8344, #5368, #12449, #40258, #22245, #36141, #39801, #5136, #4909, #9024, #22922, #5582, #29541, #43457, #18825, #1489, #8570, #22470, #36364, #19052, #10159, #23616, #45036, #23847, #40712, #37958, #34080, #37267, #2847, #26802, #9702, #24287, #9472, #20643, #27708, #41622, #40946, #3298, #41174, #16777, #12906, #30221, #10378, #34735, #23383, #37502 ),
 ( #13796, #17005, #20420, #34520, #6037, #19959, #16549, #30894, #38173, #30671, #44592, #6276, #41403, #6733, #33848, #13574, #3076, #34303, #3518, #24067, #31111, #20196, #20857, #13355, #30445, #44364, #6952, #44141, #17221, #2617, #13126, #6505, #27259, #27031, #44816, #9934, #37734, #27484, #21749, #39074, #7843, #21973, #25402, #35640, #996, #31777, #38840, #35860, #3735, #548, #14460, #7609, #34949, #17658, #322, #35181, #11268, #32223, #14911, #31329, #21523, #28822, #31554, #42732, #28367, #7381, #11497, #42280, #7160, #35410, #761, #103, #4416, #11042, #4185, #24944, #39300, #17436, #14235, #24716, #24503, #18103, #31998, #14683, #21298, #17880, #18330, #14016, #28597, #42508, #21072, #10600, #8070, #41840, #27931, #38387, #28151, #42061, #10819, #25176, #38605, #3958, #39973, #40203, #11716, #25627, #36091, #5314, #19449, #22420, #8517, #15360, #15808, #12396, #39532, #33111, #22644, #8736, #23102, #29709, #5530, #11945, #40434, #39749, #4862, #18780, #29942, #43855, #26296, #22868, #4634, #26069, #1660, #18555, #36540, #8969, #36761, #36313, #33332, #2106, #16034, #9195, #12627, #26525, #32447, #18999, #19230, #1221, #32670, #32886, #15582, #1881, #22195, #1438, #29265, #5083, #43622, #15135, #29041, #42950, #8293 ) ),
 .UNSPECIFIED., .F., .F., .T. ) 
 B_SPLINE_SURFACE_WITH_KNOTS ( ( 2, 2 ),
 ( 3, 2, 2, 2, 2, 2, 2, 2, 2, 2, 2, 2, 2, 2, 2, 2, 2, 2, 2, 2, 2, 2, 2, 2, 2, 2, 2, 2, 2, 2, 2, 2, 2, 2, 2, 2, 2, 2, 2, 2, 2, 2, 2, 2, 2, 2, 2, 2, 2, 2, 2, 2, 2, 2, 2, 2, 2, 2, 2, 2, 2, 2, 2, 2, 2, 2, 2, 2, 2, 2, 2, 2, 2, 2, 2, 2, 2, 2, 2, 2, 3 ),
 ( 0.000000000000000000, 1.000000000000000000 ),
 ( 0.000000000000000000, 0.01250000000000000069, 0.02500000000000000139, 0.03749999999999999861, 0.05000000000000000278, 0.06250000000000000000, 0.07499999999999999722, 0.08749999999999999445, 0.1000000000000000056, 0.1125000000000000028, 0.1250000000000000000, 0.1375000000000000111, 0.1499999999999999944, 0.1625000000000000056, 0.1749999999999999889, 0.1875000000000000000, 0.2000000000000000111, 0.2124999999999999944, 0.2250000000000000056, 0.2374999999999999889, 0.2500000000000000000, 0.2625000000000000111, 0.2750000000000000222, 0.2874999999999999778, 0.2999999999999999889, 0.3125000000000000000, 0.3250000000000000111, 0.3375000000000000222, 0.3499999999999999778, 0.3624999999999999889, 0.3750000000000000000, 0.3875000000000000111, 0.4000000000000000222, 0.4124999999999999778, 0.4249999999999999889, 0.4375000000000000000, 0.4500000000000000111, 0.4625000000000000222, 0.4749999999999999778, 0.4874999999999999889, 0.5000000000000000000, 0.5124999999999999556, 0.5250000000000000222, 0.5374999999999999778, 0.5500000000000000444, 0.5625000000000000000, 0.5749999999999999556, 0.5875000000000000222, 0.5999999999999999778, 0.6125000000000000444, 0.6250000000000000000, 0.6374999999999999556, 0.6500000000000000222, 0.6624999999999999778, 0.6750000000000000444, 0.6875000000000000000, 0.6999999999999999556, 0.7125000000000000222, 0.7249999999999999778, 0.7375000000000000444, 0.7500000000000000000, 0.7624999999999999556, 0.7750000000000000222, 0.7874999999999999778, 0.8000000000000000444, 0.8125000000000000000, 0.8249999999999999556, 0.8375000000000000222, 0.8499999999999999778, 0.8625000000000000444, 0.8750000000000000000, 0.8874999999999999556, 0.9000000000000000222, 0.9124999999999999778, 0.9250000000000000444, 0.9375000000000000000, 0.9499999999999999556, 0.9625000000000000222, 0.9749999999999999778, 0.9875000000000000444, 1.000000000000000000 ),
 .UNSPECIFIED. ) 
 GEOMETRIC_REPRESENTATION_ITEM ( )  RATIONAL_B_SPLINE_SURFACE ( (
 ( 1.000000000000000000, 0.9238795325112869605, 1.000000000000000000, 0.9238795325112869605, 1.000000000000000000, 0.9238795325112869605, 1.000000000000000000, 0.9238795325112869605, 1.000000000000000000, 0.9238795325112869605, 1.000000000000000000, 0.9238795325112869605, 1.000000000000000000, 0.9238795325112869605, 1.000000000000000000, 0.9238795325112869605, 1.000000000000000000, 0.9238795325112869605, 1.000000000000000000, 0.9238795325112869605, 1.000000000000000000, 0.9238795325112869605, 1.000000000000000000, 0.9238795325112869605, 1.000000000000000000, 0.9238795325112869605, 1.000000000000000000, 0.9238795325112869605, 1.000000000000000000, 0.9238795325112869605, 1.000000000000000000, 0.9238795325112869605, 1.000000000000000000, 0.9238795325112869605, 1.000000000000000000, 0.9238795325112869605, 1.000000000000000000, 0.9238795325112869605, 1.000000000000000000, 0.9238795325112869605, 1.000000000000000000, 0.9238795325112869605, 1.000000000000000000, 0.9238795325112869605, 1.000000000000000000, 0.9238795325112869605, 1.000000000000000000, 0.9238795325112869605, 1.000000000000000000, 0.9238795325112869605, 1.000000000000000000, 0.9238795325112869605, 1.000000000000000000, 0.9238795325112869605, 1.000000000000000000, 0.9238795325112869605, 1.000000000000000000, 0.9238795325112869605, 1.000000000000000000, 0.9238795325112869605, 1.000000000000000000, 0.9238795325112869605, 1.000000000000000000, 0.9238795325112869605, 1.000000000000000000, 0.9238795325112869605, 1.000000000000000000, 0.9238795325112869605, 1.000000000000000000, 0.9238795325112869605, 1.000000000000000000, 0.9238795325112869605, 1.000000000000000000, 0.9238795325112869605, 1.000000000000000000, 0.9238795325112869605, 1.000000000000000000, 0.9238795325112869605, 1.000000000000000000, 0.9238795325112869605, 1.000000000000000000, 0.9238795325112869605, 1.000000000000000000, 0.9238795325112869605, 1.000000000000000000, 0.9238795325112869605, 1.000000000000000000, 0.9238795325112869605, 1.000000000000000000, 0.9238795325112869605, 1.000000000000000000, 0.9238795325112869605, 1.000000000000000000, 0.9238795325112869605, 1.000000000000000000, 0.9238795325112869605, 1.000000000000000000, 0.9238795325112869605, 1.000000000000000000, 0.9238795325112869605, 1.000000000000000000, 0.9238795325112869605, 1.000000000000000000, 0.9238795325112869605, 1.000000000000000000, 0.9238795325112869605, 1.000000000000000000, 0.9238795325112869605, 1.000000000000000000, 0.9238795325112869605, 1.000000000000000000, 0.9238795325112869605, 1.000000000000000000, 0.9238795325112869605, 1.000000000000000000, 0.9238795325112869605, 1.000000000000000000, 0.9238795325112869605, 1.000000000000000000, 0.9238795325112869605, 1.000000000000000000, 0.9238795325112869605, 1.000000000000000000, 0.9238795325112869605, 1.000000000000000000, 0.9238795325112869605, 1.000000000000000000, 0.9238795325112869605, 1.000000000000000000, 0.9238795325112869605, 1.000000000000000000, 0.9238795325112869605, 1.000000000000000000, 0.9238795325112869605, 1.000000000000000000, 0.9238795325112869605, 1.000000000000000000, 0.9238795325112869605, 1.000000000000000000, 0.9238795325112869605, 1.000000000000000000, 0.9238795325112869605, 1.000000000000000000, 0.9238795325112869605, 1.000000000000000000, 0.9238795325112869605, 1.000000000000000000, 0.9238795325112869605, 1.000000000000000000, 0.9238795325112869605, 1.000000000000000000, 0.9238795325112869605, 1.000000000000000000, 0.9238795325112869605, 1.000000000000000000, 0.9238795325112869605, 1.000000000000000000, 0.9238795325112869605, 1.000000000000000000, 0.9238795325112869605, 1.000000000000000000),
 ( 1.000000000000000000, 0.9238795325112869605, 1.000000000000000000, 0.9238795325112869605, 1.000000000000000000, 0.9238795325112869605, 1.000000000000000000, 0.9238795325112869605, 1.000000000000000000, 0.9238795325112869605, 1.000000000000000000, 0.9238795325112869605, 1.000000000000000000, 0.9238795325112869605, 1.000000000000000000, 0.9238795325112869605, 1.000000000000000000, 0.9238795325112869605, 1.000000000000000000, 0.9238795325112869605, 1.000000000000000000, 0.9238795325112869605, 1.000000000000000000, 0.9238795325112869605, 1.000000000000000000, 0.9238795325112869605, 1.000000000000000000, 0.9238795325112869605, 1.000000000000000000, 0.9238795325112869605, 1.000000000000000000, 0.9238795325112869605, 1.000000000000000000, 0.9238795325112869605, 1.000000000000000000, 0.9238795325112869605, 1.000000000000000000, 0.9238795325112869605, 1.000000000000000000, 0.9238795325112869605, 1.000000000000000000, 0.9238795325112869605, 1.000000000000000000, 0.9238795325112869605, 1.000000000000000000, 0.9238795325112869605, 1.000000000000000000, 0.9238795325112869605, 1.000000000000000000, 0.9238795325112869605, 1.000000000000000000, 0.9238795325112869605, 1.000000000000000000, 0.9238795325112869605, 1.000000000000000000, 0.9238795325112869605, 1.000000000000000000, 0.9238795325112869605, 1.000000000000000000, 0.9238795325112869605, 1.000000000000000000, 0.9238795325112869605, 1.000000000000000000, 0.9238795325112869605, 1.000000000000000000, 0.9238795325112869605, 1.000000000000000000, 0.9238795325112869605, 1.000000000000000000, 0.9238795325112869605, 1.000000000000000000, 0.9238795325112869605, 1.000000000000000000, 0.9238795325112869605, 1.000000000000000000, 0.9238795325112869605, 1.000000000000000000, 0.9238795325112869605, 1.000000000000000000, 0.9238795325112869605, 1.000000000000000000, 0.9238795325112869605, 1.000000000000000000, 0.9238795325112869605, 1.000000000000000000, 0.9238795325112869605, 1.000000000000000000, 0.9238795325112869605, 1.000000000000000000, 0.9238795325112869605, 1.000000000000000000, 0.9238795325112869605, 1.000000000000000000, 0.9238795325112869605, 1.000000000000000000, 0.9238795325112869605, 1.000000000000000000, 0.9238795325112869605, 1.000000000000000000, 0.9238795325112869605, 1.000000000000000000, 0.9238795325112869605, 1.000000000000000000, 0.9238795325112869605, 1.000000000000000000, 0.9238795325112869605, 1.000000000000000000, 0.9238795325112869605, 1.000000000000000000, 0.9238795325112869605, 1.000000000000000000, 0.9238795325112869605, 1.000000000000000000, 0.9238795325112869605, 1.000000000000000000, 0.9238795325112869605, 1.000000000000000000, 0.9238795325112869605, 1.000000000000000000, 0.9238795325112869605, 1.000000000000000000, 0.9238795325112869605, 1.000000000000000000, 0.9238795325112869605, 1.000000000000000000, 0.9238795325112869605, 1.000000000000000000, 0.9238795325112869605, 1.000000000000000000, 0.9238795325112869605, 1.000000000000000000, 0.9238795325112869605, 1.000000000000000000, 0.9238795325112869605, 1.000000000000000000, 0.9238795325112869605, 1.000000000000000000, 0.9238795325112869605, 1.000000000000000000, 0.9238795325112869605, 1.000000000000000000, 0.9238795325112869605, 1.000000000000000000, 0.9238795325112869605, 1.000000000000000000, 0.9238795325112869605, 1.000000000000000000, 0.9238795325112869605, 1.000000000000000000, 0.9238795325112869605, 1.000000000000000000, 0.9238795325112869605, 1.000000000000000000, 0.9238795325112869605, 1.000000000000000000, 0.9238795325112869605, 1.000000000000000000, 0.9238795325112869605, 1.000000000000000000, 0.9238795325112869605, 1.000000000000000000) ) ) 
 REPRESENTATION_ITEM ( '' )  SURFACE ( )  );
#34013 = CARTESIAN_POINT ( 'NONE',  ( 124.3117748109119844, 0.1319031606808879209, -14.10382304977623669 ) ) ;
#34014 = CARTESIAN_POINT ( 'NONE',  ( 112.5126281442453120, -10.30919188438810075, -12.61870101168855918 ) ) ;
#34015 = ORIENTED_EDGE ( 'NONE', *, *, #21393, .F. ) ;
#34016 = CARTESIAN_POINT ( 'NONE',  ( 124.9357681442453014, -7.643976991954077427, -18.09477374809248928 ) ) ;
#34017 = CARTESIAN_POINT ( 'NONE',  ( 117.2294421295247844, -4.863998795839590272, -7.758215200338314688 ) ) ;
#34018 = PLANE ( 'NONE',  #34372 ) ;
#34019 = CARTESIAN_POINT ( 'NONE',  ( 109.5102233795247884, -8.938348069036489818, -17.46756447353520159 ) ) ;
#34020 = CARTESIAN_POINT ( 'NONE',  ( 111.9410827545248708, -6.936859964151250502, -8.388885654883777576 ) ) ;
#34021 = CARTESIAN_POINT ( 'NONE',  ( 107.9822546295247889, -4.863998795839590272, -7.631215200338315796 ) ) ;
#34022 = VECTOR ( 'NONE', #8382, 999.9999999999998863 ) ;
#34023 = CARTESIAN_POINT ( 'NONE',  ( 121.7590748109119687, -7.893985811506177619, -18.51759400769804742 ) ) ;
#34024 = CARTESIAN_POINT ( 'NONE',  ( 121.1918081442452859, -10.15424416112533912, -14.75197769757731336 ) ) ;
#34025 = VERTEX_POINT ( 'NONE', #15644 ) ;
#34026 = CARTESIAN_POINT ( 'NONE',  ( 124.2550481442452792, -9.988377603198980381, -10.36322818467138518 ) ) ;
#34027 = CARTESIAN_POINT ( 'NONE',  ( 113.0231681442453180, -10.15424416112533912, -14.75197769757731336 ) ) ;
#34028 = CARTESIAN_POINT ( 'NONE',  ( 121.5437981415388862, -0.1020945015694968705, -15.74893487844867757 ) ) ;
#34029 = CARTESIAN_POINT ( 'NONE',  ( 120.7379948109119709, -10.63000616557722466, -14.87417383870573495 ) ) ;
#34030 = CARTESIAN_POINT ( 'NONE',  ( 120.5110881442453206, -6.344957434206665248, -7.627207830600338134 ) ) ;
#34031 = CARTESIAN_POINT ( 'NONE',  ( 119.4656423109119743, -0.4387604401700512802, -15.73000352943951619 ) ) ;
#34032 = CARTESIAN_POINT ( 'NONE',  ( 126.0703014775786102, -0.1624402480850797581, -16.17319339645315424 ) ) ;
#34033 = DIRECTION ( 'NONE',  ( -0.000000000000000000, -0.9284778069183718952, -0.3713878862591649677 ) ) ;
#34034 = ORIENTED_EDGE ( 'NONE', *, *, #2161, .F. ) ;
#34035 = LINE ( 'NONE', #17397, #21559 ) ;
#34036 = CARTESIAN_POINT ( 'NONE',  ( 118.6950019144190520, -1.220279397241701647, -16.99638242193885418 ) ) ;
#34037 = CARTESIAN_POINT ( 'NONE',  ( 124.3117748109119844, 0.1319031606808879209, -14.10382304977623669 ) ) ;
#34038 = CARTESIAN_POINT ( 'NONE',  ( 108.8851452545248151, -9.868328341294098749, -15.46607636864997204 ) ) ;
#34039 = CARTESIAN_POINT ( 'NONE',  ( 110.5520202545248054, 0.1403307496149616695, -11.32035403202665336 ) ) ;
#34040 = CARTESIAN_POINT ( 'NONE',  ( 118.4689281442453250, -10.15424416112533912, -14.75197769757731336 ) ) ;
#34041 =( NAMED_UNIT ( * ) PLANE_ANGLE_UNIT ( ) SI_UNIT ( $, .RADIAN. ) );
#34042 = CARTESIAN_POINT ( 'NONE',  ( 117.7314814775786260, -5.574606645277164318, -18.38911715685844683 ) ) ;
#34043 = CARTESIAN_POINT ( 'NONE',  ( 122.3263414775786373, -6.344957434206665248, -7.627207830600338134 ) ) ;
#34044 = EDGE_LOOP ( 'NONE', ( #15569, #35916, #26489, #42804 ) ) ;
#34045 = AXIS2_PLACEMENT_3D ( 'NONE', #366, #18147, #21791 ) ;
#34046 = CARTESIAN_POINT ( 'NONE',  ( 120.7947214775786193, -0.8288870151387760510, -10.36305467784173118 ) ) ;
#34047 = CARTESIAN_POINT ( 'NONE',  ( 120.0005481442453146, -5.638512984488999180, -18.83840828888717311 ) ) ;
#34048 = CARTESIAN_POINT ( 'NONE',  ( 124.8223148109119762, 0.9020085738987339008, -11.91225656197089222 ) ) ;
#34049 = CARTESIAN_POINT ( 'NONE',  ( 124.2550481442452792, -0.1624402480850797581, -16.17319339645315424 ) ) ;
#34050 = VERTEX_POINT ( 'NONE', #26127 ) ;
#34051 = DIRECTION ( 'NONE',  ( 0.000000000000000000, -0.3818493186865936084, 0.9242245927363024194 ) ) ;
#34052 = EDGE_CURVE ( 'NONE', #31689, #37171, #8796, .T. ) ;
#34053 = CARTESIAN_POINT ( 'NONE',  ( 125.2194014775786286, -10.30919188438810075, -12.61870101168855918 ) ) ;
#34054 = CARTESIAN_POINT ( 'NONE',  ( 114.1577014775786552, -3.505236298600246325, -18.68346056562440793 ) ) ;
#34055 = VECTOR ( 'NONE', #14502, 1000.000000000000114 ) ;
#34056 = CARTESIAN_POINT ( 'NONE',  ( 125.2761281442453054, -10.63000616557722466, -14.87417383870573495 ) ) ;
#34057 = CARTESIAN_POINT ( 'NONE',  ( 66.38809756183205479, -36.79083284667497367, -4.893215200338314474 ) ) ;
#34058 = CARTESIAN_POINT ( 'NONE',  ( 124.7440798109119697, -7.200787124940443817, -17.81845355600750835 ) ) ;
#34059 = ORIENTED_EDGE ( 'NONE', *, *, #20953, .T. ) ;
#34060 = CARTESIAN_POINT ( 'NONE',  ( 67.69189222814998175, -49.76310523276723785, -40.89321520033831092 ) ) ;
#34061 = CARTESIAN_POINT ( 'NONE',  ( 124.1726284085826251, 3.074464114999942765, -12.40349330775361025 ) ) ;
#34062 = CARTESIAN_POINT ( 'NONE',  ( 108.0517077545248696, -2.791137627527939813, -18.39754474579286025 ) ) ;
#34063 = EDGE_CURVE ( 'NONE', #14190, #9071, #5574, .T. ) ;
#34064 = CARTESIAN_POINT ( 'NONE',  ( 115.6220983795247861, -8.402594152722633325, -16.93181055722144990 ) ) ;
#34065 = CARTESIAN_POINT ( 'NONE',  ( 123.3474214775786209, -0.1624402480850797581, -16.17319339645315424 ) ) ;
#34066 = CARTESIAN_POINT ( 'NONE',  ( 114.7816948109119863, -9.859900752359374465, -12.68260735090039404 ) ) ;
#34067 = CARTESIAN_POINT ( 'NONE',  ( 126.7858337141697689, -6.477483175330938536, -18.42452263347122354 ) ) ;
#34068 = ORIENTED_EDGE ( 'NONE', *, *, #20999, .T. ) ;
#34069 = CYLINDRICAL_SURFACE ( 'NONE', #23715, 4.000000000000000888 ) ;
#34070 = CARTESIAN_POINT ( 'NONE',  ( 118.9794681442453026, -0.8288870151387760510, -10.36305467784173118 ) ) ;
#34071 = CARTESIAN_POINT ( 'NONE',  ( 114.1577014775786552, -3.505236298600246325, -18.68346056562440793 ) ) ;
#34072 = DIRECTION ( 'NONE',  ( 0.9908103287288504424, -0.1352586133457950590, 0.000000000000000000 ) ) ;
#34073 = CARTESIAN_POINT ( 'NONE',  ( 111.4348214775786801, -3.505236298600246325, -18.68346056562440793 ) ) ;
#34075 = CARTESIAN_POINT ( 'NONE',  ( 125.1626748109119802, -9.988377603198980381, -10.36322818467138518 ) ) ;
#34074 = DIRECTION ( 'NONE',  ( 0.000000000000000000, 0.000000000000000000, -1.000000000000000000 ) ) ;
#34076 = CARTESIAN_POINT ( 'NONE',  ( 125.0492214775786266, -3.505236298600246325, -18.68346056562440793 ) ) ;
#34077 = ORIENTED_EDGE ( 'NONE', *, *, #39257, .F. ) ;
#34078 = CARTESIAN_POINT ( 'NONE',  ( 112.8529881442453302, -1.561330072975668060, -17.79121239304076596 ) ) ;
#34079 = DIRECTION ( 'NONE',  ( 1.000000000000000000, 0.000000000000000000, -0.000000000000000000 ) ) ;
#34080 = CARTESIAN_POINT ( 'NONE',  ( 107.3571765045248299, -2.791137627527939813, -8.388885654883777576 ) ) ;
#34081 = CARTESIAN_POINT ( 'NONE',  ( 123.6310548109119765, -4.153390946401325223, -8.397313243818185668 ) ) ;
#34082 = CARTESIAN_POINT ( 'NONE',  ( 119.2631014775786298, -9.565557343593413364, -10.61323700422348004 ) ) ;
#34083 = DIRECTION ( 'NONE',  ( -0.9489384314806880161, -0.3124801273375112931, -0.04326688431242012300 ) ) ;
#34084 = CARTESIAN_POINT ( 'NONE',  ( 106.1070202545248407, -10.62599879583958717, -15.77991374673208469 ) ) ;
#34085 = CARTESIAN_POINT ( 'NONE',  ( 111.0762212410415799, 0.7607806665037644134, -12.14321520033829316 ) ) ;
#34086 = DIRECTION ( 'NONE',  ( -0.000000000000000000, -0.9284778069183721172, -0.3713878862591650232 ) ) ;
#34087 = CARTESIAN_POINT ( 'NONE',  ( 112.8529881442453302, -7.894159318335819187, -9.358103419637840759 ) ) ;
#34088 = CARTESIAN_POINT ( 'NONE',  ( 92.22433883960545131, -8.119819663282910938, -18.64321520033831803 ) ) ;
#34089 = VECTOR ( 'NONE', #40327, 1000.000000000000000 ) ;
#34090 = CARTESIAN_POINT ( 'NONE',  ( 117.6180281442453150, -0.4660016031367954503, -10.09054647747473155 ) ) ;
#34091 = CARTESIAN_POINT ( 'NONE',  ( 114.4413952545248350, 0.8980012041604421569, -11.00651665394454071 ) ) ;
#34092 = CARTESIAN_POINT ( 'NONE',  ( 123.9146881442452894, 0.9020085738987339008, -11.91225656197089222 ) ) ;
#34093 = CARTESIAN_POINT ( 'NONE',  ( 121.9292548109119849, -1.561330072975668948, -17.79121239304076951 ) ) ;
#34094 = CARTESIAN_POINT ( 'NONE',  ( 111.5497331777918788, -0.01829820670803256055, -14.64321520033831447 ) ) ;
#34095 = CARTESIAN_POINT ( 'NONE',  ( 118.5823814775786360, -1.834011780172310813, -8.268836392978581529 ) ) ;
#34096 = CARTESIAN_POINT ( 'NONE',  ( -12.36826994950264513, -4.374949827406455327, -8.593215200338315540 ) ) ;
#34097 = VERTEX_POINT ( 'NONE', #5590 ) ;
#34098 = CARTESIAN_POINT ( 'NONE',  ( 115.0653281442453277, -3.505236298600246325, -18.68346056562440793 ) ) ;
#34099 = CARTESIAN_POINT ( 'NONE',  ( 112.0020881442453344, -9.565557343593413364, -10.61323700422348004 ) ) ;
#34100 = CARTESIAN_POINT ( 'NONE',  ( 122.2696148109119889, -4.089484607189486809, -7.948022111789456723 ) ) ;
#34101 = CARTESIAN_POINT ( 'NONE',  ( 112.7395348109119766, -5.638512984488999180, -18.83840828888717311 ) ) ;
#34102 =( BOUNDED_CURVE ( )  B_SPLINE_CURVE ( 2, ( #29353, #39844, #35957, #5171, #32754 ),
 .UNSPECIFIED., .F., .T. ) 
 B_SPLINE_CURVE_WITH_KNOTS ( ( 3, 2, 3 ),
 ( 5.122041608693530667E-06, 0.007812500000000000000, 0.01412175834311804080 ),
 .UNSPECIFIED. ) 
 CURVE ( )  GEOMETRIC_REPRESENTATION_ITEM ( )  RATIONAL_B_SPLINE_CURVE ( ( 0.9999002530354920149, 0.9239294387131110620, 1.000000000000000000, 0.9385262470930929579, 0.9763430640193200283 ) ) 
 REPRESENTATION_ITEM ( '' )  );
#34103 = CARTESIAN_POINT ( 'NONE',  ( 111.4348214775786801, -3.505236298600246325, -18.68346056562440793 ) ) ;
#34104 = ORIENTED_EDGE ( 'NONE', *, *, #37844, .F. ) ;
#34105 = CARTESIAN_POINT ( 'NONE',  ( 118.2420214775786320, -6.222761293078241884, -8.102969835052219238 ) ) ;
#34106 = CARTESIAN_POINT ( 'NONE',  ( 112.2857214775786474, -4.089484607189486809, -7.948022111789456723 ) ) ;
#34107 = CARTESIAN_POINT ( 'NONE',  ( 111.8021765045248372, -2.791137627527939813, -8.388885654883777576 ) ) ;
#34108 = CARTESIAN_POINT ( 'NONE',  ( 124.6521348109119884, -7.894159318335828068, -9.358103419637847864 ) ) ;
#34109 = CARTESIAN_POINT ( 'NONE',  ( 123.8443641859119992, -1.409680983675146271, -17.55938974467885316 ) ) ;
#34110 = CARTESIAN_POINT ( 'NONE',  ( 114.0941296295247867, -4.863998795839590272, -19.15521520033831493 ) ) ;
#34111 = ORIENTED_EDGE ( 'NONE', *, *, #26685, .T. ) ;
#34112 = ADVANCED_BREP_SHAPE_REPRESENTATION ( '', ( #6132, #12375 ), #18656 ) ;
#34113 = LINE ( 'NONE', #45065, #7492 ) ;
#34114 = CARTESIAN_POINT ( 'NONE',  ( 125.0492214775786266, -6.344957434206665248, -7.627207830600338134 ) ) ;
#34115 = CARTESIAN_POINT ( 'NONE',  ( 85.56953267055843071, -21.30583187727814121, -4.893215200338314474 ) ) ;
#34116 = FACE_OUTER_BOUND ( 'NONE', #17479, .T. ) ;
#34117 = ADVANCED_FACE ( 'NONE', ( #43680 ), #16092, .F. ) ;
#34118 = CARTESIAN_POINT ( 'NONE',  ( 116.4360542988829081, 2.232332096932356791, -6.377660291141232562 ) ) ;
#34119 = DIRECTION ( 'NONE',  ( -0.000000000000000000, -0.9284778069183720062, -0.3713878862591650232 ) ) ;
#34120 = CARTESIAN_POINT ( 'NONE',  ( 105.9681140045248355, 0.1403307496149616695, -15.46607636864997204 ) ) ;
#34121 = FACE_OUTER_BOUND ( 'NONE', #38059, .T. ) ;
#34122 = CARTESIAN_POINT ( 'NONE',  ( 119.6034614775786196, -6.344957434206665248, -7.627207830600338134 ) ) ;
#34123 = CARTESIAN_POINT ( 'NONE',  ( 122.9382985609119743, -0.08252387247370714107, -11.91645802438286950 ) ) ;
#34124 = CYLINDRICAL_SURFACE ( 'NONE', #29576, 1.199999999999999734 ) ;
#34125 = CARTESIAN_POINT ( 'NONE',  ( 125.7866681442452688, -0.4660016031367893996, -10.09054647747474043 ) ) ;
#34126 = CARTESIAN_POINT ( 'NONE',  ( 120.1707281442453166, -9.565557343593413364, -10.61323700422348004 ) ) ;
#34127 = CARTESIAN_POINT ( 'NONE',  ( 119.7434548109119561, -4.073510663624176686, -18.95665693152923126 ) ) ;
#34128 = ORIENTED_EDGE ( 'NONE', *, *, #30077, .F. ) ;
#34129 = CARTESIAN_POINT ( 'NONE',  ( 125.3328548109119964, -9.261995988541697145, -16.69588392320189030 ) ) ;
#34130 = CARTESIAN_POINT ( 'NONE',  ( 121.0783548109119749, 0.2603800115204892296, -16.42320221600525088 ) ) ;
#34131 = DIRECTION ( 'NONE',  ( 0.9609149988134843001, -0.1028163501681632064, 0.2570431154366505933 ) ) ;
#34132 = CARTESIAN_POINT ( 'NONE',  ( 116.1431348109119881, 0.1319031606808879209, -14.10382304977623669 ) ) ;
#34133 = CARTESIAN_POINT ( 'NONE',  ( 123.9714148109119805, -0.4660016031367893996, -10.09054647747474043 ) ) ;
#34134 = CARTESIAN_POINT ( 'NONE',  ( 109.7880358795247986, -0.7896495226426338832, -17.46756447353520159 ) ) ;
#34135 = CARTESIAN_POINT ( 'NONE',  ( 79.79010115959992788, 5.106172230548759572, -6.893215200338315363 ) ) ;
#34136 = CARTESIAN_POINT ( 'NONE',  ( 83.01822478718537468, -31.84465705650555734, -23.29249428169273628 ) ) ;
#34137 = CARTESIAN_POINT ( 'NONE',  ( 115.4624148109119943, -4.153390946401321671, -8.397313243818183892 ) ) ;
#34138 = CARTESIAN_POINT ( 'NONE',  ( 115.1787814775786387, -0.1624402480850797581, -16.17319339645315424 ) ) ;
#34139 = DIRECTION ( 'NONE',  ( 1.000000000000000000, 0.000000000000000000, -0.000000000000000000 ) ) ;
#34140 = CARTESIAN_POINT ( 'NONE',  ( 112.0799890045248475, -9.868328341294098749, -11.32035403202665869 ) ) ;
#34141 = ORIENTED_EDGE ( 'NONE', *, *, #11674, .F. ) ;
#34142 = CARTESIAN_POINT ( 'NONE',  ( 111.5125327111057345, -1.267766418764825875, -16.93314635290698789 ) ) ;
#34143 = CARTESIAN_POINT ( 'NONE',  ( 114.5547881442453217, -5.638512984488999180, -18.83840828888717311 ) ) ;
#34144 = CARTESIAN_POINT ( 'NONE',  ( 112.8729331642484510, -2.215723800389698184, -18.16877924232191788 ) ) ;
#34145 = CARTESIAN_POINT ( 'NONE',  ( 121.6186891859119896, -1.406689858478933353, -17.56299727309130887 ) ) ;
#34146 = CARTESIAN_POINT ( 'NONE',  ( 120.5768923109119868, -0.4387604401700512802, -15.73000352943951619 ) ) ;
#34147 = ORIENTED_EDGE ( 'NONE', *, *, #9440, .F. ) ;
#34148 = CARTESIAN_POINT ( 'NONE',  ( 63.69189222814998175, -80.85404093559408523, -31.07034979220001603 ) ) ;
#34149 = CARTESIAN_POINT ( 'NONE',  ( 116.8074716117156413, -11.72235701766462057, -21.41449971386014184 ) ) ;
#34150 = ORIENTED_EDGE ( 'NONE', *, *, #6053, .T. ) ;
#34151 = CARTESIAN_POINT ( 'NONE',  ( 116.8238548109119819, -4.089484607189486809, -7.948022111789456723 ) ) ;
#34152 = CARTESIAN_POINT ( 'NONE',  ( 114.3846081442453197, -10.63000616557722466, -14.87417383870573495 ) ) ;
#34153 = AXIS2_PLACEMENT_3D ( 'NONE', #7448, #17950, #10671 ) ;
#34154 = CARTESIAN_POINT ( 'NONE',  ( 118.8660148109119774, 0.1319031606808879209, -14.10382304977623669 ) ) ;
#34155 = CARTESIAN_POINT ( 'NONE',  ( 120.2542535264548889, -8.247323210606168686, -17.08054893949881148 ) ) ;
#34156 = CARTESIAN_POINT ( 'NONE',  ( 120.2274548109119934, 0.5811942927096110934, -14.16772938898807510 ) ) ;
#34157 = CARTESIAN_POINT ( 'NONE',  ( 118.0718414775786300, -9.261995988541697145, -16.69588392320189030 ) ) ;
#34158 = CARTESIAN_POINT ( 'NONE',  ( 109.1629577545248395, -2.791137627527939813, -18.39754474579286025 ) ) ;
#34159 = CARTESIAN_POINT ( 'NONE',  ( 112.2857214775786474, -5.574606645277164318, -18.38911715685844683 ) ) ;
#34160 = CARTESIAN_POINT ( 'NONE',  ( 65.82164714941100669, 4.169909004287361221, -19.39321520033831447 ) ) ;
#34161 = ORIENTED_EDGE ( 'NONE', *, *, #1470, .T. ) ;
#34162 = CARTESIAN_POINT ( 'NONE',  ( 119.3765548109119834, 0.9020085738987339008, -11.91225656197089222 ) ) ;
#34163 = DIRECTION ( 'NONE',  ( 0.9387755102040806765, -0.3445294493088623122, 0.000000000000000000 ) ) ;
#34164 = CARTESIAN_POINT ( 'NONE',  ( 113.9875214775786532, -0.4660016031367893996, -10.09054647747474043 ) ) ;
#34165 = VERTEX_POINT ( 'NONE', #11777 ) ;
#34166 = CARTESIAN_POINT ( 'NONE',  ( 121.9292548109119849, -1.561330072975668948, -17.79121239304076951 ) ) ;
#34167 = CARTESIAN_POINT ( 'NONE',  ( 110.2184548109119788, -6.243778871467079661, -12.80482167309617125 ) ) ;
#34168 = CARTESIAN_POINT ( 'NONE',  ( 125.4584548109119737, -6.396860573544808304, -19.01579431533362907 ) ) ;
#34169 = CARTESIAN_POINT ( 'NONE',  ( 78.19609438264805590, -57.93615991906383300, -0.7640671700936263466 ) ) ;
#34170 = CARTESIAN_POINT ( 'NONE',  ( 116.7671281442453335, -7.643976991954077427, -18.09477374809248928 ) ) ;
#34171 = DIRECTION ( 'NONE',  ( -0.8636456077245092677, 0.5040994586965584778, 0.000000000000000000 ) ) ;
#34172 = CARTESIAN_POINT ( 'NONE',  ( 117.2209414775786485, -2.084020599724406786, -8.691656652584148546 ) ) ;
#34173 = CARTESIAN_POINT ( 'NONE',  ( 121.1658748871816300, -6.188980713775695364, -18.62212668298318619 ) ) ;
#34174 = CARTESIAN_POINT ( 'NONE',  ( 116.1431348109119881, 0.1319031606808879209, -14.10382304977623669 ) ) ;
#34175 = CARTESIAN_POINT ( 'NONE',  ( 115.3489614775786407, -9.261995988541697145, -16.69588392320189030 ) ) ;
#34176 = CARTESIAN_POINT ( 'NONE',  ( 123.0772048109119652, -2.527210466738041728, -8.967976844669124148 ) ) ;
#34177 = VECTOR ( 'NONE', #40831, 1000.000000000000114 ) ;
#34178 = CARTESIAN_POINT ( 'NONE',  ( 113.3635281442453504, -9.988377603198976828, -10.36322818467138340 ) ) ;
#34179 = CARTESIAN_POINT ( 'NONE',  ( 116.4267681442453153, -6.222761293078241884, -8.102969835052219238 ) ) ;
#34180 = CARTESIAN_POINT ( 'NONE',  ( 113.4769814775786330, 0.4262465694468514643, -12.03445270309931736 ) ) ;
#34181 = CARTESIAN_POINT ( 'NONE',  ( 116.2565881442453133, -0.8288870151387760510, -10.36305467784173118 ) ) ;
#34182 = ORIENTED_EDGE ( 'NONE', *, *, #28698, .F. ) ;
#34183 = CARTESIAN_POINT ( 'NONE',  ( 112.5126281442453120, -10.30919188438810075, -12.61870101168855918 ) ) ;
#34184 = EDGE_CURVE ( 'NONE', #7030, #14703, #24536, .T. ) ;
#34185 = CARTESIAN_POINT ( 'NONE',  ( 105.4819421295248247, 0.8980012041604618078, -13.39321520033831447 ) ) ;
#34186 = CARTESIAN_POINT ( 'NONE',  ( 106.3848327545248651, -6.936859964151250502, -8.388885654883777576 ) ) ;
#34187 = CARTESIAN_POINT ( 'NONE',  ( 105.1346765045248475, -2.791137627527939813, -8.388885654883777576 ) ) ;
#34188 = CARTESIAN_POINT ( 'NONE',  ( 64.40114967617560637, -36.78199758899061322, -5.510037480650538555 ) ) ;
#34189 = CARTESIAN_POINT ( 'NONE',  ( 117.4478481442453131, 0.2603800115204892296, -16.42320221600525088 ) ) ;
#34190 = EDGE_LOOP ( 'NONE', ( #39392, #27112, #42249, #38468, #23763, #35955 ) ) ;
#34191 = CARTESIAN_POINT ( 'NONE',  ( 61.69189222814998175, -48.76310523276723785, -23.89321520033831803 ) ) ;
#34192 = CARTESIAN_POINT ( 'NONE',  ( 124.9924948109119924, -4.089484607189473486, -7.948022111789465605 ) ) ;
#34193 = CARTESIAN_POINT ( 'NONE',  ( 118.9794681442453026, -0.8288870151387760510, -10.36305467784173118 ) ) ;
#34194 = CARTESIAN_POINT ( 'NONE',  ( 128.2184548109119930, 1.087851763053662602, -12.63461456455805276 ) ) ;
#34195 = CARTESIAN_POINT ( 'NONE',  ( 123.9146881442452894, 0.9020085738987339008, -11.91225656197089222 ) ) ;
#34196 = CARTESIAN_POINT ( 'NONE',  ( 106.8015515045248378, -2.477300249445798297, -7.631215200338321125 ) ) ;
#34197 = CARTESIAN_POINT ( 'NONE',  ( 124.3880659103642188, -8.454079026182052203, -17.47208793939444149 ) ) ;
#34198 = ORIENTED_EDGE ( 'NONE', *, *, #37471, .F. ) ;
#34199 = CARTESIAN_POINT ( 'NONE',  ( 143.3676850761856940, -69.76310523276724496, -16.89321520033831447 ) ) ;
#34200 = CARTESIAN_POINT ( 'NONE',  ( 120.7947214775786193, -0.8288870151387760510, -10.36305467784173118 ) ) ;
#34201 = CARTESIAN_POINT ( 'NONE',  ( 119.6601881442453106, -8.166667518702819706, -8.995218007635861213 ) ) ;
#34202 = CARTESIAN_POINT ( 'NONE',  ( 118.3554748109119998, -9.565557343593413364, -10.61323700422348004 ) ) ;
#34203 = CARTESIAN_POINT ( 'NONE',  ( 118.9794681442453026, -9.261995988541697145, -16.69588392320189030 ) ) ;
#34204 = ADVANCED_FACE ( 'NONE', ( #26357 ), #28186, .T. ) ;
#34205 = CARTESIAN_POINT ( 'NONE',  ( 94.86797725101170897, -25.23805398138116018, -13.87635650542741850 ) ) ;
#34206 = CARTESIAN_POINT ( 'NONE',  ( 107.2294421295247844, -9.051693226400931991, -21.39321520033831447 ) ) ;
#34207 = CARTESIAN_POINT ( 'NONE',  ( 122.0427081442452817, -9.859900752359378018, -12.68260735090039759 ) ) ;
#34208 = ORIENTED_EDGE ( 'NONE', *, *, #33926, .F. ) ;
#34209 = EDGE_CURVE ( 'NONE', #29406, #13605, #4868, .T. ) ;
#34210 = EDGE_CURVE ( 'NONE', #23154, #6107, #32725, .T. ) ;
#34211 = CARTESIAN_POINT ( 'NONE',  ( 85.45605303719084134, -15.74807682313488222, -16.89321520033831447 ) ) ;
#34212 = AXIS2_PLACEMENT_3D ( 'NONE', #30783, #41064, #12562 ) ;
#34213 = CARTESIAN_POINT ( 'NONE',  ( 117.1074881442453233, -10.63000616557722466, -14.87417383870573495 ) ) ;
#34214 = CARTESIAN_POINT ( 'NONE',  ( 121.3052614775786111, -7.643976991954077427, -18.09477374809248928 ) ) ;
#34215 = VERTEX_POINT ( 'NONE', #19060 ) ;
#34216 = CARTESIAN_POINT ( 'NONE',  ( 122.9382985609119743, -0.08252387247370887580, -11.91645802438286417 ) ) ;
#34217 = CARTESIAN_POINT ( 'NONE',  ( 137.1886586612299652, -0.1096322012115264061, -11.00619489583255906 ) ) ;
#34218 = CARTESIAN_POINT ( 'NONE',  ( 119.7736414775786358, -10.30919188438810075, -12.61870101168855918 ) ) ;
#34219 = CARTESIAN_POINT ( 'NONE',  ( 110.2742077545248094, -7.250697342233347165, -7.631215200338321125 ) ) ;
#34220 = CARTESIAN_POINT ( 'NONE',  ( 121.1350814775786233, -9.859900752359378018, -12.68260735090039759 ) ) ;
#34221 = ORIENTED_EDGE ( 'NONE', *, *, #2130, .F. ) ;
#34222 = ORIENTED_EDGE ( 'NONE', *, *, #39322, .F. ) ;
#34223 = CIRCLE ( 'NONE', #39337, 2.999999999999999556 ) ;
#34224 = CARTESIAN_POINT ( 'NONE',  ( 124.9357681442453014, -7.643976991954077427, -18.09477374809248928 ) ) ;
#34225 = CARTESIAN_POINT ( 'NONE',  ( 125.2761281442453054, 0.4262465694468514643, -12.03445270309931736 ) ) ;
#34226 = AXIS2_PLACEMENT_3D ( 'NONE', #38640, #41655, #10414 ) ;
#34227 = FACE_OUTER_BOUND ( 'NONE', #10619, .T. ) ;
#34228 = CARTESIAN_POINT ( 'NONE',  ( 61.69189222814998175, -69.76310523276724496, -32.79321520033831661 ) ) ;
#34229 = CARTESIAN_POINT ( 'NONE',  ( 120.4543614775786295, -4.089484607189486809, -7.948022111789456723 ) ) ;
#34230 = ADVANCED_FACE ( 'NONE', ( #4918 ), #40560, .T. ) ;
#34231 = CARTESIAN_POINT ( 'NONE',  ( 109.2294421295247844, 0.8460904216231607267, -19.39321520033831447 ) ) ;
#34232 = FACE_OUTER_BOUND ( 'NONE', #28171, .T. ) ;
#34233 = CARTESIAN_POINT ( 'NONE',  ( 120.6245414775786458, -9.988377603198976828, -10.36322818467138340 ) ) ;
#34235 = CARTESIAN_POINT ( 'NONE',  ( 120.7947214775786193, -0.8288870151387760510, -10.36305467784173118 ) ) ;
#34234 = CARTESIAN_POINT ( 'NONE',  ( 117.4478481442453131, 0.2603800115204892296, -16.42320221600525088 ) ) ;
#34236 = CARTESIAN_POINT ( 'NONE',  ( -7.923679509334008664, -5.078949698970065540, -19.39321520033831447 ) ) ;
#34237 = CARTESIAN_POINT ( 'NONE',  ( 117.4478481442453131, 0.2603800115204892296, -16.42320221600525088 ) ) ;
#34238 = ADVANCED_FACE ( 'NONE', ( #2165 ), #20896, .T. ) ;
#34239 = EDGE_LOOP ( 'NONE', ( #37466, #2686, #3915, #24606, #1303 ) ) ;
#34240 = CARTESIAN_POINT ( 'NONE',  ( 123.8579614775786126, -9.859900752359378018, -12.68260735090039759 ) ) ;
#34241 = EDGE_CURVE ( 'NONE', #31913, #13199, #9971, .T. ) ;
#34242 = LINE ( 'NONE', #7104, #23489 ) ;
#34243 = CARTESIAN_POINT ( 'NONE',  ( 108.7462390045248242, 0.8980012041604421569, -15.77991374673208469 ) ) ;
#34244 = CARTESIAN_POINT ( 'NONE',  ( 114.5108483795247878, -8.402594152722688392, -16.93181055722141792 ) ) ;
#34245 = CARTESIAN_POINT ( 'NONE',  ( 107.2877233795247776, -8.938348069036489818, -17.46756447353520159 ) ) ;
#34246 = AXIS2_PLACEMENT_3D ( 'NONE', #30731, #33229, #36653 ) ;
#34247 = CARTESIAN_POINT ( 'NONE',  ( 123.2339681442453241, -6.344957434206665248, -7.627207830600338134 ) ) ;
#34248 = CARTESIAN_POINT ( 'NONE',  ( 122.7234281442452755, -4.153390946401325223, -8.397313243818185668 ) ) ;
#34249 = ORIENTED_EDGE ( 'NONE', *, *, #12793, .T. ) ;
#34250 = CARTESIAN_POINT ( 'NONE',  ( 124.3117748109119844, -10.30919188438810075, -12.61870101168855918 ) ) ;
#34251 = CARTESIAN_POINT ( 'NONE',  ( 112.3424481442453384, -3.505236298600246325, -18.68346056562440793 ) ) ;
#34252 = DIRECTION ( 'NONE',  ( 0.000000000000000000, 0.9242245927363040847, 0.3818493186865897226 ) ) ;
#34253 = CARTESIAN_POINT ( 'NONE',  ( 121.9292548109119849, -1.561330072975668948, -17.79121239304076951 ) ) ;
#34254 = CARTESIAN_POINT ( 'NONE',  ( 120.1140014775786398, -1.561330072975668504, -17.79121239304076951 ) ) ;
#34255 = CARTESIAN_POINT ( 'NONE',  ( 119.9486391859119863, -8.318316608003105017, -9.227040655997587493 ) ) ;
#34256 = CARTESIAN_POINT ( 'NONE',  ( 125.9568481442452850, -3.505236298600246325, -18.68346056562440793 ) ) ;
#34257 = CARTESIAN_POINT ( 'NONE',  ( 111.7184548109119788, -9.261995988541697145, -16.69588392320189030 ) ) ;
#34258 = CARTESIAN_POINT ( 'NONE',  ( 107.0099108795247815, -8.938348069036489818, -9.318865927141430916 ) ) ;
#34259 = ORIENTED_EDGE ( 'NONE', *, *, #4755, .F. ) ;
#34260 = DIRECTION ( 'NONE',  ( 1.000000000000000000, 0.000000000000000000, 0.000000000000000000 ) ) ;
#34261 = CARTESIAN_POINT ( 'NONE',  ( 113.2500748109119968, -3.505236298600246325, -18.68346056562440793 ) ) ;
#34262 = CARTESIAN_POINT ( 'NONE',  ( 122.2128881442453263, -7.643976991954077427, -18.09477374809248928 ) ) ;
#34263 = CARTESIAN_POINT ( 'NONE',  ( 106.1764733795248219, -1.325403438956436419, -9.854619843455211026 ) ) ;
#34264 = CARTESIAN_POINT ( 'NONE',  ( 105.8292077545248446, -2.791137627527939813, -18.39754474579286025 ) ) ;
#34265 = AXIS2_PLACEMENT_3D ( 'NONE', #30596, #44513, #37663 ) ;
#34266 = CARTESIAN_POINT ( 'NONE',  ( 123.0637881442452937, -8.899110576539710493, -16.42337572283490132 ) ) ;
#34267 = CARTESIAN_POINT ( 'NONE',  ( 114.7249681442453237, -9.565557343593413364, -10.61323700422348004 ) ) ;
#34268 = CARTESIAN_POINT ( 'NONE',  ( 111.7184548109119788, -0.8288870151387760510, -10.36305467784173118 ) ) ;
#34269 = ORIENTED_EDGE ( 'NONE', *, *, #20054, .T. ) ;
#34270 = ADVANCED_FACE ( 'NONE', ( #35929 ), #29998, .F. ) ;
#34271 = CARTESIAN_POINT ( 'NONE',  ( 122.6667014775786413, -2.084020599724406786, -8.691656652584148546 ) ) ;
#34272 = CARTESIAN_POINT ( 'NONE',  ( 118.4689281442453392, 0.9020085738987339008, -11.91225656197089222 ) ) ;
#34273 = CARTESIAN_POINT ( 'NONE',  ( 96.54708369096698561, -27.78532125115470208, -14.69016690077367926 ) ) ;
#34274 = VERTEX_POINT ( 'NONE', #36821 ) ;
#34275 = CARTESIAN_POINT ( 'NONE',  ( 75.95778847736481509, -3.256761025687722189, -9.893215200338316251 ) ) ;
#34276 = ORIENTED_EDGE ( 'NONE', *, *, #16779, .F. ) ;
#34277 = CIRCLE ( 'NONE', #9553, 0.5000000000000043299 ) ;
#34278 = CARTESIAN_POINT ( 'NONE',  ( 116.0296814775786345, -1.833838273342658809, -17.42832698103878286 ) ) ;
#34279 = CARTESIAN_POINT ( 'NONE',  ( 113.8173414775786512, -9.565557343593413364, -10.61323700422348004 ) ) ;
#34280 =( BOUNDED_SURFACE ( )  B_SPLINE_SURFACE ( 1, 2, ( 
 ( #30393, #13523, #27204, #34251, #5750, #6219, #26751, #41122, #2335, #3024, #43854, #16947, #40433, #23566, #9413, #34027, #26970, #30841, #19670, #30168, #44764, #23324, #37210, #37447, #9644, #9881, #5982, #2795, #44315, #19907, #33792, #2564, #13071, #20142, #30617, #44534, #13296, #23791, #8503, #22407, #36077, #2322, #19215, #26735, #12608, #19656, #15343, #8955, #36300, #26510, #25827, #36966, #8279, #8722, #22855, #22628, #1423, #4848, #40418, #33543, #39960, #5299, #18984, #16019, #29927, #36526, #5068, #22181, #26281, #18767, #5737, #43841, #9178, #23085, #15566, #29470, #15794, #29252, #1642, #36746, #16250, #40189, #32656, #5514, #32873, #30153, #43161, #44069, #12835, #39734, #43385, #26056, #12153, #11929, #33095, #1865, #29696, #43607, #12383, #19434, #33319, #2093, #31044, #27188, #30600, #19891, #6203, #34672, #9866, #20573, #27640, #16931, #23550, #44974, #20792, #23775, #36, #13509, #2548, #13948, #13282, #24216, #3231, #37667, #26954, #16475, #34450, #13055, #33778, #23999, #37887, #20125, #30378, #41108, #44517, #34010, #40876, #44300, #13731, #6442, #2781, #37193, #40643, #9629, #37433, #16706, #23309, #3458, #20351, #9398, #41554, #6882, #34235, #41337, #3009, #10314, #30826, #38107, #5967, #44750, #10096, #27417, #6663, #17157, #17375, #31263, #14389, #24877, #38538, #35567, #4340, #28301, #24653, #41771, #694, #10531, #11429, #18260, #924, #32156, #35111, #3892, #35339, #34883, #21232, #11201, #14843, #14614, #24430, #25106, #7313, #25334, #3671, #39227, #28753, #255, #17812, #476, #31706, #38322, #42213, #42658, #7992, #10974, #7539, #38769, #21900, #10755, #35794, #21456, #4111, #7099, #18032, #4566, #31929, #7772, #18490, #28531, #42437, #32380, #1147, #39002, #27861, #21679, #17592, #21009, #31485, #14164, #28082, #41990, #1372, #22129, #8897, #32602, #8223, #43555, #12323, #25777, #39459, #32818, #18931, #39684, #15284, #36022, #5459, #36473, #26223, #9122, #36913, #42883, #15064, #15739, #29416, #19379, #18711, #12099, #26003 ),
 ( #19156, #4790, #43330, #33487, #29641, #33267, #8668, #5013, #28978, #23026, #5240, #29191, #40132, #2042, #8449, #22352, #33037, #43103, #36246, #5684, #1812, #29869, #22795, #11873, #1588, #15509, #39907, #11644, #36689, #19603, #25553, #22571, #15965, #43784, #12549, #26456, #40358, #6148, #10039, #7206, #37609, #23719, #16193, #37826, #13455, #16422, #370, #2951, #14281, #9347, #44244, #13228, #23946, #44463, #21119, #41053, #10868, #44013, #2265, #6383, #30541, #30097, #9810, #20291, #34175, #33954, #24763, #16878, #13002, #27129, #38654, #3777, #27359, #26900, #40821, #12775, #17701, #9576, #23492, #7423, #28200, #30769, #33723, #34993, #31601, #30318, #42105, #21344, #44695, #26677, #20068, #40588, #41279, #23256, #2721, #37140, #5914, #19836, #2493, #37378, #16647, #31823, #14955, #32271, #813, #594, #18150, #35228, #18820, #39796, #18383, #28417, #28867, #7886, #15176, #32711, #25891, #42779, #4003, #36136, #35457, #24990, #4462, #1484, #32045, #14504, #8339, #8118, #22239, #25448, #42550, #29082, #17925, #42328, #35913, #39350, #11089, #1038, #11541, #11311, #38885, #8565, #7654, #4231, #14732, #21570, #29310, #22019, #28644, #39576, #15406, #25221, #4679, #39120, #4904, #21793, #43223, #35687, #18600, #32491, #1266, #42994, #11761, #11990, #25671, #9019, #19501, #33158, #30215, #44135, #22917, #19280, #36359, #40483, #5130, #6032, #12901, #40707, #26797, #29757, #43669, #29986, #29536, #15861, #5803, #9466, #9243, #19047, #19722, #1935, #19954, #43452, #33843, #23378, #40020, #12444, #40252, #26345, #32934, #36809, #37260, #2611, #5577, #2151, #33380, #16544, #5363, #30440, #16081, #43903, #1709, #12671, #44359, #26570, #2385, #13120, #23152, #37034, #27026, #40941, #33608, #22465, #16313, #12217, #15632, #26114, #8785, #22690, #36588, #41169, #16771, #3513, #27254, #2841, #38168, #6947, #20414, #34075, #27479, #13568, #34298, #9928, #30666, #97, #31106, #20851, #3730, #31549, #37497, #9696, #10373, #24061, #14011, #13350, #6727, #20638, #44587 ) ),
 .UNSPECIFIED., .F., .F., .F. ) 
 B_SPLINE_SURFACE_WITH_KNOTS ( ( 2, 2 ),
 ( 3, 2, 2, 2, 2, 2, 2, 2, 2, 2, 2, 2, 2, 2, 2, 2, 2, 2, 2, 2, 2, 2, 2, 2, 2, 2, 2, 2, 2, 2, 2, 2, 2, 2, 2, 2, 2, 2, 2, 2, 2, 2, 2, 2, 2, 2, 2, 2, 2, 2, 2, 2, 2, 2, 2, 2, 2, 2, 2, 2, 2, 2, 2, 2, 2, 2, 2, 2, 2, 2, 2, 2, 2, 2, 2, 2, 2, 2, 2, 2, 2, 2, 2, 2, 2, 2, 2, 2, 2, 2, 2, 2, 2, 2, 2, 2, 2, 2, 2, 2, 2, 2, 2, 2, 2, 2, 2, 2, 2, 2, 2, 2, 2, 2, 2, 2, 2, 2, 2, 2, 2, 2, 2, 2, 2, 2, 2, 2, 3 ),
 ( 0.000000000000000000, 1.000000000000000000 ),
 ( 0.000000000000000000, 0.007812500000000000000, 0.01562500000000000000, 0.02343750000000000000, 0.03125000000000000000, 0.03906250000000000000, 0.04687500000000000000, 0.05468750000000000000, 0.06250000000000000000, 0.07031250000000000000, 0.07812500000000000000, 0.08593750000000000000, 0.09375000000000000000, 0.1015625000000000000, 0.1093750000000000000, 0.1171875000000000000, 0.1250000000000000000, 0.1328125000000000000, 0.1406250000000000000, 0.1484375000000000000, 0.1562500000000000000, 0.1640625000000000000, 0.1718750000000000000, 0.1796875000000000000, 0.1875000000000000000, 0.1953125000000000000, 0.2031250000000000000, 0.2109375000000000000, 0.2187500000000000000, 0.2265625000000000000, 0.2343750000000000000, 0.2421875000000000000, 0.2500000000000000000, 0.2578125000000000000, 0.2656250000000000000, 0.2734375000000000000, 0.2812500000000000000, 0.2890625000000000000, 0.2968750000000000000, 0.3046875000000000000, 0.3125000000000000000, 0.3203125000000000000, 0.3281250000000000000, 0.3359375000000000000, 0.3437500000000000000, 0.3515625000000000000, 0.3593750000000000000, 0.3671875000000000000, 0.3750000000000000000, 0.3828125000000000000, 0.3906250000000000000, 0.3984375000000000000, 0.4062500000000000000, 0.4140625000000000000, 0.4218750000000000000, 0.4296875000000000000, 0.4375000000000000000, 0.4453125000000000000, 0.4531250000000000000, 0.4609375000000000000, 0.4687500000000000000, 0.4765625000000000000, 0.4843750000000000000, 0.4921875000000000000, 0.5000000000000000000, 0.5078125000000000000, 0.5156250000000000000, 0.5234375000000000000, 0.5312500000000000000, 0.5390625000000000000, 0.5468750000000000000, 0.5546875000000000000, 0.5625000000000000000, 0.5703125000000000000, 0.5781250000000000000, 0.5859375000000000000, 0.5937500000000000000, 0.6015625000000000000, 0.6093750000000000000, 0.6171875000000000000, 0.6250000000000000000, 0.6328125000000000000, 0.6406250000000000000, 0.6484375000000000000, 0.6562500000000000000, 0.6640625000000000000, 0.6718750000000000000, 0.6796875000000000000, 0.6875000000000000000, 0.6953125000000000000, 0.7031250000000000000, 0.7109375000000000000, 0.7187500000000000000, 0.7265625000000000000, 0.7343750000000000000, 0.7421875000000000000, 0.7500000000000000000, 0.7578125000000000000, 0.7656250000000000000, 0.7734375000000000000, 0.7812500000000000000, 0.7890625000000000000, 0.7968750000000000000, 0.8046875000000000000, 0.8125000000000000000, 0.8203125000000000000, 0.8281250000000000000, 0.8359375000000000000, 0.8437500000000000000, 0.8515625000000000000, 0.8593750000000000000, 0.8671875000000000000, 0.8750000000000000000, 0.8828125000000000000, 0.8906250000000000000, 0.8984375000000000000, 0.9062500000000000000, 0.9140625000000000000, 0.9218750000000000000, 0.9296875000000000000, 0.9375000000000000000, 0.9453125000000000000, 0.9531250000000000000, 0.9609375000000000000, 0.9687500000000000000, 0.9765625000000000000, 0.9843750000000000000, 0.9921875000000000000, 1.000000000000000000 ),
 .UNSPECIFIED. ) 
 GEOMETRIC_REPRESENTATION_ITEM ( )  RATIONAL_B_SPLINE_SURFACE ( (
 ( 1.000000000000000000, 0.9238795325112869605, 1.000000000000000000, 0.9238795325112869605, 1.000000000000000000, 0.9238795325112869605, 1.000000000000000000, 0.9238795325112869605, 1.000000000000000000, 0.9238795325112869605, 1.000000000000000000, 0.9238795325112869605, 1.000000000000000000, 0.9238795325112869605, 1.000000000000000000, 0.9238795325112869605, 1.000000000000000000, 0.9238795325112869605, 1.000000000000000000, 0.9238795325112869605, 1.000000000000000000, 0.9238795325112869605, 1.000000000000000000, 0.9238795325112869605, 1.000000000000000000, 0.9238795325112869605, 1.000000000000000000, 0.9238795325112869605, 1.000000000000000000, 0.9238795325112869605, 1.000000000000000000, 0.9238795325112869605, 1.000000000000000000, 0.9238795325112869605, 1.000000000000000000, 0.9238795325112869605, 1.000000000000000000, 0.9238795325112869605, 1.000000000000000000, 0.9238795325112869605, 1.000000000000000000, 0.9238795325112869605, 1.000000000000000000, 0.9238795325112869605, 1.000000000000000000, 0.9238795325112869605, 1.000000000000000000, 0.9238795325112869605, 1.000000000000000000, 0.9238795325112869605, 1.000000000000000000, 0.9238795325112869605, 1.000000000000000000, 0.9238795325112869605, 1.000000000000000000, 0.9238795325112869605, 1.000000000000000000, 0.9238795325112869605, 1.000000000000000000, 0.9238795325112869605, 1.000000000000000000, 0.9238795325112869605, 1.000000000000000000, 0.9238795325112869605, 1.000000000000000000, 0.9238795325112869605, 1.000000000000000000, 0.9238795325112869605, 1.000000000000000000, 0.9238795325112869605, 1.000000000000000000, 0.9238795325112869605, 1.000000000000000000, 0.9238795325112869605, 1.000000000000000000, 0.9238795325112869605, 1.000000000000000000, 0.9238795325112869605, 1.000000000000000000, 0.9238795325112869605, 1.000000000000000000, 0.9238795325112869605, 1.000000000000000000, 0.9238795325112869605, 1.000000000000000000, 0.9238795325112869605, 1.000000000000000000, 0.9238795325112869605, 1.000000000000000000, 0.9238795325112869605, 1.000000000000000000, 0.9238795325112869605, 1.000000000000000000, 0.9238795325112869605, 1.000000000000000000, 0.9238795325112869605, 1.000000000000000000, 0.9238795325112869605, 1.000000000000000000, 0.9238795325112869605, 1.000000000000000000, 0.9238795325112869605, 1.000000000000000000, 0.9238795325112869605, 1.000000000000000000, 0.9238795325112869605, 1.000000000000000000, 0.9238795325112869605, 1.000000000000000000, 0.9238795325112869605, 1.000000000000000000, 0.9238795325112869605, 1.000000000000000000, 0.9238795325112869605, 1.000000000000000000, 0.9238795325112869605, 1.000000000000000000, 0.9238795325112869605, 1.000000000000000000, 0.9238795325112869605, 1.000000000000000000, 0.9238795325112869605, 1.000000000000000000, 0.9238795325112869605, 1.000000000000000000, 0.9238795325112869605, 1.000000000000000000, 0.9238795325112869605, 1.000000000000000000, 0.9238795325112869605, 1.000000000000000000, 0.9238795325112869605, 1.000000000000000000, 0.9238795325112869605, 1.000000000000000000, 0.9238795325112869605, 1.000000000000000000, 0.9238795325112869605, 1.000000000000000000, 0.9238795325112869605, 1.000000000000000000, 0.9238795325112869605, 1.000000000000000000, 0.9238795325112869605, 1.000000000000000000, 0.9238795325112869605, 1.000000000000000000, 0.9238795325112869605, 1.000000000000000000, 0.9238795325112869605, 1.000000000000000000, 0.9238795325112869605, 1.000000000000000000, 0.9238795325112869605, 1.000000000000000000, 0.9238795325112869605, 1.000000000000000000, 0.9238795325112869605, 1.000000000000000000, 0.9238795325112869605, 1.000000000000000000, 0.9238795325112869605, 1.000000000000000000, 0.9238795325112869605, 1.000000000000000000, 0.9238795325112869605, 1.000000000000000000, 0.9238795325112869605, 1.000000000000000000, 0.9238795325112869605, 1.000000000000000000, 0.9238795325112869605, 1.000000000000000000, 0.9238795325112869605, 1.000000000000000000, 0.9238795325112869605, 1.000000000000000000, 0.9238795325112869605, 1.000000000000000000, 0.9238795325112869605, 1.000000000000000000, 0.9238795325112869605, 1.000000000000000000, 0.9238795325112869605, 1.000000000000000000, 0.9238795325112869605, 1.000000000000000000, 0.9238795325112869605, 1.000000000000000000, 0.9238795325112869605, 1.000000000000000000, 0.9238795325112869605, 1.000000000000000000, 0.9238795325112869605, 1.000000000000000000, 0.9238795325112869605, 1.000000000000000000, 0.9238795325112869605, 1.000000000000000000, 0.9238795325112869605, 1.000000000000000000, 0.9238795325112869605, 1.000000000000000000, 0.9238795325112869605, 1.000000000000000000, 0.9238795325112869605, 1.000000000000000000, 0.9238795325112869605, 1.000000000000000000, 0.9238795325112869605, 1.000000000000000000, 0.9238795325112869605, 1.000000000000000000, 0.9238795325112869605, 1.000000000000000000, 0.9238795325112869605, 1.000000000000000000, 0.9238795325112869605, 1.000000000000000000, 0.9238795325112869605, 1.000000000000000000, 0.9238795325112869605, 1.000000000000000000, 0.9238795325112869605, 1.000000000000000000, 0.9238795325112869605, 1.000000000000000000, 0.9238795325112869605, 1.000000000000000000, 0.9238795325112869605, 1.000000000000000000, 0.9238795325112869605, 1.000000000000000000, 0.9238795325112869605, 1.000000000000000000, 0.9238795325112869605, 1.000000000000000000, 0.9238795325112869605, 1.000000000000000000, 0.9238795325112869605, 1.000000000000000000, 0.9238795325112869605, 1.000000000000000000, 0.9238795325112869605, 1.000000000000000000, 0.9238795325112869605, 1.000000000000000000, 0.9238795325112869605, 1.000000000000000000, 0.9238795325112869605, 1.000000000000000000, 0.9238795325112869605, 1.000000000000000000, 0.9238795325112869605, 1.000000000000000000, 0.9238795325112869605, 1.000000000000000000),
 ( 1.000000000000000000, 0.9238795325112869605, 1.000000000000000000, 0.9238795325112869605, 1.000000000000000000, 0.9238795325112869605, 1.000000000000000000, 0.9238795325112869605, 1.000000000000000000, 0.9238795325112869605, 1.000000000000000000, 0.9238795325112869605, 1.000000000000000000, 0.9238795325112869605, 1.000000000000000000, 0.9238795325112869605, 1.000000000000000000, 0.9238795325112869605, 1.000000000000000000, 0.9238795325112869605, 1.000000000000000000, 0.9238795325112869605, 1.000000000000000000, 0.9238795325112869605, 1.000000000000000000, 0.9238795325112869605, 1.000000000000000000, 0.9238795325112869605, 1.000000000000000000, 0.9238795325112869605, 1.000000000000000000, 0.9238795325112869605, 1.000000000000000000, 0.9238795325112869605, 1.000000000000000000, 0.9238795325112869605, 1.000000000000000000, 0.9238795325112869605, 1.000000000000000000, 0.9238795325112869605, 1.000000000000000000, 0.9238795325112869605, 1.000000000000000000, 0.9238795325112869605, 1.000000000000000000, 0.9238795325112869605, 1.000000000000000000, 0.9238795325112869605, 1.000000000000000000, 0.9238795325112869605, 1.000000000000000000, 0.9238795325112869605, 1.000000000000000000, 0.9238795325112869605, 1.000000000000000000, 0.9238795325112869605, 1.000000000000000000, 0.9238795325112869605, 1.000000000000000000, 0.9238795325112869605, 1.000000000000000000, 0.9238795325112869605, 1.000000000000000000, 0.9238795325112869605, 1.000000000000000000, 0.9238795325112869605, 1.000000000000000000, 0.9238795325112869605, 1.000000000000000000, 0.9238795325112869605, 1.000000000000000000, 0.9238795325112869605, 1.000000000000000000, 0.9238795325112869605, 1.000000000000000000, 0.9238795325112869605, 1.000000000000000000, 0.9238795325112869605, 1.000000000000000000, 0.9238795325112869605, 1.000000000000000000, 0.9238795325112869605, 1.000000000000000000, 0.9238795325112869605, 1.000000000000000000, 0.9238795325112869605, 1.000000000000000000, 0.9238795325112869605, 1.000000000000000000, 0.9238795325112869605, 1.000000000000000000, 0.9238795325112869605, 1.000000000000000000, 0.9238795325112869605, 1.000000000000000000, 0.9238795325112869605, 1.000000000000000000, 0.9238795325112869605, 1.000000000000000000, 0.9238795325112869605, 1.000000000000000000, 0.9238795325112869605, 1.000000000000000000, 0.9238795325112869605, 1.000000000000000000, 0.9238795325112869605, 1.000000000000000000, 0.9238795325112869605, 1.000000000000000000, 0.9238795325112869605, 1.000000000000000000, 0.9238795325112869605, 1.000000000000000000, 0.9238795325112869605, 1.000000000000000000, 0.9238795325112869605, 1.000000000000000000, 0.9238795325112869605, 1.000000000000000000, 0.9238795325112869605, 1.000000000000000000, 0.9238795325112869605, 1.000000000000000000, 0.9238795325112869605, 1.000000000000000000, 0.9238795325112869605, 1.000000000000000000, 0.9238795325112869605, 1.000000000000000000, 0.9238795325112869605, 1.000000000000000000, 0.9238795325112869605, 1.000000000000000000, 0.9238795325112869605, 1.000000000000000000, 0.9238795325112869605, 1.000000000000000000, 0.9238795325112869605, 1.000000000000000000, 0.9238795325112869605, 1.000000000000000000, 0.9238795325112869605, 1.000000000000000000, 0.9238795325112869605, 1.000000000000000000, 0.9238795325112869605, 1.000000000000000000, 0.9238795325112869605, 1.000000000000000000, 0.9238795325112869605, 1.000000000000000000, 0.9238795325112869605, 1.000000000000000000, 0.9238795325112869605, 1.000000000000000000, 0.9238795325112869605, 1.000000000000000000, 0.9238795325112869605, 1.000000000000000000, 0.9238795325112869605, 1.000000000000000000, 0.9238795325112869605, 1.000000000000000000, 0.9238795325112869605, 1.000000000000000000, 0.9238795325112869605, 1.000000000000000000, 0.9238795325112869605, 1.000000000000000000, 0.9238795325112869605, 1.000000000000000000, 0.9238795325112869605, 1.000000000000000000, 0.9238795325112869605, 1.000000000000000000, 0.9238795325112869605, 1.000000000000000000, 0.9238795325112869605, 1.000000000000000000, 0.9238795325112869605, 1.000000000000000000, 0.9238795325112869605, 1.000000000000000000, 0.9238795325112869605, 1.000000000000000000, 0.9238795325112869605, 1.000000000000000000, 0.9238795325112869605, 1.000000000000000000, 0.9238795325112869605, 1.000000000000000000, 0.9238795325112869605, 1.000000000000000000, 0.9238795325112869605, 1.000000000000000000, 0.9238795325112869605, 1.000000000000000000, 0.9238795325112869605, 1.000000000000000000, 0.9238795325112869605, 1.000000000000000000, 0.9238795325112869605, 1.000000000000000000, 0.9238795325112869605, 1.000000000000000000, 0.9238795325112869605, 1.000000000000000000, 0.9238795325112869605, 1.000000000000000000, 0.9238795325112869605, 1.000000000000000000, 0.9238795325112869605, 1.000000000000000000, 0.9238795325112869605, 1.000000000000000000, 0.9238795325112869605, 1.000000000000000000, 0.9238795325112869605, 1.000000000000000000, 0.9238795325112869605, 1.000000000000000000, 0.9238795325112869605, 1.000000000000000000, 0.9238795325112869605, 1.000000000000000000, 0.9238795325112869605, 1.000000000000000000, 0.9238795325112869605, 1.000000000000000000, 0.9238795325112869605, 1.000000000000000000, 0.9238795325112869605, 1.000000000000000000, 0.9238795325112869605, 1.000000000000000000, 0.9238795325112869605, 1.000000000000000000, 0.9238795325112869605, 1.000000000000000000, 0.9238795325112869605, 1.000000000000000000, 0.9238795325112869605, 1.000000000000000000, 0.9238795325112869605, 1.000000000000000000, 0.9238795325112869605, 1.000000000000000000, 0.9238795325112869605, 1.000000000000000000, 0.9238795325112869605, 1.000000000000000000, 0.9238795325112869605, 1.000000000000000000, 0.9238795325112869605, 1.000000000000000000, 0.9238795325112869605, 1.000000000000000000) ) ) 
 REPRESENTATION_ITEM ( '' )  SURFACE ( )  );
#34281 = DIRECTION ( 'NONE',  ( 1.000000000000000000, 0.000000000000000000, 0.000000000000000000 ) ) ;
#34282 = CARTESIAN_POINT ( 'NONE',  ( 119.9518141859119851, -0.8832429491016019485, -18.19431474523657855 ) ) ;
#34283 = VERTEX_POINT ( 'NONE', #18833 ) ;
#34284 = CARTESIAN_POINT ( 'NONE',  ( 59.92024162955041788, -14.76985142791843053, -8.596615743543749133 ) ) ;
#34285 = CARTESIAN_POINT ( 'NONE',  ( 125.1433143116089894, 1.889641906327490073, -10.28863673848242577 ) ) ;
#34286 = CARTESIAN_POINT ( 'NONE',  ( 114.3024890045248156, 0.8980012041604421569, -15.77991374673208469 ) ) ;
#34287 = AXIS2_PLACEMENT_3D ( 'NONE', #40447, #8, #10504 ) ;
#34288 = AXIS2_PLACEMENT_3D ( 'NONE', #8664, #5911, #33034 ) ;
#34289 = CARTESIAN_POINT ( 'NONE',  ( 123.4041481442452834, 0.1319031606808879209, -14.10382304977623669 ) ) ;
#34290 = CARTESIAN_POINT ( 'NONE',  ( 112.5126281442453120, 0.1319031606808879209, -14.10382304977623669 ) ) ;
#34291 = CARTESIAN_POINT ( 'NONE',  ( 128.2184548109119930, 0.7167481258041193959, -11.18974888642105014 ) ) ;
#34292 = ORIENTED_EDGE ( 'NONE', *, *, #31738, .T. ) ;
#34293 = CARTESIAN_POINT ( 'NONE',  ( 96.54708369096698561, -28.17862604940189541, -13.73821557025528683 ) ) ;
#34294 = CARTESIAN_POINT ( 'NONE',  ( 69.69189222814998175, -41.76310523276723785, -20.39321520033831447 ) ) ;
#34295 = CARTESIAN_POINT ( 'NONE',  ( 112.4272546295247821, -4.863998795839590272, -7.631215200338315796 ) ) ;
#34296 = CARTESIAN_POINT ( 'NONE',  ( 111.9559014775786494, -9.522524984348097021, -10.63868154973201108 ) ) ;
#34298 = CARTESIAN_POINT ( 'NONE',  ( 125.3328548109119964, -9.261995988541697145, -16.69588392320189030 ) ) ;
#34297 = CARTESIAN_POINT ( 'NONE',  ( 65.15858969855669613, -37.34466124008154253, -5.220056341859305782 ) ) ;
#34299 = CARTESIAN_POINT ( 'NONE',  ( 111.8319081442453182, -5.638512984488999180, -18.83840828888717311 ) ) ;
#34300 = ORIENTED_EDGE ( 'NONE', *, *, #35612, .F. ) ;
#34301 = CARTESIAN_POINT ( 'NONE',  ( 114.6115148109119986, -3.383040157471821630, -19.15922257007629170 ) ) ;
#34302 = CARTESIAN_POINT ( 'NONE',  ( 113.4001635400977790, -1.223627541775725636, -16.99192386690445034 ) ) ;
#34303 = CARTESIAN_POINT ( 'NONE',  ( 115.4137390045248566, 0.8980012041604421569, -15.77991374673208469 ) ) ;
#34304 = ADVANCED_FACE ( 'NONE', ( #26581 ), #43448, .T. ) ;
#34305 = CARTESIAN_POINT ( 'NONE',  ( 123.8012348109119642, -9.565557343593413364, -10.61323700422348004 ) ) ;
#34306 = CARTESIAN_POINT ( 'NONE',  ( 122.8936081442453059, -9.565557343593413364, -10.61323700422348004 ) ) ;
#34307 = CARTESIAN_POINT ( 'NONE',  ( 70.19189222814998175, -100.0979043305785581, -53.24182196210380624 ) ) ;
#34308 = CARTESIAN_POINT ( 'NONE',  ( 105.8292077545248446, -7.250697342233347165, -7.631215200338321125 ) ) ;
#34309 = DIRECTION ( 'NONE',  ( 0.9609149988134843001, -0.1028163501681632064, 0.2570431154366505933 ) ) ;
#34310 = CARTESIAN_POINT ( 'NONE',  ( 63.02947104699595116, -32.17731879514034432, -23.89321520033831447 ) ) ;
#34311 = AXIS2_PLACEMENT_3D ( 'NONE', #17118, #23961, #27818 ) ;
#34312 = CARTESIAN_POINT ( 'NONE',  ( 108.1211608795247798, -8.938348069036489818, -9.318865927141430916 ) ) ;
#34313 = DIRECTION ( 'NONE',  ( 0.000000000000000000, 0.4669533266896289669, 0.8842819633428518067 ) ) ;
#34314 = CARTESIAN_POINT ( 'NONE',  ( 112.1494421295248003, 0.8980012041604618078, -13.39321520033831447 ) ) ;
#34315 = CARTESIAN_POINT ( 'NONE',  ( 124.0848681442452772, -4.089484607189486809, -7.948022111789456723 ) ) ;
#34316 = CARTESIAN_POINT ( 'NONE',  ( 111.7184548109119788, -0.8288870151387760510, -10.36305467784173118 ) ) ;
#34317 = LINE ( 'NONE', #41188, #37173 ) ;
#34318 = CARTESIAN_POINT ( 'NONE',  ( 120.6812681442452941, -10.30919188438810075, -12.61870101168855918 ) ) ;
#34319 = CARTESIAN_POINT ( 'NONE',  ( 113.4202548109119846, -10.30919188438810075, -12.61870101168855918 ) ) ;
#34320 = ORIENTED_EDGE ( 'NONE', *, *, #20879, .T. ) ;
#34321 = CARTESIAN_POINT ( 'NONE',  ( 114.2144281442453178, -1.833838273342658809, -17.42832698103878286 ) ) ;
#34322 = CARTESIAN_POINT ( 'NONE',  ( 125.6732148109119862, 0.5811942927096110934, -14.16772938898807510 ) ) ;
#34323 = AXIS2_PLACEMENT_3D ( 'NONE', #5983, #17171, #31060 ) ;
#34324 = CARTESIAN_POINT ( 'NONE',  ( 123.9146881442452894, 0.9020085738987339008, -11.91225656197089222 ) ) ;
#34325 = CARTESIAN_POINT ( 'NONE',  ( 113.2500748109119968, -6.344957434206662583, -7.627207830600332805 ) ) ;
#34326 = CARTESIAN_POINT ( 'NONE',  ( 113.5337081442453240, -0.8288870151387760510, -10.36305467784173118 ) ) ;
#34327 = ORIENTED_EDGE ( 'NONE', *, *, #43419, .F. ) ;
#34328 = EDGE_CURVE ( 'NONE', #34005, #21889, #39834, .T. ) ;
#34329 = CARTESIAN_POINT ( 'NONE',  ( 116.1998614775786507, 0.4262465694468514643, -12.03445270309931736 ) ) ;
#34330 = CARTESIAN_POINT ( 'NONE',  ( 111.7184548109119788, -9.261995988541697145, -16.69588392320189030 ) ) ;
#34331 = CARTESIAN_POINT ( 'NONE',  ( 125.2194014775786286, 0.1319031606808879209, -14.10382304977623669 ) ) ;
#34332 = CARTESIAN_POINT ( 'NONE',  ( 116.8308172556448596, -1.389150239195028114, -17.31318354165465578 ) ) ;
#34333 = CARTESIAN_POINT ( 'NONE',  ( 114.4413952545248350, 0.8980012041604421569, -11.00651665394454071 ) ) ;
#34334 = ORIENTED_EDGE ( 'NONE', *, *, #18597, .T. ) ;
#34335 = DIRECTION ( 'NONE',  ( 0.9609149988134837450, -0.1028163501681639419, 0.2570431154366518145 ) ) ;
#34336 = CARTESIAN_POINT ( 'NONE',  ( 68.14371629974728251, -1.351251493923715685, -10.39321520033831625 ) ) ;
#34337 = CARTESIAN_POINT ( 'NONE',  ( 88.07785292173620917, -25.99489077589524300, -13.39321520033831625 ) ) ;
#34338 = CARTESIAN_POINT ( 'NONE',  ( 115.1430393777725385, -1.267766418764730840, -16.93314635290706605 ) ) ;
#34339 = CARTESIAN_POINT ( 'NONE',  ( 116.4392337193178975, 2.230983512441839345, -6.373539596108586558 ) ) ;
#34340 = CARTESIAN_POINT ( 'NONE',  ( 61.69189222814998175, -40.21211973637273474, -23.89321520033831803 ) ) ;
#34341 = CARTESIAN_POINT ( 'NONE',  ( 108.6073327545248048, -6.936859964151250502, -8.388885654883777576 ) ) ;
#34342 = CARTESIAN_POINT ( 'NONE',  ( 95.62170725701128049, -26.77595362744983376, -12.85143736872905507 ) ) ;
#34343 = CARTESIAN_POINT ( 'NONE',  ( 119.9438214775786378, -7.893985811506177619, -18.51759400769804742 ) ) ;
#34344 = CARTESIAN_POINT ( 'NONE',  ( 137.0337503232511267, -6.699180850412786548, -18.51269755244290494 ) ) ;
#34345 = FACE_OUTER_BOUND ( 'NONE', #29335, .T. ) ;
#34346 = DIRECTION ( 'NONE',  ( 0.9609149988134837450, -0.1028163501681639419, 0.2570431154366518145 ) ) ;
#34347 = CARTESIAN_POINT ( 'NONE',  ( 120.3409081442453044, -8.899110576539710493, -16.42337572283490132 ) ) ;
#34348 = ORIENTED_EDGE ( 'NONE', *, *, #43308, .T. ) ;
#34349 = CARTESIAN_POINT ( 'NONE',  ( 126.2404814775786264, -9.261995988541697145, -16.69588392320189030 ) ) ;
#34350 = CARTESIAN_POINT ( 'NONE',  ( 118.7525614775786380, -8.166667518702819706, -8.995218007635861213 ) ) ;
#34351 = DIRECTION ( 'NONE',  ( 0.000000000000000000, -0.3818493186865936084, 0.9242245927363024194 ) ) ;
#34352 = CARTESIAN_POINT ( 'NONE',  ( 115.8595014775786609, -7.643976991954077427, -18.09477374809248928 ) ) ;
#34353 = CARTESIAN_POINT ( 'NONE',  ( 112.2857214775786474, -5.574606645277164318, -18.38911715685844683 ) ) ;
#34354 = CARTESIAN_POINT ( 'NONE',  ( 110.0658483795247804, -0.7896495226426338832, -9.318865927141430916 ) ) ;
#34355 = CARTESIAN_POINT ( 'NONE',  ( 106.3848327545248651, -6.936859964151250502, -8.388885654883777576 ) ) ;
#34356 = CARTESIAN_POINT ( 'NONE',  ( 115.3442858795247759, -0.7896495226426338832, -17.46756447353520159 ) ) ;
#34357 = CARTESIAN_POINT ( 'NONE',  ( 118.0718414775786442, -0.8288870151387760510, -10.36305467784173118 ) ) ;
#34358 = CARTESIAN_POINT ( 'NONE',  ( 119.6034614775786196, -3.505236298600246325, -18.68346056562440793 ) ) ;
#34359 = CARTESIAN_POINT ( 'NONE',  ( 109.2294426289140858, -7.739168762018897141, -8.465928987177235854 ) ) ;
#34360 = CARTESIAN_POINT ( 'NONE',  ( 121.6186891859119896, -8.844754642576884152, -8.592115655440050404 ) ) ;
#34361 = CARTESIAN_POINT ( 'NONE',  ( 110.2742077545248094, -2.791137627527939813, -18.39754474579286025 ) ) ;
#34362 = ORIENTED_EDGE ( 'NONE', *, *, #13627, .T. ) ;
#34363 = CYLINDRICAL_SURFACE ( 'NONE', #10928, 4.999999999999998224 ) ;
#34364 = CARTESIAN_POINT ( 'NONE',  ( 115.4056881442453459, -7.893985811506177619, -18.51759400769804742 ) ) ;
#34365 = CARTESIAN_POINT ( 'NONE',  ( 111.7751814775786556, -7.893985811506177619, -18.51759400769804742 ) ) ;
#34366 = DIRECTION ( 'NONE',  ( 0.000000000000000000, -0.3818493186865927203, 0.9242245927363029745 ) ) ;
#34367 = CARTESIAN_POINT ( 'NONE',  ( 122.0354079359119908, -4.360204210389833968, -8.000047426360245240 ) ) ;
#34368 = EDGE_LOOP ( 'NONE', ( #38096, #38043, #41066, #37126, #41702 ) ) ;
#34369 = CARTESIAN_POINT ( 'NONE',  ( 113.6774108795247997, -8.938348069036441856, -9.318865927141430916 ) ) ;
#34370 = ORIENTED_EDGE ( 'NONE', *, *, #36438, .T. ) ;
#34371 = CARTESIAN_POINT ( 'NONE',  ( 120.8514481442452961, -7.893985811506177619, -18.51759400769804742 ) ) ;
#34372 = AXIS2_PLACEMENT_3D ( 'NONE', #44077, #20132, #26961 ) ;
#34373 = CARTESIAN_POINT ( 'NONE',  ( 114.2144281442453178, -8.166667518702817929, -8.995218007635859436 ) ) ;
#34374 = ADVANCED_FACE ( 'NONE', ( #32506 ), #32945, .F. ) ;
#34375 = CARTESIAN_POINT ( 'NONE',  ( 118.5823814775786360, -7.643976991954077427, -18.09477374809248928 ) ) ;
#34376 = CARTESIAN_POINT ( 'NONE',  ( 122.6009548109119720, -8.523281198020143279, -6.279169073056789507 ) ) ;
#34377 = CARTESIAN_POINT ( 'NONE',  ( 120.4543614775786295, -4.089484607189486809, -7.948022111789456723 ) ) ;
#34378 = CARTESIAN_POINT ( 'NONE',  ( 118.5256548109119876, -0.4660016031367893996, -10.09054647747474043 ) ) ;
#34379 = CARTESIAN_POINT ( 'NONE',  ( 116.4555358795247884, -0.7896495226426338832, -17.46756447353520159 ) ) ;
#34380 = CARTESIAN_POINT ( 'NONE',  ( 111.4348214775786801, -3.505236298600246325, -18.68346056562440793 ) ) ;
#34381 = CARTESIAN_POINT ( 'NONE',  ( 115.9294421295247872, 1.035107641088057973, -12.14321520033831625 ) ) ;
#34382 = ORIENTED_EDGE ( 'NONE', *, *, #10274, .T. ) ;
#34383 = CARTESIAN_POINT ( 'NONE',  ( 118.9794681442453026, -9.261995988541697145, -16.69588392320189030 ) ) ;
#34384 = CARTESIAN_POINT ( 'NONE',  ( 120.0212673109119805, 0.2312338769422704887, -16.08380026872395874 ) ) ;
#34385 = CARTESIAN_POINT ( 'NONE',  ( 114.5547881442453217, -5.638512984488999180, -18.83840828888717311 ) ) ;
#34386 = ORIENTED_EDGE ( 'NONE', *, *, #18923, .T. ) ;
#34387 = CARTESIAN_POINT ( 'NONE',  ( 125.4463081442452932, -5.638512984488999180, -18.83840828888717311 ) ) ;
#34388 = EDGE_CURVE ( 'NONE', #29815, #38024, #23056, .T. ) ;
#34389 = FACE_OUTER_BOUND ( 'NONE', #16631, .T. ) ;
#34390 = CARTESIAN_POINT ( 'NONE',  ( 112.4559014775786778, -0.1624402480850797581, -16.17319339645315424 ) ) ;
#34391 = DIRECTION ( 'NONE',  ( 0.9908103287288504424, -0.1352586133457950590, 0.000000000000000000 ) ) ;
#34392 = CARTESIAN_POINT ( 'NONE',  ( 116.1431348109119881, 0.1319031606808879209, -14.10382304977623669 ) ) ;
#34393 = DIRECTION ( 'NONE',  ( 0.000000000000000000, 0.000000000000000000, -1.000000000000000000 ) ) ;
#34394 = CARTESIAN_POINT ( 'NONE',  ( 117.9016614775786280, -0.1624402480850797581, -16.17319339645315424 ) ) ;
#34395 = CIRCLE ( 'NONE', #4527, 6.500000000000000000 ) ;
#34396 = FACE_BOUND ( 'NONE', #32169, .T. ) ;
#34397 = CARTESIAN_POINT ( 'NONE',  ( 116.3700414775786527, -4.153390946401321671, -8.397313243818183892 ) ) ;
#34398 = CARTESIAN_POINT ( 'NONE',  ( 123.2161110609119561, -3.163656168406935087, -18.89861972220014508 ) ) ;
#34399 = CARTESIAN_POINT ( 'NONE',  ( 115.6893214775786447, 0.5811942927096154232, -14.16772938898807155 ) ) ;
#34400 = CARTESIAN_POINT ( 'NONE',  ( 125.6732148109119862, 0.5811942927096110934, -14.16772938898807510 ) ) ;
#34401 = CARTESIAN_POINT ( 'NONE',  ( 118.4122014775786340, -9.859900752359374465, -12.68260735090039404 ) ) ;
#34402 = VERTEX_POINT ( 'NONE', #27715 ) ;
#34403 = CARTESIAN_POINT ( 'NONE',  ( 116.7671281442453335, -1.834011780172310813, -8.268836392978581529 ) ) ;
#34404 = CARTESIAN_POINT ( 'NONE',  ( 105.9681140045248355, -10.62599879583958717, -11.00651665394454604 ) ) ;
#34405 = CARTESIAN_POINT ( 'NONE',  ( 106.4542858795248179, -8.402594152722688392, -9.854619843455216355 ) ) ;
#34406 = AXIS2_PLACEMENT_3D ( 'NONE', #33592, #19262, #26327 ) ;
#34407 = FACE_OUTER_BOUND ( 'NONE', #30064, .T. ) ;
#34408 = CARTESIAN_POINT ( 'NONE',  ( 64.08498584890432426, -35.21828807897666991, -5.893215200338318915 ) ) ;
#34409 = CARTESIAN_POINT ( 'NONE',  ( 123.5176014775786228, -9.261995988541697145, -16.69588392320189030 ) ) ;
#34410 = EDGE_LOOP ( 'NONE', ( #26592, #8095, #16794, #38193, #39275, #28828, #14850, #34463, #11689, #41313, #42873 ) ) ;
#34411 = DIRECTION ( 'NONE',  ( 0.000000000000000000, 0.000000000000000000, 1.000000000000000000 ) ) ;
#34412 = CARTESIAN_POINT ( 'NONE',  ( 118.1285681442453068, -2.084020599724406786, -8.691656652584148546 ) ) ;
#34413 = CARTESIAN_POINT ( 'NONE',  ( 127.8924691488521574, 0.9350681874800557125, -12.72727887896535925 ) ) ;
#34414 = CARTESIAN_POINT ( 'NONE',  ( 123.0070614775786169, 0.9020085738987339008, -11.91225656197089222 ) ) ;
#34415 = CARTESIAN_POINT ( 'NONE',  ( 107.7738952545248310, 0.8980012041604421569, -11.00651665394454071 ) ) ;
#34416 = CARTESIAN_POINT ( 'NONE',  ( 89.24253794056055256, -10.10023911675148334, -13.82618190763190036 ) ) ;
#34417 = EDGE_LOOP ( 'NONE', ( #19754, #5184, #22107, #28688 ) ) ;
#34418 = CARTESIAN_POINT ( 'NONE',  ( 111.8319081442453182, -5.638512984488999180, -18.83840828888717311 ) ) ;
#34419 = CARTESIAN_POINT ( 'NONE',  ( 111.7184548109119788, -9.261995988541697145, -16.69588392320189030 ) ) ;
#34420 = CARTESIAN_POINT ( 'NONE',  ( 122.5532481442453019, -10.63000616557722466, -14.87417383870573495 ) ) ;
#34421 = CARTESIAN_POINT ( 'NONE',  ( 116.9940348109119839, -0.1624402480850797581, -16.17319339645315424 ) ) ;
#34422 = FACE_OUTER_BOUND ( 'NONE', #9590, .T. ) ;
#34423 = CARTESIAN_POINT ( 'NONE',  ( 119.4900081442453086, -1.834011780172310813, -8.268836392978581529 ) ) ;
#34424 = CARTESIAN_POINT ( 'NONE',  ( 94.20708369096698220, -25.26022072204669655, -13.82270432939535709 ) ) ;
#34425 = CARTESIAN_POINT ( 'NONE',  ( 126.3115243456358883, -1.057789078141782690, -10.07954330274492882 ) ) ;
#34426 = CARTESIAN_POINT ( 'NONE',  ( 124.0848681442452772, -5.574606645277164318, -18.38911715685844683 ) ) ;
#34427 = EDGE_LOOP ( 'NONE', ( #18217, #22287, #37251, #16981 ) ) ;
#34428 = AXIS2_PLACEMENT_3D ( 'NONE', #37400, #5935, #2516 ) ;
#34429 = DIRECTION ( 'NONE',  ( 0.5040994586965589219, 0.8636456077245088236, 0.000000000000000000 ) ) ;
#34430 = CONICAL_SURFACE ( 'NONE', #43169, 2.445500000000005336, 0.9599310885968757034 ) ;
#34431 = CARTESIAN_POINT ( 'NONE',  ( 118.0151148109119816, -10.63000616557722466, -14.87417383870573495 ) ) ;
#34432 = CARTESIAN_POINT ( 'NONE',  ( 124.8790414775786246, -8.899110576539710493, -16.42337572283490132 ) ) ;
#34433 = ORIENTED_EDGE ( 'NONE', *, *, #40083, .F. ) ;
#34434 = CARTESIAN_POINT ( 'NONE',  ( 121.1325173109119788, 0.2312338769422704887, -16.08380026872395874 ) ) ;
#34435 = CARTESIAN_POINT ( 'NONE',  ( 59.44377208703740223, -12.82110557137145967, -9.393546723914594665 ) ) ;
#34436 = CARTESIAN_POINT ( 'NONE',  ( 123.8012348109119642, 0.2603800115204892296, -16.42320221600525088 ) ) ;
#34437 = CARTESIAN_POINT ( 'NONE',  ( 109.8574890045247940, 0.8980012041604421569, -15.77991374673208469 ) ) ;
#34438 = CARTESIAN_POINT ( 'NONE',  ( 119.2063748109119814, -7.894159318335828068, -9.358103419637847864 ) ) ;
#34439 = ORIENTED_EDGE ( 'NONE', *, *, #6657, .T. ) ;
#34440 = EDGE_LOOP ( 'NONE', ( #37152, #32584, #34382, #10349 ) ) ;
#34441 = CARTESIAN_POINT ( 'NONE',  ( 114.9518748109119883, -1.834011780172310813, -8.268836392978581529 ) ) ;
#34442 = CARTESIAN_POINT ( 'NONE',  ( 124.3117748109119844, 0.1319031606808879209, -14.10382304977623669 ) ) ;
#34443 = PLANE ( 'NONE',  #20769 ) ;
#34444 = DIRECTION ( 'NONE',  ( 1.000000000000000000, 0.000000000000000000, 0.000000000000000000 ) ) ;
#34445 = CARTESIAN_POINT ( 'NONE',  ( 122.0994348109119443, 0.9020085738987339008, -11.91225656197089222 ) ) ;
#34446 = CARTESIAN_POINT ( 'NONE',  ( 111.4159584094731059, -9.013377521824503802, -16.52270977695948417 ) ) ;
#34447 = CARTESIAN_POINT ( 'NONE',  ( 87.14323352029596492, -26.75858941326842810, -11.54476601486570964 ) ) ;
#34448 = CARTESIAN_POINT ( 'NONE',  ( 121.4187148109119789, -6.344957434206665248, -7.627207830600338134 ) ) ;
#34450 = CARTESIAN_POINT ( 'NONE',  ( 119.3198281442452924, -9.859900752359374465, -12.68260735090039404 ) ) ;
#34449 = CARTESIAN_POINT ( 'NONE',  ( 118.4122014775786340, 0.5811942927096110934, -14.16772938898807510 ) ) ;
#34451 = CARTESIAN_POINT ( 'NONE',  ( 68.92755183904094451, -25.82220866885473853, -5.893215200338315363 ) ) ;
#34452 = CARTESIAN_POINT ( 'NONE',  ( 116.7671281442453335, -1.834011780172310813, -8.268836392978581529 ) ) ;
#34453 = EDGE_CURVE ( 'NONE', #25646, #32564, #20139, .T. ) ;
#34454 = ORIENTED_EDGE ( 'NONE', *, *, #41214, .T. ) ;
#34455 = CARTESIAN_POINT ( 'NONE',  ( 126.5808414775786446, -9.859900752359378018, -12.68260735090039759 ) ) ;
#34456 = CIRCLE ( 'NONE', #35922, 1.610000000000000986 ) ;
#34457 = CARTESIAN_POINT ( 'NONE',  ( 125.6626748109119802, -9.522524984348629928, -10.63868154973292413 ) ) ;
#34458 = CARTESIAN_POINT ( 'NONE',  ( 106.3153796295248412, -4.863998795839590272, -19.15521520033831493 ) ) ;
#34459 = CARTESIAN_POINT ( 'NONE',  ( 107.1488171295247867, 0.1403307496149613920, -13.39321520033831447 ) ) ;
#34460 = CARTESIAN_POINT ( 'NONE',  ( 106.1070202545248407, -10.62599879583958717, -15.77991374673208469 ) ) ;
#34461 = CARTESIAN_POINT ( 'NONE',  ( 121.5321681442453183, -9.988377603198976828, -10.36322818467138340 ) ) ;
#34462 = CARTESIAN_POINT ( 'NONE',  ( 122.1561614775786353, -8.899110576539710493, -16.42337572283490132 ) ) ;
#34463 = ORIENTED_EDGE ( 'NONE', *, *, #28759, .F. ) ;
#34464 = CARTESIAN_POINT ( 'NONE',  ( 123.7445081442452874, -1.561330072975668948, -17.79121239304076951 ) ) ;
#34465 = CARTESIAN_POINT ( 'NONE',  ( 113.0523327545247838, -2.477300249445798297, -19.15521520033831138 ) ) ;
#34466 = DIRECTION ( 'NONE',  ( 1.000000000000000000, 0.000000000000000000, 0.000000000000000000 ) ) ;
#34467 = CARTESIAN_POINT ( 'NONE',  ( 125.1626748109119802, -9.988377603198980381, -10.36322818467138518 ) ) ;
#34468 = PLANE ( 'NONE',  #21148 ) ;
#34469 = CARTESIAN_POINT ( 'NONE',  ( 119.8129079359119942, -4.360204210389833968, -8.000047426360245240 ) ) ;
#34470 = CARTESIAN_POINT ( 'NONE',  ( 114.0442481442453300, -1.834011780172310813, -8.268836392978581529 ) ) ;
#34471 = CARTESIAN_POINT ( 'NONE',  ( 122.8688454359119646, 0.5291689781388270175, -13.89700978578772705 ) ) ;
#34472 = CARTESIAN_POINT ( 'NONE',  ( 107.2877233795247776, -8.938348069036489818, -17.46756447353520159 ) ) ;
#34473 = EDGE_LOOP ( 'NONE', ( #5246, #27145, #20280, #14368, #17432 ) ) ;
#34474 = CIRCLE ( 'NONE', #39564, 7.132259260909268761 ) ;
#34475 = CYLINDRICAL_SURFACE ( 'NONE', #15024, 1.499999999999999556 ) ;
#34476 = CARTESIAN_POINT ( 'NONE',  ( 112.6260814775786514, -0.8288870151387760510, -10.36305467784173118 ) ) ;
#34477 = CARTESIAN_POINT ( 'NONE',  ( 112.2857214775786474, -4.089484607189486809, -7.948022111789456723 ) ) ;
#34478 = CARTESIAN_POINT ( 'NONE',  ( 107.2182702545248105, 0.1403307496149616695, -11.32035403202665336 ) ) ;
#34479 = CARTESIAN_POINT ( 'NONE',  ( 105.8986608795248401, -1.325403438956436419, -16.93181055722141792 ) ) ;
#34480 = CARTESIAN_POINT ( 'NONE',  ( 122.4965214775786251, 0.1319031606808879209, -14.10382304977623669 ) ) ;
#34481 = CARTESIAN_POINT ( 'NONE',  ( 114.5547881442453217, -4.153390946401321671, -8.397313243818183892 ) ) ;
#34482 = CARTESIAN_POINT ( 'NONE',  ( 113.7038881442453402, -6.222761293078241884, -8.102969835052219238 ) ) ;
#34483 = VERTEX_POINT ( 'NONE', #27491 ) ;
#34484 = EDGE_CURVE ( 'NONE', #29964, #36610, #6741, .T. ) ;
#34485 = CARTESIAN_POINT ( 'NONE',  ( 124.9357681442453014, -7.643976991954077427, -18.09477374809248928 ) ) ;
#34486 = CARTESIAN_POINT ( 'NONE',  ( 119.3198281442452924, 0.5811942927096110934, -14.16772938898807510 ) ) ;
#34487 = CARTESIAN_POINT ( 'NONE',  ( 125.7866681442452688, -8.899110576539710493, -16.42337572283490132 ) ) ;
#34488 = CARTESIAN_POINT ( 'NONE',  ( 115.4624148109119943, -4.153390946401321671, -8.397313243818183892 ) ) ;
#34489 = ORIENTED_EDGE ( 'NONE', *, *, #21102, .T. ) ;
#34490 = CARTESIAN_POINT ( 'NONE',  ( 126.9276200068663343, -9.666589674469316051, -15.76113967148663697 ) ) ;
#34491 = EDGE_CURVE ( 'NONE', #1665, #2964, #16325, .T. ) ;
#34492 = EDGE_CURVE ( 'NONE', #3445, #27212, #1206, .T. ) ;
#34493 = ORIENTED_EDGE ( 'NONE', *, *, #12568, .F. ) ;
#34494 = CARTESIAN_POINT ( 'NONE',  ( 115.2355081442453155, 0.1319031606808879209, -14.10382304977623669 ) ) ;
#34495 = CARTESIAN_POINT ( 'NONE',  ( 114.9518748109119883, -7.643976991954077427, -18.09477374809248928 ) ) ;
#34496 = CARTESIAN_POINT ( 'NONE',  ( 115.2355081442453155, -10.30919188438809542, -12.61870101168854852 ) ) ;
#34497 = CARTESIAN_POINT ( 'NONE',  ( 120.4379860609119675, -6.564341423271550902, -7.887810678476487425 ) ) ;
#34498 = ORIENTED_EDGE ( 'NONE', *, *, #26557, .T. ) ;
#34499 = EDGE_CURVE ( 'NONE', #11722, #32385, #8523, .T. ) ;
#34500 = LINE ( 'NONE', #23828, #9158 ) ;
#34501 = CARTESIAN_POINT ( 'NONE',  ( 124.9801526047685201, 1.982760200694134056, -10.09727770056924889 ) ) ;
#34502 = CARTESIAN_POINT ( 'NONE',  ( 113.6774108795247997, -8.938348069036489818, -9.318865927141430916 ) ) ;
#34503 = CARTESIAN_POINT ( 'NONE',  ( 115.7610046295247912, -4.863998795839541422, -18.39754474579285315 ) ) ;
#34504 = EDGE_CURVE ( 'NONE', #17518, #29144, #44214, .T. ) ;
#34505 = CARTESIAN_POINT ( 'NONE',  ( 122.7234281442452755, -4.153390946401325223, -8.397313243818185668 ) ) ;
#34506 = CARTESIAN_POINT ( 'NONE',  ( 113.5337081442453240, -0.8288870151387760510, -10.36305467784173118 ) ) ;
#34507 = CARTESIAN_POINT ( 'NONE',  ( 124.7201422582637349, -7.338191648192773364, -20.79841806650483704 ) ) ;
#34508 = EDGE_CURVE ( 'NONE', #36514, #25917, #2396, .T. ) ;
#34509 = EDGE_CURVE ( 'NONE', #43753, #39217, #13803, .T. ) ;
#34510 = VERTEX_POINT ( 'NONE', #3083 ) ;
#34511 = DIRECTION ( 'NONE',  ( -0.7871354856660162103, -0.4483307682966942709, -0.4235767337848251879 ) ) ;
#34512 = CARTESIAN_POINT ( 'NONE',  ( 113.1217858795247935, -0.7896495226426338832, -17.46756447353520159 ) ) ;
#34513 = CARTESIAN_POINT ( 'NONE',  ( 111.6617281442453304, 0.4262465694468514643, -12.03445270309931736 ) ) ;
#34515 = DIRECTION ( 'NONE',  ( 1.000000000000000000, 0.000000000000000000, -0.000000000000000000 ) ) ;
#34514 = CARTESIAN_POINT ( 'NONE',  ( 64.85279889734272274, -37.42711610596241911, -5.218367175100045330 ) ) ;
#34516 = CARTESIAN_POINT ( 'NONE',  ( 124.9357681442453014, -7.643976991954077427, -18.09477374809248928 ) ) ;
#34517 = ORIENTED_EDGE ( 'NONE', *, *, #40661, .F. ) ;
#34518 = CARTESIAN_POINT ( 'NONE',  ( 114.3278814775786429, -10.30919188438810075, -12.61870101168855918 ) ) ;
#34519 = CARTESIAN_POINT ( 'NONE',  ( 126.4599182912957644, 0.09025682329171769158, -14.68838553235235445 ) ) ;
#34520 = CARTESIAN_POINT ( 'NONE',  ( 116.3860827545247787, -2.477300249445798297, -19.15521520033831138 ) ) ;
#34521 = CARTESIAN_POINT ( 'NONE',  ( 124.0281414775786146, -7.643976991954077427, -18.09477374809248928 ) ) ;
#34523 = AXIS2_PLACEMENT_3D ( 'NONE', #23942, #41495, #37821 ) ;
#34522 = CARTESIAN_POINT ( 'NONE',  ( 122.0427081442452817, -9.859900752359378018, -12.68260735090039759 ) ) ;
#34524 = CARTESIAN_POINT ( 'NONE',  ( 94.86797725101156686, -25.79977623989092805, -12.51676909700203666 ) ) ;
#34525 = CARTESIAN_POINT ( 'NONE',  ( 109.8574890045248509, -9.868328341294098749, -11.32035403202665869 ) ) ;
#34526 = DIRECTION ( 'NONE',  ( 0.1352586133457950590, 0.9908103287288504424, 0.000000000000000000 ) ) ;
#34527 = CARTESIAN_POINT ( 'NONE',  ( 67.37136766119182596, -67.53150897494617766, -41.09057840265009531 ) ) ;
#34528 = CARTESIAN_POINT ( 'NONE',  ( 114.4413348109119823, -0.8288870151387760510, -10.36305467784173118 ) ) ;
#34529 = CARTESIAN_POINT ( 'NONE',  ( 70.19189222814998175, -60.97346038181336070, -37.59218076343751136 ) ) ;
#34530 = CARTESIAN_POINT ( 'NONE',  ( 111.7184544649789331, -9.256331613732484698, -16.70304772739236654 ) ) ;
#34531 = CARTESIAN_POINT ( 'NONE',  ( 109.7185827545247889, -2.477300249445798297, -19.15521520033831138 ) ) ;
#34532 = CARTESIAN_POINT ( 'NONE',  ( 125.7866681442452688, -0.4660016031367893996, -10.09054647747474043 ) ) ;
#34533 = CARTESIAN_POINT ( 'NONE',  ( 126.0703014775786102, -9.988377603198980381, -10.36322818467138518 ) ) ;
#34534 = CARTESIAN_POINT ( 'NONE',  ( 111.8698066399283704, 0.4261359969231631739, -14.64321520033831447 ) ) ;
#34535 = CARTESIAN_POINT ( 'NONE',  ( 121.9292548109119849, -1.561330072975668948, -17.79121239304076951 ) ) ;
#34536 = CARTESIAN_POINT ( 'NONE',  ( 115.0653281442453277, -6.344957434206662583, -7.627207830600332805 ) ) ;
#34537 = VERTEX_POINT ( 'NONE', #37045 ) ;
#34538 = CARTESIAN_POINT ( 'NONE',  ( 114.4413348109119823, -0.8288870151387760510, -10.36305467784173118 ) ) ;
#34539 = CARTESIAN_POINT ( 'NONE',  ( 124.4819548109119722, -7.893985811506177619, -18.51759400769804742 ) ) ;
#34540 = CARTESIAN_POINT ( 'NONE',  ( 112.6260814775786514, -9.261995988541697145, -16.69588392320189030 ) ) ;
#34541 = CARTESIAN_POINT ( 'NONE',  ( 117.1074881442453233, 0.4262465694468514643, -12.03445270309931736 ) ) ;
#34542 = VERTEX_POINT ( 'NONE', #5816 ) ;
#34543 = CARTESIAN_POINT ( 'NONE',  ( 118.8092881442453290, -0.1624402480850797581, -16.17319339645315424 ) ) ;
#34544 =( BOUNDED_CURVE ( )  B_SPLINE_CURVE ( 3, ( #23993, #28075, #20565, #38762 ),
 .UNSPECIFIED., .F., .F. ) 
 B_SPLINE_CURVE_WITH_KNOTS ( ( 4, 4 ),
 ( 4.712388980384689674, 4.760535684117931154 ),
 .UNSPECIFIED. ) 
 CURVE ( )  GEOMETRIC_REPRESENTATION_ITEM ( )  RATIONAL_B_SPLINE_CURVE ( ( 1.000000000000000000, 0.9998068339056410680, 0.9998068339056410680, 1.000000000000000000 ) ) 
 REPRESENTATION_ITEM ( '' )  );
#34545 = AXIS2_PLACEMENT_3D ( 'NONE', #6269, #34074, #26344 ) ;
#34546 = CARTESIAN_POINT ( 'NONE',  ( 116.5402214775786405, 0.2603800115204892296, -16.42320221600525088 ) ) ;
#34547 = CARTESIAN_POINT ( 'NONE',  ( 122.6099748109119929, -0.8288870151387760510, -10.36305467784173118 ) ) ;
#34548 = CARTESIAN_POINT ( 'NONE',  ( 116.8699474989354741, -0.1023020899842886217, -15.73832783096735355 ) ) ;
#34549 = CARTESIAN_POINT ( 'NONE',  ( 115.2053796295247849, -4.863998795839590272, -19.15521520033831493 ) ) ;
#34550 = VERTEX_POINT ( 'NONE', #23390 ) ;
#34551 = AXIS2_PLACEMENT_3D ( 'NONE', #31152, #34776, #3559 ) ;
#34552 = CARTESIAN_POINT ( 'NONE',  ( 60.53937939559665438, -4.256997083809236138, -7.393215200338315363 ) ) ;
#34553 = DIRECTION ( 'NONE',  ( 1.000000000000000000, 0.000000000000000000, -0.000000000000000000 ) ) ;
#34554 = FACE_OUTER_BOUND ( 'NONE', #27567, .T. ) ;
#34555 = CARTESIAN_POINT ( 'NONE',  ( 116.3133148109119759, -7.893985811506177619, -18.51759400769804742 ) ) ;
#34556 = CARTESIAN_POINT ( 'NONE',  ( 125.4584548109119737, -4.863998795839242995, -13.39321520033831447 ) ) ;
#34557 = CARTESIAN_POINT ( 'NONE',  ( 113.0798948109119948, -8.899110576539710493, -16.42337572283490132 ) ) ;
#34558 = CARTESIAN_POINT ( 'NONE',  ( 60.02532325032445470, -12.65039385568375963, -17.37383293601393675 ) ) ;
#34559 = ADVANCED_FACE ( 'NONE', ( #40720 ), #26721, .T. ) ;
#34560 = CARTESIAN_POINT ( 'NONE',  ( 111.3123452706805807, 0.3193521225029610777, -14.64321520033833757 ) ) ;
#34561 = CARTESIAN_POINT ( 'NONE',  ( 115.1359265045248605, -2.791137627527939813, -8.388885654883777576 ) ) ;
#34562 = CARTESIAN_POINT ( 'NONE',  ( 118.6391081442452986, -4.089484607189486809, -7.948022111789456723 ) ) ;
#34563 = CARTESIAN_POINT ( 'NONE',  ( 136.6493356239704156, -4.310644207877323275, -19.04512585373862876 ) ) ;
#34564 = PLANE ( 'NONE',  #11390 ) ;
#34565 = DIRECTION ( 'NONE',  ( 0.000000000000000000, -0.4669533266896289669, -0.8842819633428519177 ) ) ;
#34566 = CARTESIAN_POINT ( 'NONE',  ( 119.8303681442453126, 0.4262465694468514643, -12.03445270309931736 ) ) ;
#34567 = ORIENTED_EDGE ( 'NONE', *, *, #17775, .T. ) ;
#34568 = DIRECTION ( 'NONE',  ( 1.000000000000000000, 0.000000000000000000, -0.000000000000000000 ) ) ;
#34569 = EDGE_CURVE ( 'NONE', #16121, #279, #19966, .T. ) ;
#34570 = CARTESIAN_POINT ( 'NONE',  ( 117.6180281442453150, -0.4660016031367893996, -10.09054647747474043 ) ) ;
#34571 = CARTESIAN_POINT ( 'NONE',  ( 116.8722546295247895, -4.863998795839590272, -18.39754474579285315 ) ) ;
#34572 = CARTESIAN_POINT ( 'NONE',  ( 117.2776681442452968, -4.153390946401321671, -8.397313243818183892 ) ) ;
#34573 = CARTESIAN_POINT ( 'NONE',  ( 112.4559014775786778, -0.1624402480850797581, -16.17319339645315424 ) ) ;
#34574 = CARTESIAN_POINT ( 'NONE',  ( 111.2465515045248168, -2.477300249445798297, -7.631215200338321125 ) ) ;
#34575 = CARTESIAN_POINT ( 'NONE',  ( 61.76986277844709861, -39.32091226840162079, -6.340220811149025693 ) ) ;
#34576 = CARTESIAN_POINT ( 'NONE',  ( 112.2883483795247770, -0.7896495226426338832, -9.318865927141430916 ) ) ;
#34577 = CIRCLE ( 'NONE', #10584, 1.610000000000000986 ) ;
#34578 = CARTESIAN_POINT ( 'NONE',  ( 115.1787814775786387, -0.1624402480850797581, -16.17319339645315424 ) ) ;
#34579 = CARTESIAN_POINT ( 'NONE',  ( 120.6245414775786458, -0.1624402480850797581, -16.17319339645315424 ) ) ;
#34580 = CARTESIAN_POINT ( 'NONE',  ( 70.89841814381148311, -71.67679885123182260, -38.80507129598510119 ) ) ;
#34581 = CARTESIAN_POINT ( 'NONE',  ( 122.0354079359119908, -5.444069387712269226, -19.60292469916370450 ) ) ;
#34582 = CARTESIAN_POINT ( 'NONE',  ( 110.1353015045248469, -6.936859964151250502, -18.39754474579286025 ) ) ;
#34583 = CARTESIAN_POINT ( 'NONE',  ( 69.36136150295220659, -52.55181209640981166, -31.11874315707907357 ) ) ;
#34584 = CARTESIAN_POINT ( 'NONE',  ( 114.7816948109119863, 0.5811942927096154232, -14.16772938898807155 ) ) ;
#34585 = CARTESIAN_POINT ( 'NONE',  ( 113.9875214775786532, -0.4660016031367893996, -10.09054647747474043 ) ) ;
#34586 = CARTESIAN_POINT ( 'NONE',  ( 122.0354079359119908, -4.360204210389833968, -8.000047426360245240 ) ) ;
#34587 = ORIENTED_EDGE ( 'NONE', *, *, #28832, .F. ) ;
#34588 = CARTESIAN_POINT ( 'NONE',  ( 113.4690515045247992, -2.477300249445798297, -7.631215200338321125 ) ) ;
#34589 = VECTOR ( 'NONE', #13785, 1000.000000000000000 ) ;
#34590 = ORIENTED_EDGE ( 'NONE', *, *, #44253, .T. ) ;
#34591 = CARTESIAN_POINT ( 'NONE',  ( 123.0637881442452937, -0.4660016031367893996, -10.09054647747474043 ) ) ;
#34592 = CARTESIAN_POINT ( 'NONE',  ( 113.3635281442453504, -9.988377603198976828, -10.36322818467138340 ) ) ;
#34593 = CARTESIAN_POINT ( 'NONE',  ( 119.8870948109119752, -0.8288870151387760510, -10.36305467784173118 ) ) ;
#34594 =( NAMED_UNIT ( * ) PLANE_ANGLE_UNIT ( ) SI_UNIT ( $, .RADIAN. ) );
#34595 = DIRECTION ( 'NONE',  ( 0.9908103287288505534, -0.1352586133457951145, 0.000000000000000000 ) ) ;
#34596 = CARTESIAN_POINT ( 'NONE',  ( 121.8158014775786171, -5.638512984488999180, -18.83840828888717311 ) ) ;
#34597 = CARTESIAN_POINT ( 'NONE',  ( 117.8449348109119938, -8.166667518702817929, -8.995218007635861213 ) ) ;
#34598 = CARTESIAN_POINT ( 'NONE',  ( 107.9128015045248219, -6.936859964151250502, -18.39754474579286025 ) ) ;
#34599 = CARTESIAN_POINT ( 'NONE',  ( 113.8173414775786512, -9.565557343593413364, -10.61323700422348004 ) ) ;
#34600 = CARTESIAN_POINT ( 'NONE',  ( 123.9584548109119737, -5.853704621469987934, -5.454671103420249523 ) ) ;
#34601 = ORIENTED_EDGE ( 'NONE', *, *, #18643, .F. ) ;
#34602 = CARTESIAN_POINT ( 'NONE',  ( 117.2209414775786485, -7.893985811506177619, -18.51759400769804742 ) ) ;
#34603 = EDGE_CURVE ( 'NONE', #28337, #22202, #9941, .T. ) ;
#34604 = CARTESIAN_POINT ( 'NONE',  ( -7.923679509334008664, -5.078949698970065540, -7.393215200338315363 ) ) ;
#34605 = CARTESIAN_POINT ( 'NONE',  ( 115.8595014775786609, -1.834011780172310813, -8.268836392978581529 ) ) ;
#34606 = VERTEX_POINT ( 'NONE', #37508 ) ;
#34607 = CARTESIAN_POINT ( 'NONE',  ( 115.6220983795247861, -0.7896495226426338832, -9.318865927141430916 ) ) ;
#34608 = CARTESIAN_POINT ( 'NONE',  ( 124.1415948109119540, -6.344957434206665248, -7.627207830600338134 ) ) ;
#34609 = CARTESIAN_POINT ( 'NONE',  ( 84.38170309240724976, -24.14644159042263993, -12.62951656296512937 ) ) ;
#34610 = CARTESIAN_POINT ( 'NONE',  ( 124.5059548109119731, -2.529232162391097827, -8.971805383624054997 ) ) ;
#34611 = CARTESIAN_POINT ( 'NONE',  ( 124.6713397424434078, -0.9924539043446091169, -17.29976612834908423 ) ) ;
#34612 = CARTESIAN_POINT ( 'NONE',  ( 116.5969481442453031, -9.859900752359374465, -12.68260735090039404 ) ) ;
#34613 = DIRECTION ( 'NONE',  ( 0.000000000000000000, -0.4669533266896290225, -0.8842819633428516957 ) ) ;
#34614 = CARTESIAN_POINT ( 'NONE',  ( 117.5045748109119756, -9.859900752359374465, -12.68260735090039404 ) ) ;
#34615 = EDGE_CURVE ( 'NONE', #13545, #36181, #6351, .T. ) ;
#34616 = CYLINDRICAL_SURFACE ( 'NONE', #7732, 5.999999999999998224 ) ;
#34617 = CARTESIAN_POINT ( 'NONE',  ( 120.5110881442453206, -3.505236298600246325, -18.68346056562440793 ) ) ;
#34618 = CARTESIAN_POINT ( 'NONE',  ( 122.0354079359119908, -5.444069387712269226, -19.60292469916370450 ) ) ;
#34619 = CARTESIAN_POINT ( 'NONE',  ( 116.7671281442453335, -1.834011780172310813, -8.268836392978581529 ) ) ;
#34620 = CARTESIAN_POINT ( 'NONE',  ( 112.9097148109120070, -9.565557343593413364, -10.61323700422348004 ) ) ;
#34621 = CARTESIAN_POINT ( 'NONE',  ( 117.4478481442453131, -9.565557343593413364, -10.61323700422348004 ) ) ;
#34622 = ORIENTED_EDGE ( 'NONE', *, *, #20874, .F. ) ;
#34623 = CARTESIAN_POINT ( 'NONE',  ( 115.9729548109119861, -6.344957434206662583, -7.627207830600332805 ) ) ;
#34624 = CARTESIAN_POINT ( 'NONE',  ( 108.2600671295247992, -10.62599879583958540, -13.39321520033831447 ) ) ;
#34625 = CARTESIAN_POINT ( 'NONE',  ( 107.7044421295247929, -9.868328341294093420, -13.39321520033831447 ) ) ;
#34626 = CARTESIAN_POINT ( 'NONE',  ( 106.7320983795247855, -8.402594152722688392, -16.93181055722141792 ) ) ;
#34627 = CARTESIAN_POINT ( 'NONE',  ( 113.8604010812576774, -0.01829820670803256055, -12.14321520033831625 ) ) ;
#34628 = AXIS2_PLACEMENT_3D ( 'NONE', #3082, #17442, #34309 ) ;
#34629 = CARTESIAN_POINT ( 'NONE',  ( 121.7023481442452777, -9.261995988541697145, -16.69588392320189030 ) ) ;
#34630 = EDGE_LOOP ( 'NONE', ( #33895, #7950, #37176, #8704, #31377 ) ) ;
#34631 = CARTESIAN_POINT ( 'NONE',  ( 118.5143726669217585, -2.334846009198389805, -18.01015021110788439 ) ) ;
#34632 = CARTESIAN_POINT ( 'NONE',  ( 118.4689281442453392, -10.15424416112533912, -14.75197769757731336 ) ) ;
#34633 = PLANE ( 'NONE',  #39524 ) ;
#34634 = DIRECTION ( 'NONE',  ( 1.000000000000000000, 0.000000000000000000, -0.000000000000000000 ) ) ;
#34635 = CARTESIAN_POINT ( 'NONE',  ( 121.9292548109119849, -1.561330072975668948, -17.79121239304076951 ) ) ;
#34636 = CARTESIAN_POINT ( 'NONE',  ( 113.4690515045247992, -6.936859964151250502, -18.39754474579286025 ) ) ;
#34637 = DIRECTION ( 'NONE',  ( 1.000000000000000000, 0.000000000000000000, 0.000000000000000000 ) ) ;
#34638 = EDGE_LOOP ( 'NONE', ( #43366, #1324, #16754, #24643 ) ) ;
#34639 = CARTESIAN_POINT ( 'NONE',  ( 111.8319081442453182, -5.638512984488999180, -18.83840828888717311 ) ) ;
#34640 = CARTESIAN_POINT ( 'NONE',  ( 112.3991748109119868, -8.166667518702817929, -8.995218007635859436 ) ) ;
#34641 = CARTESIAN_POINT ( 'NONE',  ( 124.4252281442452812, -9.261995988541697145, -16.69588392320189030 ) ) ;
#34642 = CARTESIAN_POINT ( 'NONE',  ( 118.6391081442452986, -5.574606645277164318, -18.38911715685844683 ) ) ;
#34643 = CARTESIAN_POINT ( 'NONE',  ( 61.69189222814998175, -56.75720911921465728, -38.40793382609975737 ) ) ;
#34644 = CARTESIAN_POINT ( 'NONE',  ( 120.8514481442452961, -7.893985811506177619, -18.51759400769804742 ) ) ;
#34645 = LINE ( 'NONE', #20766, #35927 ) ;
#34646 = CARTESIAN_POINT ( 'NONE',  ( 121.9859814775786333, -9.565557343593413364, -10.61323700422348004 ) ) ;
#34647 = ORIENTED_EDGE ( 'NONE', *, *, #21393, .T. ) ;
#34648 = AXIS2_PLACEMENT_3D ( 'NONE', #10140, #2827, #19940 ) ;
#34649 = DIRECTION ( 'NONE',  ( 0.000000000000000000, 0.000000000000000000, 1.000000000000000000 ) ) ;
#34650 = VECTOR ( 'NONE', #12301, 1000.000000000000227 ) ;
#34651 = CARTESIAN_POINT ( 'NONE',  ( 116.1998614775786507, -10.63000616557722466, -14.87417383870573495 ) ) ;
#34652 = CARTESIAN_POINT ( 'NONE',  ( 123.2906948109119867, -1.833838273342659697, -17.42832698103878286 ) ) ;
#34653 = ORIENTED_EDGE ( 'NONE', *, *, #34004, .F. ) ;
#34654 = CARTESIAN_POINT ( 'NONE',  ( 121.2714235609119697, 0.6414057260225851653, -11.69287257290600657 ) ) ;
#34655 = PLANE ( 'NONE',  #37111 ) ;
#34656 = CARTESIAN_POINT ( 'NONE',  ( 124.0281414775786146, -1.834011780172310813, -8.268836392978581529 ) ) ;
#34657 = CARTESIAN_POINT ( 'NONE',  ( 107.0099108795247815, -8.938348069036489818, -9.318865927141430916 ) ) ;
#34658 = CARTESIAN_POINT ( 'NONE',  ( 120.8514481442452961, -2.084020599724406786, -8.691656652584148546 ) ) ;
#34659 = VERTEX_POINT ( 'NONE', #27037 ) ;
#34660 = ORIENTED_EDGE ( 'NONE', *, *, #22277, .F. ) ;
#34661 = CARTESIAN_POINT ( 'NONE',  ( 115.4056881442453459, -7.893985811506177619, -18.51759400769804742 ) ) ;
#34662 = CARTESIAN_POINT ( 'NONE',  ( 125.4463081442452932, -4.153390946401325223, -8.397313243818185668 ) ) ;
#34663 =( REPRESENTATION_RELATIONSHIP ('NONE','NONE', #36667, #850 ) REPRESENTATION_RELATIONSHIP_WITH_TRANSFORMATION ( #9493 )SHAPE_REPRESENTATION_RELATIONSHIP( ) );
#34664 = DIRECTION ( 'NONE',  ( 0.000000000000000000, -0.3818493186865936084, 0.9242245927363024194 ) ) ;
#34665 = DIRECTION ( 'NONE',  ( -0.9908103287288503314, 0.1352586133457959749, 0.000000000000000000 ) ) ;
#34666 = CARTESIAN_POINT ( 'NONE',  ( 122.2696148109119889, -4.089484607189486809, -7.948022111789456723 ) ) ;
#34667 = AXIS2_PLACEMENT_3D ( 'NONE', #40818, #44460, #27127 ) ;
#34668 = EDGE_CURVE ( 'NONE', #7297, #30491, #42575, .T. ) ;
#34669 = CARTESIAN_POINT ( 'NONE',  ( 116.9948677074048931, -2.419733177069680607, -17.89711025544712442 ) ) ;
#34670 = CARTESIAN_POINT ( 'NONE',  ( 120.3409081442453044, -0.4660016031367893996, -10.09054647747474043 ) ) ;
#34672 = CARTESIAN_POINT ( 'NONE',  ( 118.2420214775786320, -6.222761293078241884, -8.102969835052219238 ) ) ;
#34671 = CARTESIAN_POINT ( 'NONE',  ( 119.0929214775786278, -5.638512984488999180, -18.83840828888717311 ) ) ;
#34673 = DIRECTION ( 'NONE',  ( 1.000000000000000000, 0.000000000000000000, 0.000000000000000000 ) ) ;
#34674 = CARTESIAN_POINT ( 'NONE',  ( 115.2922348109119781, -10.63000616557722466, -14.87417383870573495 ) ) ;
#34675 = VERTEX_POINT ( 'NONE', #39980 ) ;
#34676 = CIRCLE ( 'NONE', #17934, 5.000000000000005329 ) ;
#34677 = CARTESIAN_POINT ( 'NONE',  ( 116.0861162244890892, -0.02276961308034231024, -12.14321520033833934 ) ) ;
#34678 = CARTESIAN_POINT ( 'NONE',  ( 108.9545983795247821, -0.7896495226426338832, -9.318865927141430916 ) ) ;
#34679 = CARTESIAN_POINT ( 'NONE',  ( 108.0517077545248696, -2.791137627527939813, -18.39754474579286025 ) ) ;
#34680 = CARTESIAN_POINT ( 'NONE',  ( 107.0099108795247815, -8.938348069036489818, -9.318865927141430916 ) ) ;
#34681 = CARTESIAN_POINT ( 'NONE',  ( 113.3635281442453504, -9.988377603198976828, -10.36322818467138340 ) ) ;
#34682 = ORIENTED_EDGE ( 'NONE', *, *, #20144, .T. ) ;
#34683 = CARTESIAN_POINT ( 'NONE',  ( 124.5386814775786206, -5.638512984488999180, -18.83840828888717311 ) ) ;
#34684 = CARTESIAN_POINT ( 'NONE',  ( 112.9134265045247645, -7.250697342233347165, -19.15521520033831138 ) ) ;
#34685 = LINE ( 'NONE', #38553, #14668 ) ;
#34686 = CARTESIAN_POINT ( 'NONE',  ( 123.9146881442452894, 0.9020085738987339008, -11.91225656197089222 ) ) ;
#34687 = CARTESIAN_POINT ( 'NONE',  ( 124.5954081442453116, -3.383040157471821630, -19.15922257007629170 ) ) ;
#34688 = DIRECTION ( 'NONE',  ( 0.000000000000000000, 0.9284778069183720062, 0.3713878862591650232 ) ) ;
#34689 = CARTESIAN_POINT ( 'NONE',  ( 113.5337081442453240, -9.261995988541697145, -16.69588392320189030 ) ) ;
#34690 = CARTESIAN_POINT ( 'NONE',  ( 123.3550173109119612, -9.289237151508434209, -11.05642687123711276 ) ) ;
#34691 = CARTESIAN_POINT ( 'NONE',  ( 107.4960827545248350, -2.477300249445798297, -19.15521520033831138 ) ) ;
#34692 = VERTEX_POINT ( 'NONE', #1447 ) ;
#34693 = DIRECTION ( 'NONE',  ( 1.000000000000000000, 0.000000000000000000, 0.000000000000000000 ) ) ;
#34694 = CARTESIAN_POINT ( 'NONE',  ( 113.8173414775786512, -9.565557343593413364, -10.61323700422348004 ) ) ;
#34695 = CARTESIAN_POINT ( 'NONE',  ( 113.7038881442453402, -3.383040157471821630, -19.15922257007629170 ) ) ;
#34696 = VECTOR ( 'NONE', #517, 1000.000000000000114 ) ;
#34697 = CARTESIAN_POINT ( 'NONE',  ( 113.8163171295247764, -10.62599879583958540, -13.39321520033831447 ) ) ;
#34698 = CARTESIAN_POINT ( 'NONE',  ( 106.2459265045248173, -2.791137627527939813, -8.388885654883777576 ) ) ;
#34699 = CARTESIAN_POINT ( 'NONE',  ( 119.8303681442453126, 0.4262465694468514643, -12.03445270309931736 ) ) ;
#34700 = CARTESIAN_POINT ( 'NONE',  ( 115.5758681442453053, -7.894159318335828068, -9.358103419637847864 ) ) ;
#34701 = CARTESIAN_POINT ( 'NONE',  ( 113.1366214775786432, -7.643976991954077427, -18.09477374809248928 ) ) ;
#34702 = ORIENTED_EDGE ( 'NONE', *, *, #40774, .T. ) ;
#34703 = VECTOR ( 'NONE', #13362, 1000.000000000000227 ) ;
#34704 = CARTESIAN_POINT ( 'NONE',  ( 121.9659548109119811, -2.527210466738041728, -8.967976844669124148 ) ) ;
#34705 = DIRECTION ( 'NONE',  ( 0.5735764363510498232, -0.3127926500124802445, 0.7570804645221007600 ) ) ;
#34706 = CARTESIAN_POINT ( 'NONE',  ( 115.6893214775786447, -9.859900752359374465, -12.68260735090039404 ) ) ;
#34707 = EDGE_LOOP ( 'NONE', ( #6472, #4751, #8841, #37875, #13305, #23725, #30650, #9727, #43957, #34059, #44665, #18283, #10682, #8934, #24683 ) ) ;
#34708 = CARTESIAN_POINT ( 'NONE',  ( 89.12784890491134604, -25.99489077589524300, -13.39321520033831625 ) ) ;
#34709 = AXIS2_PLACEMENT_3D ( 'NONE', #13668, #20510, #40809 ) ;
#34710 = ORIENTED_EDGE ( 'NONE', *, *, #13608, .F. ) ;
#34711 = CARTESIAN_POINT ( 'NONE',  ( 118.8092881442453290, -0.1624402480850797581, -16.17319339645315424 ) ) ;
#34712 = B_SPLINE_CURVE_WITH_KNOTS ( 'NONE', 3,
 ( #15469, #15240, #29148, #43061 ),
 .UNSPECIFIED., .F., .F.,
 ( 4, 4 ),
 ( 0.000000000000000000, 1.000000000000000000 ),
 .UNSPECIFIED. ) ;
#34713 = CARTESIAN_POINT ( 'NONE',  ( 113.1366214775786432, -7.643976991954077427, -18.09477374809248928 ) ) ;
#34714 = LINE ( 'NONE', #31306, #26053 ) ;
#34715 = CARTESIAN_POINT ( 'NONE',  ( 121.9659548109119811, -2.527210466738041728, -8.967976844669124148 ) ) ;
#34716 = EDGE_LOOP ( 'NONE', ( #13547, #32608, #33382, #26776 ) ) ;
#34717 = CARTESIAN_POINT ( 'NONE',  ( 70.19189222814998175, -53.33815113939435548, -34.53808368179734600 ) ) ;
#34718 = CARTESIAN_POINT ( 'NONE',  ( 124.1726284085847851, 0.04950309887738641584, -7.080035182150737683 ) ) ;
#34719 = CARTESIAN_POINT ( 'NONE',  ( 114.7192077545248594, -7.250697342233347165, -7.631215200338321125 ) ) ;
#34720 = CIRCLE ( 'NONE', #4888, 2.999999999999999556 ) ;
#34721 = DIRECTION ( 'NONE',  ( 1.000000000000000000, 0.000000000000000000, -0.000000000000000000 ) ) ;
#34722 = CARTESIAN_POINT ( 'NONE',  ( 124.4819548109119722, -2.084020599724406786, -8.691656652584148546 ) ) ;
#34723 = CARTESIAN_POINT ( 'NONE',  ( 117.7882081442453170, -3.505236298600246325, -18.68346056562440793 ) ) ;
#34724 = CARTESIAN_POINT ( 'NONE',  ( 119.6811727111058588, -1.267766418764730840, -16.93314635290706605 ) ) ;
#34725 = VERTEX_POINT ( 'NONE', #43188 ) ;
#34726 = DIRECTION ( 'NONE',  ( 0.5735764363510498232, -0.3127926500124802445, 0.7570804645221007600 ) ) ;
#34727 = CARTESIAN_POINT ( 'NONE',  ( 115.2355081442453155, 0.1319031606808879209, -14.10382304977623669 ) ) ;
#34728 = EDGE_CURVE ( 'NONE', #8919, #22099, #16503, .T. ) ;
#34729 = CARTESIAN_POINT ( 'NONE',  ( 64.01282776924008999, -34.86145050234443943, -5.893215200338315363 ) ) ;
#34730 = CARTESIAN_POINT ( 'NONE',  ( 116.8011953663348805, -1.172797794773246416, -17.05961127468924587 ) ) ;
#34731 = CARTESIAN_POINT ( 'NONE',  ( 114.3846081442453197, -10.63000616557722466, -14.87417383870573495 ) ) ;
#34732 = ORIENTED_EDGE ( 'NONE', *, *, #37000, .F. ) ;
#34733 = CARTESIAN_POINT ( 'NONE',  ( 115.3489614775786407, -9.261995988541697145, -16.69588392320189030 ) ) ;
#34734 = CARTESIAN_POINT ( 'NONE',  ( 61.69189222814998175, -49.76310523276723785, -19.39321520033831447 ) ) ;
#34735 = CARTESIAN_POINT ( 'NONE',  ( 106.1764733795248219, -1.325403438956436419, -9.854619843455211026 ) ) ;
#34736 = CARTESIAN_POINT ( 'NONE',  ( 113.2500748109119968, -6.344957434206662583, -7.627207830600332805 ) ) ;
#34737 = CARTESIAN_POINT ( 'NONE',  ( 113.1933481442453058, -4.089484607189486809, -7.948022111789456723 ) ) ;
#34738 = AXIS2_PLACEMENT_3D ( 'NONE', #17922, #24547, #809 ) ;
#34739 = CARTESIAN_POINT ( 'NONE',  ( 125.0492214775786266, -3.505236298600246325, -18.68346056562440793 ) ) ;
#34740 = EDGE_CURVE ( 'NONE', #40113, #8883, #11075, .T. ) ;
#34741 = CARTESIAN_POINT ( 'NONE',  ( 112.2883483795247770, -8.402594152722633325, -16.93181055722145345 ) ) ;
#34742 = CARTESIAN_POINT ( 'NONE',  ( 108.9545983795247821, -8.402594152722688392, -16.93181055722141792 ) ) ;
#34743 = CARTESIAN_POINT ( 'NONE',  ( 120.2798381407226032, -1.081026697600536046, -17.18181821144402832 ) ) ;
#34744 = CARTESIAN_POINT ( 'NONE',  ( 109.2294549733054652, -7.062974527347291698, -18.20822852925657998 ) ) ;
#34745 = CARTESIAN_POINT ( 'NONE',  ( 118.2420214775786320, -6.222761293078241884, -8.102969835052219238 ) ) ;
#34746 = CARTESIAN_POINT ( 'NONE',  ( 61.58853448128274266, 6.499901296646661386, -12.14321520033831625 ) ) ;
#34747 = CARTESIAN_POINT ( 'NONE',  ( 116.1082702545247827, 0.1403307496149616695, -11.32035403202665336 ) ) ;
#34748 = CARTESIAN_POINT ( 'NONE',  ( 109.4407702545248355, -10.62599879583958717, -15.77991374673208469 ) ) ;
#34749 = CARTESIAN_POINT ( 'NONE',  ( 123.3474214775786209, -9.988377603198976828, -10.36322818467138340 ) ) ;
#34750 = CARTESIAN_POINT ( 'NONE',  ( 125.7299414775786346, 0.9020085738987339008, -11.91225656197089222 ) ) ;
#34751 = CARTESIAN_POINT ( 'NONE',  ( 119.8870948109119752, -0.8288870151387535135, -10.36305467784176138 ) ) ;
#34752 = CARTESIAN_POINT ( 'NONE',  ( 120.6245414775786458, -9.988377603198976828, -10.36322818467138340 ) ) ;
#34753 = CARTESIAN_POINT ( 'NONE',  ( 118.0718414775786300, -9.261995988541697145, -16.69588392320189030 ) ) ;
#34754 = ORIENTED_EDGE ( 'NONE', *, *, #15840, .T. ) ;
#34755 = CARTESIAN_POINT ( 'NONE',  ( 116.0864081442453113, -0.1624402480850797581, -16.17319339645315424 ) ) ;
#34756 = CARTESIAN_POINT ( 'NONE',  ( 125.6164881442453094, 0.2603800115204892296, -16.42320221600525088 ) ) ;
#34757 = CARTESIAN_POINT ( 'NONE',  ( 113.1933481442453058, -4.089484607189486809, -7.948022111789456723 ) ) ;
#34758 = AXIS2_PLACEMENT_3D ( 'NONE', #2839, #20188, #6725 ) ;
#34759 = CARTESIAN_POINT ( 'NONE',  ( 114.6115148109119986, -6.222761293078241884, -8.102969835052219238 ) ) ;
#34760 = ORIENTED_EDGE ( 'NONE', *, *, #41032, .T. ) ;
#34761 = EDGE_CURVE ( 'NONE', #2194, #20823, #39080, .T. ) ;
#34762 = CARTESIAN_POINT ( 'NONE',  ( 121.0783548109119749, -9.565557343593413364, -10.61323700422348004 ) ) ;
#34763 = EDGE_CURVE ( 'NONE', #8410, #31533, #19421, .T. ) ;
#34764 = EDGE_CURVE ( 'NONE', #11839, #19331, #9960, .T. ) ;
#34765 = CARTESIAN_POINT ( 'NONE',  ( 118.2420214775786320, -3.383040157471821630, -19.15922257007629170 ) ) ;
#34766 = DIRECTION ( 'NONE',  ( 0.000000000000000000, 0.6004852223388321697, -0.7996358532186279566 ) ) ;
#34767 = CARTESIAN_POINT ( 'NONE',  ( 113.5385046295247804, -4.863998795839590272, -7.631215200338315796 ) ) ;
#34768 = ORIENTED_EDGE ( 'NONE', *, *, #10847, .T. ) ;
#34769 = LINE ( 'NONE', #6983, #10415 ) ;
#34770 = DIRECTION ( 'NONE',  ( -0.000000000000000000, -0.9284778069183721172, -0.3713878862591650232 ) ) ;
#34771 = CARTESIAN_POINT ( 'NONE',  ( 119.7434548109119703, -8.245233026025740486, -17.07659070123625611 ) ) ;
#34772 = CARTESIAN_POINT ( 'NONE',  ( 115.9162281442453235, -4.089484607189486809, -7.948022111789456723 ) ) ;
#34773 = CARTESIAN_POINT ( 'NONE',  ( 136.5278073585146217, -10.56988143321154539, -13.98918071750362735 ) ) ;
#34774 = CARTESIAN_POINT ( 'NONE',  ( 124.5966688623432219, -9.713577380183913590, -14.62808432448665563 ) ) ;
#34775 = CARTESIAN_POINT ( 'NONE',  ( 62.89961678332094408, -12.58539693385646885, -16.60389039546696566 ) ) ;
#34776 = DIRECTION ( 'NONE',  ( -0.000000000000000000, -0.9284778069183720062, -0.3713878862591650232 ) ) ;
#34777 = CARTESIAN_POINT ( 'NONE',  ( 113.7468640045248236, 0.1403307496149616695, -15.46607636864997204 ) ) ;
#34778 = CARTESIAN_POINT ( 'NONE',  ( 118.8660148109119774, -10.30919188438810075, -12.61870101168855918 ) ) ;
#34779 = CARTESIAN_POINT ( 'NONE',  ( 70.47992290675011873, 2.032776587329049978, -10.39321520033831625 ) ) ;
#34780 = EDGE_CURVE ( 'NONE', #42481, #19894, #10120, .T. ) ;
#34781 = CARTESIAN_POINT ( 'NONE',  ( 111.7062228165344067, -2.324775150319231098, -18.02356106541843062 ) ) ;
#34782 = CYLINDRICAL_SURFACE ( 'NONE', #21443, 6.999999999999999112 ) ;
#34783 = CARTESIAN_POINT ( 'NONE',  ( 122.8936081442453059, -9.565557343593413364, -10.61323700422348004 ) ) ;
#34784 = ORIENTED_EDGE ( 'NONE', *, *, #13884, .F. ) ;
#34785 = LINE ( 'NONE', #20691, #10066 ) ;
#34786 = CARTESIAN_POINT ( 'NONE',  ( 119.8870948109119752, -9.261995988541697145, -16.69588392320189030 ) ) ;
#34787 = CARTESIAN_POINT ( 'NONE',  ( 117.2294421295247844, 1.035107641088057973, -12.14321520033831625 ) ) ;
#34788 = CARTESIAN_POINT ( 'NONE',  ( 115.8027748109119841, -8.899110576539710493, -16.42337572283490132 ) ) ;
#34789 = CARTESIAN_POINT ( 'NONE',  ( 111.4915481442453142, -1.833838273342658365, -17.42832698103878286 ) ) ;
#34790 = EDGE_CURVE ( 'NONE', #10447, #43343, #12635, .T. ) ;
#34791 = DIRECTION ( 'NONE',  ( 0.000000000000000000, 0.000000000000000000, 1.000000000000000000 ) ) ;
#34792 = CARTESIAN_POINT ( 'NONE',  ( 113.6079577545248043, -7.250697342233347165, -7.631215200338321125 ) ) ;
#34793 = CARTESIAN_POINT ( 'NONE',  ( 118.6958348109119754, -3.505236298600246325, -18.68346056562440793 ) ) ;
#34794 = CARTESIAN_POINT ( 'NONE',  ( 120.9649014775786355, -6.222761293078241884, -8.102969835052219238 ) ) ;
#34795 = CARTESIAN_POINT ( 'NONE',  ( 109.2294886045864502, -1.390863055952577865, -9.246587650953511428 ) ) ;
#34796 = CARTESIAN_POINT ( 'NONE',  ( 122.8688454359119646, -11.07370829466463569, -12.81314460846529002 ) ) ;
#34797 = CARTESIAN_POINT ( 'NONE',  ( 107.2182702545248105, 0.1403307496149616695, -11.32035403202665336 ) ) ;
#34798 = DIRECTION ( 'NONE',  ( -0.9908103287288503314, 0.1352586133457956419, 0.000000000000000000 ) ) ;
#34799 = CARTESIAN_POINT ( 'NONE',  ( 112.7395348109119766, -5.638512984488999180, -18.83840828888717311 ) ) ;
#34800 = CARTESIAN_POINT ( 'NONE',  ( 116.1998614775786507, -10.63000616557722466, -14.87417383870573495 ) ) ;
#34801 = CARTESIAN_POINT ( 'NONE',  ( 109.3018640045248304, -10.62599879583958717, -11.00651665394454604 ) ) ;
#34802 = CARTESIAN_POINT ( 'NONE',  ( 123.3550173109119612, -9.289237151508434209, -11.05642687123711276 ) ) ;
#34803 = ORIENTED_EDGE ( 'NONE', *, *, #42588, .T. ) ;
#34804 = DIRECTION ( 'NONE',  ( 0.000000000000000000, 0.000000000000000000, -1.000000000000000000 ) ) ;
#34805 = CARTESIAN_POINT ( 'NONE',  ( 120.5678148109119832, -8.166667518702819706, -8.995218007635861213 ) ) ;
#34806 = CARTESIAN_POINT ( 'NONE',  ( 126.4106614775786284, -6.222761293078241884, -8.102969835052219238 ) ) ;
#34807 = CARTESIAN_POINT ( 'NONE',  ( 117.3911214775786505, -7.894159318335828068, -9.358103419637847864 ) ) ;
#34808 = CARTESIAN_POINT ( 'NONE',  ( 124.0281414775786146, -1.834011780172310813, -8.268836392978581529 ) ) ;
#34809 = CARTESIAN_POINT ( 'NONE',  ( 119.8870948109119752, -9.261995988541697145, -16.69588392320189030 ) ) ;
#34810 = EDGE_CURVE ( 'NONE', #12347, #36520, #25255, .T. ) ;
#34811 = CARTESIAN_POINT ( 'NONE',  ( 108.8851452545248151, -9.868328341294098749, -15.46607636864997204 ) ) ;
#34812 = AXIS2_PLACEMENT_3D ( 'NONE', #22319, #12066, #30066 ) ;
#34813 = CARTESIAN_POINT ( 'NONE',  ( 113.0231681442453180, -10.15424416112533912, -14.75197769757731336 ) ) ;
#34814 = CARTESIAN_POINT ( 'NONE',  ( 124.9357681442453156, -7.643976991953527644, -18.09477374809256034 ) ) ;
#34815 = ORIENTED_EDGE ( 'NONE', *, *, #22524, .T. ) ;
#34816 = ADVANCED_FACE ( 'NONE', ( #5993 ), #10541, .T. ) ;
#34817 = CARTESIAN_POINT ( 'NONE',  ( 122.6667014775786413, -7.893985811506177619, -18.51759400769804742 ) ) ;
#34818 = CARTESIAN_POINT ( 'NONE',  ( 120.0907204359119760, 1.345710702986147034, -13.97328579221134426 ) ) ;
#34819 = CARTESIAN_POINT ( 'NONE',  ( 116.4834948109119779, -1.561330072975668504, -17.79121239304076951 ) ) ;
#34820 = ORIENTED_EDGE ( 'NONE', *, *, #41745, .T. ) ;
#34821 = CARTESIAN_POINT ( 'NONE',  ( 114.0246765045248196, -7.250697342233347165, -19.15521520033831138 ) ) ;
#34822 = CARTESIAN_POINT ( 'NONE',  ( 124.7655881442452852, 0.5811942927096110934, -14.16772938898807510 ) ) ;
#34823 = CARTESIAN_POINT ( 'NONE',  ( 122.3830681442452857, -8.166667518702830364, -8.995218007635870094 ) ) ;
#34824 = CARTESIAN_POINT ( 'NONE',  ( 124.7570620761208744, -6.011119092344218373, -18.28530538883421386 ) ) ;
#34825 = CARTESIAN_POINT ( 'NONE',  ( 128.2184548109119930, -0.6896191363000483410, -17.70303589939592825 ) ) ;
#34826 = CARTESIAN_POINT ( 'NONE',  ( 120.5110881442453206, -3.505236298600246325, -18.68346056562440793 ) ) ;
#34827 = CARTESIAN_POINT ( 'NONE',  ( 70.19189222814998175, -56.69156685714467159, -35.87943827948784303 ) ) ;
#34828 = CARTESIAN_POINT ( 'NONE',  ( 120.0572748109119772, -6.222761293078241884, -8.102969835052219238 ) ) ;
#34829 = DIRECTION ( 'NONE',  ( 0.000000000000000000, 0.000000000000000000, -1.000000000000000000 ) ) ;
#34830 = CARTESIAN_POINT ( 'NONE',  ( 120.3976348109119812, -7.643976991954077427, -18.09477374809248928 ) ) ;
#34831 = CARTESIAN_POINT ( 'NONE',  ( 120.7157985609119635, -10.36940331770106916, -15.09355782777062061 ) ) ;
#34832 = CARTESIAN_POINT ( 'NONE',  ( 117.3911214775786505, -1.561330072975668504, -17.79121239304076951 ) ) ;
#34833 = DIRECTION ( 'NONE',  ( 0.000000000000000000, -0.9242245927363028635, -0.3818493186865927758 ) ) ;
#34834 = CARTESIAN_POINT ( 'NONE',  ( 115.1787814775786387, -0.1624402480850797581, -16.17319339645315424 ) ) ;
#34835 = ORIENTED_EDGE ( 'NONE', *, *, #30870, .T. ) ;
#34836 = CARTESIAN_POINT ( 'NONE',  ( 115.4056881442453459, -7.893985811506177619, -18.51759400769804742 ) ) ;
#34837 = CARTESIAN_POINT ( 'NONE',  ( 108.6073327545248048, -2.477300249445798297, -19.15521520033831138 ) ) ;
#34838 = CARTESIAN_POINT ( 'NONE',  ( 87.80477198183443477, -26.75858941326842810, -11.54476601486570964 ) ) ;
#34839 = CARTESIAN_POINT ( 'NONE',  ( -13.32377113153209791, -5.100909530930220370, -8.593215200338315540 ) ) ;
#34840 = CARTESIAN_POINT ( 'NONE',  ( 127.7816961174390258, -4.552121613038932146, -15.05751623555017993 ) ) ;
#34841 = CARTESIAN_POINT ( 'NONE',  ( 121.7590748109119687, -7.893985811506177619, -18.51759400769804742 ) ) ;
#34842 = ORIENTED_EDGE ( 'NONE', *, *, #20886, .T. ) ;
#34843 = CARTESIAN_POINT ( 'NONE',  ( 126.8137406967828582, -8.727882229017838611, -9.768360422713213254 ) ) ;
#34844 = CARTESIAN_POINT ( 'NONE',  ( 116.5402214775786405, -9.565557343593413364, -10.61323700422348004 ) ) ;
#34845 = CARTESIAN_POINT ( 'NONE',  ( 116.3700414775786527, -5.638512984489023161, -18.83840828888716601 ) ) ;
#34846 = CARTESIAN_POINT ( 'NONE',  ( 61.65122664504198013, -14.46472737607295045, -17.88559175297232784 ) ) ;
#34847 = EDGE_CURVE ( 'NONE', #16965, #16241, #27402, .T. ) ;
#34848 = CARTESIAN_POINT ( 'NONE',  ( 124.1983214775786166, -8.166667518702819706, -8.995218007635861213 ) ) ;
#34849 = CARTESIAN_POINT ( 'NONE',  ( 112.2883483795247770, -8.402594152722688392, -16.93181055722141792 ) ) ;
#34850 = CARTESIAN_POINT ( 'NONE',  ( 124.2193060444391790, -1.267766418764731728, -16.93314635290706605 ) ) ;
#34851 = ORIENTED_EDGE ( 'NONE', *, *, #10825, .F. ) ;
#34852 = CARTESIAN_POINT ( 'NONE',  ( 115.6325948109119821, 0.2603800115204892296, -16.42320221600525088 ) ) ;
#34853 = CARTESIAN_POINT ( 'NONE',  ( 125.6164881442453094, -9.565557343593413364, -10.61323700422348004 ) ) ;
#34854 = CARTESIAN_POINT ( 'NONE',  ( 122.7234281442452755, -5.638512984488999180, -18.83840828888717311 ) ) ;
#34855 = CARTESIAN_POINT ( 'NONE',  ( 118.8092881442453290, -0.1624402480850797581, -16.17319339645315424 ) ) ;
#34856 = LINE ( 'NONE', #3642, #23405 ) ;
#34857 = CARTESIAN_POINT ( 'NONE',  ( 118.1852948109119836, -5.638512984488999180, -18.83840828888717311 ) ) ;
#34858 = CARTESIAN_POINT ( 'NONE',  ( 119.6811727111058588, -1.267766418764730840, -16.93314635290706605 ) ) ;
#34859 = CARTESIAN_POINT ( 'NONE',  ( 123.8012348109119642, -9.565557343593413364, -10.61323700422348004 ) ) ;
#34860 = EDGE_LOOP ( 'NONE', ( #43933, #7496, #5859, #38489 ) ) ;
#34861 = DIRECTION ( 'NONE',  ( -0.9908103287288504424, 0.1352586133457950590, 0.000000000000000000 ) ) ;
#34862 = CARTESIAN_POINT ( 'NONE',  ( 115.6325948109119821, 0.2603800115204892296, -16.42320221600525088 ) ) ;
#34863 = EDGE_CURVE ( 'NONE', #43791, #44074, #29656, .T. ) ;
#34864 = CARTESIAN_POINT ( 'NONE',  ( 124.7655881442452852, -9.859900752359378018, -12.68260735090039759 ) ) ;
#34865 = ORIENTED_EDGE ( 'NONE', *, *, #37614, .T. ) ;
#34866 = CARTESIAN_POINT ( 'NONE',  ( 136.2267163768073601, -1.228667602531395620, -8.800274834874135976 ) ) ;
#34867 = CARTESIAN_POINT ( 'NONE',  ( 122.8368814775786291, -1.561330072975668948, -17.79121239304076951 ) ) ;
#34868 = CARTESIAN_POINT ( 'NONE',  ( 106.1070202545248407, -10.62599879583958717, -15.77991374673208469 ) ) ;
#34869 = CARTESIAN_POINT ( 'NONE',  ( 118.6391081442452986, -5.574606645277164318, -18.38911715685844683 ) ) ;
#34870 = ORIENTED_EDGE ( 'NONE', *, *, #37683, .F. ) ;
#34871 = ORIENTED_EDGE ( 'NONE', *, *, #27901, .F. ) ;
#34872 = CARTESIAN_POINT ( 'NONE',  ( 115.0086014775786509, -4.089484607189486809, -7.948022111789456723 ) ) ;
#34873 = AXIS2_PLACEMENT_3D ( 'NONE', #17500, #32300, #11566 ) ;
#34874 = CARTESIAN_POINT ( 'NONE',  ( 123.8012348109119642, -9.565557343593413364, -10.61323700422348004 ) ) ;
#34875 = CIRCLE ( 'NONE', #18889, 2.000000000000000444 ) ;
#34876 = CARTESIAN_POINT ( 'NONE',  ( 120.2274548109119934, 0.5811942927096084288, -14.16772938898808931 ) ) ;
#34877 = DIRECTION ( 'NONE',  ( 0.000000000000000000, 0.000000000000000000, -1.000000000000000000 ) ) ;
#34878 = CARTESIAN_POINT ( 'NONE',  ( 121.1918081442452859, 0.9020085738987339008, -11.91225656197089222 ) ) ;
#34879 = DIRECTION ( 'NONE',  ( 0.9908103287288513306, -0.1352586133457890638, 0.000000000000000000 ) ) ;
#34880 = CARTESIAN_POINT ( 'NONE',  ( 116.9555940574772706, -2.443475742715334853, -17.86549347949429389 ) ) ;
#34881 = CARTESIAN_POINT ( 'NONE',  ( 122.6667014775786413, -7.893985811506177619, -18.51759400769804742 ) ) ;
#34883 = CARTESIAN_POINT ( 'NONE',  ( 122.5532481442453019, 0.4262465694468514643, -12.03445270309931736 ) ) ;
#34882 = CARTESIAN_POINT ( 'NONE',  ( 118.9794681442453026, -9.261995988541697145, -16.69588392320189030 ) ) ;
#34884 = CARTESIAN_POINT ( 'NONE',  ( 120.0005481442453146, -4.153390946401325223, -8.397313243818185668 ) ) ;
#34885 = CARTESIAN_POINT ( 'NONE',  ( 128.2184548109119930, -5.622599431619523358, -7.441364641445410655 ) ) ;
#34886 = CARTESIAN_POINT ( 'NONE',  ( 116.4834948109119779, -1.561330072975668504, -17.79121239304076951 ) ) ;
#34887 = VERTEX_POINT ( 'NONE', #5700 ) ;
#34888 = CARTESIAN_POINT ( 'NONE',  ( 88.22708560785949317, -3.622631779710408395, -16.89321520033831447 ) ) ;
#34889 = CARTESIAN_POINT ( 'NONE',  ( 105.9681140045248355, -10.62599879583958717, -11.00651665394454604 ) ) ;
#34890 = CARTESIAN_POINT ( 'NONE',  ( 109.4407702545248355, 0.1403307496149616695, -11.32035403202665336 ) ) ;
#34891 = CARTESIAN_POINT ( 'NONE',  ( 109.5796765045248122, -7.250697342233347165, -19.15521520033831138 ) ) ;
#34892 = CARTESIAN_POINT ( 'NONE',  ( 125.1521348109119742, -1.861572684144302992, -17.39139446643087084 ) ) ;
#34893 = CARTESIAN_POINT ( 'NONE',  ( 124.9357681442453014, -7.643976991954077427, -18.09477374809248928 ) ) ;
#34894 = VERTEX_POINT ( 'NONE', #30556 ) ;
#34895 = CARTESIAN_POINT ( 'NONE',  ( 114.0442481442453300, -7.643976991954077427, -18.09477374809248928 ) ) ;
#34896 = CARTESIAN_POINT ( 'NONE',  ( 111.6632702545248605, -10.62599879583958717, -15.77991374673208469 ) ) ;
#34897 = FACE_OUTER_BOUND ( 'NONE', #31196, .T. ) ;
#34898 = CARTESIAN_POINT ( 'NONE',  ( 121.8725281442453223, -3.383040157471821630, -19.15922257007629170 ) ) ;
#34899 = CARTESIAN_POINT ( 'NONE',  ( 123.2339681442453241, -6.344957434206665248, -7.627207830600338134 ) ) ;
#34900 = CARTESIAN_POINT ( 'NONE',  ( 119.1846548109119794, -7.198765429287387718, -17.81462501705257395 ) ) ;
#34901 = CARTESIAN_POINT ( 'NONE',  ( 113.8740681442453138, 0.5811942927096154232, -14.16772938898807155 ) ) ;
#34902 = CARTESIAN_POINT ( 'NONE',  ( 116.5249890045247980, 0.8980012041604421569, -15.77991374673208469 ) ) ;
#34903 = CARTESIAN_POINT ( 'NONE',  ( 106.7320983795247855, -0.7896495226426338832, -9.318865927141430916 ) ) ;
#34904 = EDGE_LOOP ( 'NONE', ( #1847, #33555, #16944, #3925 ) ) ;
#34905 = FACE_OUTER_BOUND ( 'NONE', #24473, .T. ) ;
#34906 = CARTESIAN_POINT ( 'NONE',  ( 113.5904348109119866, -2.084020599724406786, -8.691656652584148546 ) ) ;
#34907 = CARTESIAN_POINT ( 'NONE',  ( 113.6471614775786492, -5.638512984488999180, -18.83840828888717311 ) ) ;
#34908 = TOROIDAL_SURFACE ( 'NONE', #15273, 2.200000000000000178, 0.2000000000000000111 ) ;
#34909 = CARTESIAN_POINT ( 'NONE',  ( 113.6079577545248043, -7.250697342233347165, -7.631215200338321125 ) ) ;
#34910 = CARTESIAN_POINT ( 'NONE',  ( 105.9681140045248355, 0.1403307496149616695, -15.46607636864997204 ) ) ;
#34911 = CARTESIAN_POINT ( 'NONE',  ( 121.6456214775786293, 0.4262465694468514643, -12.03445270309931736 ) ) ;
#34912 = CARTESIAN_POINT ( 'NONE',  ( 118.9227414775786542, 0.4262465694468514643, -12.03445270309931736 ) ) ;
#34913 = CARTESIAN_POINT ( 'NONE',  ( 113.3068014775786594, -1.833838273342658809, -17.42832698103878286 ) ) ;
#34914 = ORIENTED_EDGE ( 'NONE', *, *, #20999, .F. ) ;
#34915 = CARTESIAN_POINT ( 'NONE',  ( 67.30914723170953096, -59.73653352439050934, -37.99192222348830938 ) ) ;
#34916 = CIRCLE ( 'NONE', #37943, 3.099999999999998757 ) ;
#34917 = EDGE_CURVE ( 'NONE', #11067, #37731, #27146, .T. ) ;
#34918 = CARTESIAN_POINT ( 'NONE',  ( 67.72463061902256243, -68.06054142010196983, -39.76798576395498941 ) ) ;
#34919 = CARTESIAN_POINT ( 'NONE',  ( 114.4413348109119823, -0.8288870151387760510, -10.36305467784173118 ) ) ;
#34920 = EDGE_LOOP ( 'NONE', ( #15260, #37358, #25339, #41171, #27371, #9619, #5652 ) ) ;
#34921 =( REPRESENTATION_RELATIONSHIP ('NONE','NONE', #36667, #15458 ) REPRESENTATION_RELATIONSHIP_WITH_TRANSFORMATION ( #29786 )SHAPE_REPRESENTATION_RELATIONSHIP( ) );
#34922 = VECTOR ( 'NONE', #25265, 1000.000000000000114 ) ;
#34923 = CARTESIAN_POINT ( 'NONE',  ( 77.77634386988383142, 3.254514819260860392, -4.893215200338314474 ) ) ;
#34924 = CARTESIAN_POINT ( 'NONE',  ( 109.5102233795247884, -1.325403438956436419, -9.854619843455211026 ) ) ;
#34925 = ORIENTED_EDGE ( 'NONE', *, *, #32432, .T. ) ;
#34926 = CARTESIAN_POINT ( 'NONE',  ( 120.3976348109119812, -7.643976991954077427, -18.09477374809248928 ) ) ;
#34927 = CARTESIAN_POINT ( 'NONE',  ( 113.3068014775786594, -1.833838273342658809, -17.42832698103878286 ) ) ;
#34928 = CARTESIAN_POINT ( 'NONE',  ( 115.0086014775786509, -4.089484607189486809, -7.948022111789456723 ) ) ;
#34929 = CARTESIAN_POINT ( 'NONE',  ( 122.8688454359119646, -11.07370829466463569, -12.81314460846529002 ) ) ;
#34930 = ORIENTED_EDGE ( 'NONE', *, *, #2187, .T. ) ;
#34931 = DIRECTION ( 'NONE',  ( 0.000000000000000000, 0.6004852223388321697, -0.7996358532186279566 ) ) ;
#34932 = CARTESIAN_POINT ( 'NONE',  ( 125.0532895624263432, -0.4468654995609705471, -7.300568634099578347 ) ) ;
#34933 = CARTESIAN_POINT ( 'NONE',  ( 116.0388171295248014, -10.62599879583958540, -13.39321520033831447 ) ) ;
#34934 = AXIS2_PLACEMENT_3D ( 'NONE', #13688, #10266, #10929 ) ;
#34935 = CARTESIAN_POINT ( 'NONE',  ( 112.7962614775786676, -3.383040157471821630, -19.15922257007629170 ) ) ;
#34936 = CARTESIAN_POINT ( 'NONE',  ( 122.3263414775786373, -3.505236298600246325, -18.68346056562440793 ) ) ;
#34937 = CARTESIAN_POINT ( 'NONE',  ( 118.5256548109119876, -8.899110576539710493, -16.42337572283490132 ) ) ;
#34938 = CARTESIAN_POINT ( 'NONE',  ( 119.7535502067644444, -1.223627541775746730, -16.99192386690446810 ) ) ;
#34939 = VERTEX_POINT ( 'NONE', #2509 ) ;
#34940 = CARTESIAN_POINT ( 'NONE',  ( 115.7460481442453357, -10.15424416112533912, -14.75197769757731336 ) ) ;
#34941 = CARTESIAN_POINT ( 'NONE',  ( 119.7434548109119987, -3.285100104180844305, -18.74292181979904726 ) ) ;
#34942 = VECTOR ( 'NONE', #32174, 1000.000000000000114 ) ;
#34943 = CARTESIAN_POINT ( 'NONE',  ( 65.06330879403716949, -35.71473443186641816, -5.721420406450495655 ) ) ;
#34944 = CARTESIAN_POINT ( 'NONE',  ( 79.00611218289952831, -44.99489077589586827, -23.89321520033831803 ) ) ;
#34945 = CARTESIAN_POINT ( 'NONE',  ( 116.1431348109119881, -10.30919188438810075, -12.61870101168855918 ) ) ;
#34946 = VERTEX_POINT ( 'NONE', #30112 ) ;
#34947 = VECTOR ( 'NONE', #2090, 1000.000000000000000 ) ;
#34948 = CARTESIAN_POINT ( 'NONE',  ( 113.2500748109119968, -6.344957434206662583, -7.627207830600332805 ) ) ;
#34949 = CARTESIAN_POINT ( 'NONE',  ( 112.9828796295247884, -4.863998795839590272, -19.15521520033831493 ) ) ;
#34950 = CARTESIAN_POINT ( 'NONE',  ( 112.6828081442453282, -7.893985811506177619, -18.51759400769804742 ) ) ;
#34951 = CARTESIAN_POINT ( 'NONE',  ( 114.9518748109119883, -1.834011780172310813, -8.268836392978581529 ) ) ;
#34952 = CARTESIAN_POINT ( 'NONE',  ( 124.4252281442452812, -0.8288870151387760510, -10.36305467784173118 ) ) ;
#34953 = CARTESIAN_POINT ( 'NONE',  ( 62.93082072130040672, -14.63772337389976208, -17.27340791136839471 ) ) ;
#34954 = CARTESIAN_POINT ( 'NONE',  ( 112.1494421295248003, -9.868328341294093420, -13.39321520033831447 ) ) ;
#34955 = CARTESIAN_POINT ( 'NONE',  ( 117.2776681442452968, -5.638512984489023161, -18.83840828888716601 ) ) ;
#34956 = CARTESIAN_POINT ( 'NONE',  ( 109.2295631630446593, -8.625464214188930612, -17.23631248896216661 ) ) ;
#34957 = CARTESIAN_POINT ( 'NONE',  ( 115.5191414775786569, -6.222761293078241884, -8.102969835052219238 ) ) ;
#34958 = CARTESIAN_POINT ( 'NONE',  ( 107.4960827545248350, -2.477300249445798297, -19.15521520033831138 ) ) ;
#34959 = CARTESIAN_POINT ( 'NONE',  ( 114.5803015045248117, -6.936859964151250502, -18.39754474579286025 ) ) ;
#34960 = CARTESIAN_POINT ( 'NONE',  ( 110.6909265045248247, -7.250697342233347165, -19.15521520033831138 ) ) ;
#34961 = CARTESIAN_POINT ( 'NONE',  ( 127.0298367773237089, -5.162954104783970877, -7.995796553879564783 ) ) ;
#34962 = CARTESIAN_POINT ( 'NONE',  ( 126.2404814775786264, -9.261995988541697145, -16.69588392320189030 ) ) ;
#34963 = CARTESIAN_POINT ( 'NONE',  ( 75.95778847736514194, -3.256761025687008537, -16.39321520033831447 ) ) ;
#34964 = CARTESIAN_POINT ( 'NONE',  ( 123.5176014775786228, -9.261995988541697145, -16.69588392320189030 ) ) ;
#34965 = CARTESIAN_POINT ( 'NONE',  ( 116.1431348109119881, -10.30919188438810075, -12.61870101168855918 ) ) ;
#34966 = ORIENTED_EDGE ( 'NONE', *, *, #35754, .F. ) ;
#34967 = CARTESIAN_POINT ( 'NONE',  ( 114.7816948109119863, -9.859900752359374465, -12.68260735090039404 ) ) ;
#34968 = DIRECTION ( 'NONE',  ( 0.7871354856660167654, -0.6167752151498625546, -0.002461946824136807422 ) ) ;
#34969 = VECTOR ( 'NONE', #9310, 1000.000000000000000 ) ;
#34970 = CARTESIAN_POINT ( 'NONE',  ( 116.5969481442453031, 0.5811942927096154232, -14.16772938898807155 ) ) ;
#34971 = CARTESIAN_POINT ( 'NONE',  ( 116.7104014775786425, -8.899110576539710493, -16.42337572283490132 ) ) ;
#34972 = ORIENTED_EDGE ( 'NONE', *, *, #23975, .T. ) ;
#34973 = CARTESIAN_POINT ( 'NONE',  ( 119.9438214775786378, -2.084020599724406786, -8.691656652584148546 ) ) ;
#34974 = VECTOR ( 'NONE', #32514, 1000.000000000000000 ) ;
#34975 = CARTESIAN_POINT ( 'NONE',  ( 117.9016614775786280, -9.988377603198976828, -10.36322818467138340 ) ) ;
#34976 = CARTESIAN_POINT ( 'NONE',  ( 137.4406106298543193, 0.07373545144022489173, -14.57874919129496583 ) ) ;
#34977 = CARTESIAN_POINT ( 'NONE',  ( 112.2188952545247531, 0.8980012041604421569, -11.00651665394454071 ) ) ;
#34978 = CIRCLE ( 'NONE', #16841, 2.000000000000000444 ) ;
#34979 = CARTESIAN_POINT ( 'NONE',  ( 63.42533636626423998, -3.154224173321905855, -7.672534579508055508 ) ) ;
#34980 = DIRECTION ( 'NONE',  ( 0.000000000000000000, 0.000000000000000000, 1.000000000000000000 ) ) ;
#34981 = CARTESIAN_POINT ( 'NONE',  ( 117.0806140045248185, 0.1403307496149616695, -15.46607636864997204 ) ) ;
#34982 = CARTESIAN_POINT ( 'NONE',  ( 113.0231681442453322, 0.9020085738987339008, -11.91225656197089222 ) ) ;
#34983 = CARTESIAN_POINT ( 'NONE',  ( 137.1799701741867921, -10.18481525785750819, -13.59600295436091066 ) ) ;
#34984 = CARTESIAN_POINT ( 'NONE',  ( 113.8173414775786512, -9.565557343593413364, -10.61323700422348004 ) ) ;
#34985 = DIRECTION ( 'NONE',  ( 0.000000000000000000, 0.000000000000000000, -1.000000000000000000 ) ) ;
#34986 = LINE ( 'NONE', #15623, #43325 ) ;
#34987 = CARTESIAN_POINT ( 'NONE',  ( 115.0664733795247798, -1.325403438956436419, -9.854619843455211026 ) ) ;
#34988 = CARTESIAN_POINT ( 'NONE',  ( 122.3620835773848654, -2.467220198592778413, -17.83387418641524391 ) ) ;
#34989 = CARTESIAN_POINT ( 'NONE',  ( 123.5393205993907486, -9.245649465415468171, -16.16453161350215950 ) ) ;
#34990 = AXIS2_PLACEMENT_3D ( 'NONE', #5195, #2001, #22983 ) ;
#34991 = DIRECTION ( 'NONE',  ( 1.000000000000000000, 0.000000000000000000, 0.000000000000000000 ) ) ;
#34993 = CARTESIAN_POINT ( 'NONE',  ( 116.4267681442453153, -3.383040157471821630, -19.15922257007629170 ) ) ;
#34992 = CARTESIAN_POINT ( 'NONE',  ( 119.7434548109119703, -4.863998795839242995, -13.39321520033831447 ) ) ;
#34994 = CARTESIAN_POINT ( 'NONE',  ( 123.1772414775786189, -5.574606645277164318, -18.38911715685844683 ) ) ;
#34995 = CARTESIAN_POINT ( 'NONE',  ( 118.3554748109119998, -9.565557343593413364, -10.61323700422348004 ) ) ;
#34996 = EDGE_LOOP ( 'NONE', ( #6687, #57 ) ) ;
#34997 = CARTESIAN_POINT ( 'NONE',  ( 136.3514896075744218, -9.407894941071146988, -9.767453091696252088 ) ) ;
#34998 = CARTESIAN_POINT ( 'NONE',  ( 123.9714148109119805, -0.4660016031367893996, -10.09054647747474043 ) ) ;
#34999 = CARTESIAN_POINT ( 'NONE',  ( 116.5944421295247793, -9.868328341294093420, -13.39321520033831447 ) ) ;
#35000 = CARTESIAN_POINT ( 'NONE',  ( 113.9875214775786532, -8.899110576539710493, -16.42337572283490132 ) ) ;
#35001 = EDGE_CURVE ( 'NONE', #30513, #20890, #43800, .T. ) ;
#35002 = CARTESIAN_POINT ( 'NONE',  ( 111.8886348109120092, -6.222761293078241884, -8.102969835052219238 ) ) ;
#35003 = CARTESIAN_POINT ( 'NONE',  ( 85.40866212614237440, -28.66666519958388193, -9.415214268655820007 ) ) ;
#35004 = CARTESIAN_POINT ( 'NONE',  ( 110.6909265045248247, -7.250697342233347165, -19.15521520033831138 ) ) ;
#35005 = CARTESIAN_POINT ( 'NONE',  ( 119.2631014775786298, -9.565557343593413364, -10.61323700422348004 ) ) ;
#35006 = VECTOR ( 'NONE', #29954, 1000.000000000000227 ) ;
#35007 = CARTESIAN_POINT ( 'NONE',  ( 120.5110881442453206, -3.505236298600246325, -18.68346056562440793 ) ) ;
#35008 = CARTESIAN_POINT ( 'NONE',  ( 115.8998954522301830, 0.1168444861213632779, -14.64321520033831447 ) ) ;
#35009 = CARTESIAN_POINT ( 'NONE',  ( 109.2291353395606421, 0.1491742553690190431, -11.67757420713069649 ) ) ;
#35010 = CARTESIAN_POINT ( 'NONE',  ( 81.52050388106540879, 0.5255923868638483487, -10.39321520033831625 ) ) ;
#35011 = CARTESIAN_POINT ( 'NONE',  ( 108.7462390045248242, -9.868328341294098749, -11.32035403202665869 ) ) ;
#35012 = CIRCLE ( 'NONE', #19755, 8.000000000000001776 ) ;
#35013 = PRODUCT ( 'Body4', 'Body4', '', ( #25923 ) ) ;
#35014 = CARTESIAN_POINT ( 'NONE',  ( 116.6166916131588351, 2.139222853825150761, -20.64615525626918213 ) ) ;
#35015 = CARTESIAN_POINT ( 'NONE',  ( 118.4689281442453392, 0.9020085738987339008, -11.91225656197089222 ) ) ;
#35016 = CARTESIAN_POINT ( 'NONE',  ( 113.4202548109119846, -10.30919188438810075, -12.61870101168855918 ) ) ;
#35017 = CARTESIAN_POINT ( 'NONE',  ( 111.0381921295247878, 0.8980012041604618078, -13.39321520033831447 ) ) ;
#35018 = LINE ( 'NONE', #41244, #17024 ) ;
#35019 = VERTEX_POINT ( 'NONE', #12790 ) ;
#35020 = DIRECTION ( 'NONE',  ( -0.9495615000563050190, 0.3135808629537517600, 0.000000000000000000 ) ) ;
#35021 = CARTESIAN_POINT ( 'NONE',  ( 123.6310548109119765, -5.638512984488999180, -18.83840828888717311 ) ) ;
#35022 = CARTESIAN_POINT ( 'NONE',  ( 112.5126281442453120, -10.30919188438810075, -12.61870101168855918 ) ) ;
#35023 = CARTESIAN_POINT ( 'NONE',  ( 121.4754414775786131, -1.833838273342659697, -17.42832698103878286 ) ) ;
#35024 =( NAMED_UNIT ( * ) SI_UNIT ( $, .STERADIAN. ) SOLID_ANGLE_UNIT ( ) );
#35025 = CARTESIAN_POINT ( 'NONE',  ( 123.7445081442452874, -1.561330072975668948, -17.79121239304076951 ) ) ;
#35026 = CARTESIAN_POINT ( 'NONE',  ( 120.6245414775786458, -9.988377603198976828, -10.36322818467138340 ) ) ;
#35027 = EDGE_CURVE ( 'NONE', #10427, #7998, #9363, .T. ) ;
#35028 = CARTESIAN_POINT ( 'NONE',  ( 109.4407702545248355, 0.1403307496149616695, -11.32035403202665336 ) ) ;
#35029 = AXIS2_PLACEMENT_3D ( 'NONE', #9827, #33742, #33972 ) ;
#35030 = CARTESIAN_POINT ( 'NONE',  ( 117.0507614775786465, 0.1319031606808879209, -14.10382304977623669 ) ) ;
#35031 = CARTESIAN_POINT ( 'NONE',  ( 89.01247232317646763, -25.23119213852205789, -15.24166438581092109 ) ) ;
#35032 = ORIENTED_EDGE ( 'NONE', *, *, #43690, .F. ) ;
#35033 = CARTESIAN_POINT ( 'NONE',  ( 121.0783548109119749, 0.2603800115204892296, -16.42320221600525088 ) ) ;
#35034 = EDGE_CURVE ( 'NONE', #930, #2865, #13016, .T. ) ;
#35035 = CARTESIAN_POINT ( 'NONE',  ( 83.16394245587648015, -30.76310523276723785, -20.89321520033831447 ) ) ;
#35036 = EDGE_CURVE ( 'NONE', #42739, #7998, #40374, .T. ) ;
#35037 = CARTESIAN_POINT ( 'NONE',  ( 116.7104014775786425, -0.4660016031367893996, -10.09054647747474043 ) ) ;
#35038 = ORIENTED_EDGE ( 'NONE', *, *, #11170, .F. ) ;
#35039 = CARTESIAN_POINT ( 'NONE',  ( 106.8710046295248759, -4.863998795839590272, -18.39754474579285315 ) ) ;
#35040 = AXIS2_PLACEMENT_3D ( 'NONE', #23325, #37682, #6680 ) ;
#35041 = CARTESIAN_POINT ( 'NONE',  ( 125.9001214775786224, -4.089484607189486809, -7.948022111789456723 ) ) ;
#35042 = CARTESIAN_POINT ( 'NONE',  ( 122.8176765460471955, -2.191907684172563986, -18.20049396185734025 ) ) ;
#35043 = CARTESIAN_POINT ( 'NONE',  ( 116.0864081442453113, -0.1624402480850797581, -16.17319339645315424 ) ) ;
#35044 = CARTESIAN_POINT ( 'NONE',  ( 69.36136150295220659, -101.1685209014307674, -50.56525720990386219 ) ) ;
#35045 = CARTESIAN_POINT ( 'NONE',  ( 120.4543614775786295, -5.574606645277164318, -18.38911715685844683 ) ) ;
#35046 = CARTESIAN_POINT ( 'NONE',  ( 70.19189222814998175, -61.69445140165969121, -37.88057465812982372 ) ) ;
#35047 = EDGE_CURVE ( 'NONE', #25300, #34550, #20849, .T. ) ;
#35048 = CARTESIAN_POINT ( 'NONE',  ( 122.3263414775786373, -3.505236298600246325, -18.68346056562440793 ) ) ;
#35049 = CARTESIAN_POINT ( 'NONE',  ( 124.7472578386052362, -11.05872435226744344, -8.686341302686004795 ) ) ;
#35050 = CARTESIAN_POINT ( 'NONE',  ( 118.1852948109119836, -4.153390946401325223, -8.397313243818185668 ) ) ;
#35051 = EDGE_CURVE ( 'NONE', #36955, #43140, #9289, .T. ) ;
#35052 = CARTESIAN_POINT ( 'NONE',  ( 120.6463454359119822, -11.07370829466463569, -12.81314460846529002 ) ) ;
#35053 = CARTESIAN_POINT ( 'NONE',  ( 115.7460481442453357, 0.9020085738987339008, -11.91225656197089222 ) ) ;
#35054 = DIRECTION ( 'NONE',  ( 0.000000000000000000, 0.4669533266896289669, 0.8842819633428518067 ) ) ;
#35055 = EDGE_CURVE ( 'NONE', #14177, #36847, #16354, .T. ) ;
#35056 = EDGE_CURVE ( 'NONE', #5805, #31941, #5610, .T. ) ;
#35057 = CARTESIAN_POINT ( 'NONE',  ( 122.0994348109119443, -10.15424416112533912, -14.75197769757731336 ) ) ;
#35058 = VERTEX_POINT ( 'NONE', #37541 ) ;
#35059 = CARTESIAN_POINT ( 'NONE',  ( 117.7314814775786260, -4.089484607189486809, -7.948022111789456723 ) ) ;
#35060 = CARTESIAN_POINT ( 'NONE',  ( 106.3153796295248412, -4.863998795839590272, -19.15521520033831493 ) ) ;
#35061 = CARTESIAN_POINT ( 'NONE',  ( 115.4056881442453317, -2.084020599724388578, -8.691656652584157428 ) ) ;
#35062 = DIRECTION ( 'NONE',  ( 0.000000000000000000, -0.3818493186865927203, 0.9242245927363029745 ) ) ;
#35063 = CIRCLE ( 'NONE', #44584, 3.000000000000002665 ) ;
#35064 = CARTESIAN_POINT ( 'NONE',  ( 113.5886041094426844, 0.3591747506842615789, -12.14321520033833046 ) ) ;
#35065 = CARTESIAN_POINT ( 'NONE',  ( 121.6456214775786293, -10.63000616557722466, -14.87417383870573495 ) ) ;
#35066 = ORIENTED_EDGE ( 'NONE', *, *, #26137, .F. ) ;
#35067 = CARTESIAN_POINT ( 'NONE',  ( 128.2184548109119930, -10.81584935473217080, -14.15181583611863303 ) ) ;
#35068 = CARTESIAN_POINT ( 'NONE',  ( 117.5045748109119756, -9.859900752359374465, -12.68260735090039404 ) ) ;
#35069 = FACE_OUTER_BOUND ( 'NONE', #19255, .T. ) ;
#35070 = CARTESIAN_POINT ( 'NONE',  ( 109.2309317933750634, -1.356617975920010322, -16.96302509418498161 ) ) ;
#35071 = CARTESIAN_POINT ( 'NONE',  ( 120.4470390828414139, -8.372502050422339082, -17.31760344562335519 ) ) ;
#35072 = CARTESIAN_POINT ( 'NONE',  ( 110.4131140045248287, 0.1403307496149616695, -15.46607636864997204 ) ) ;
#35073 = DIRECTION ( 'NONE',  ( 1.000000000000000000, 0.000000000000000000, -0.000000000000000000 ) ) ;
#35074 = EDGE_LOOP ( 'NONE', ( #18226, #34128, #31528, #29915, #35407 ) ) ;
#35075 = CARTESIAN_POINT ( 'NONE',  ( 115.0653281442453277, -6.344957434206662583, -7.627207830600332805 ) ) ;
#35076 = CIRCLE ( 'NONE', #15448, 4.999999999999998224 ) ;
#35077 = CARTESIAN_POINT ( 'NONE',  ( 111.9453614775786434, -1.561330072975668060, -17.79121239304076596 ) ) ;
#35078 = CARTESIAN_POINT ( 'NONE',  ( 122.9503348109119827, 0.5811942927096110934, -14.16772938898807510 ) ) ;
#35079 = CARTESIAN_POINT ( 'NONE',  ( 116.8805814775786445, -3.505236298600246325, -18.68346056562440793 ) ) ;
#35080 = CARTESIAN_POINT ( 'NONE',  ( 119.7434548109119703, 2.753894863294152007, -15.83610205775420177 ) ) ;
#35081 = FILL_AREA_STYLE ('',( #14585 ) ) ;
#35082 = CARTESIAN_POINT ( 'NONE',  ( 120.7947214775786193, -9.261995988541697145, -16.69588392320189030 ) ) ;
#35083 = CARTESIAN_POINT ( 'NONE',  ( 111.5020881442453202, -0.2054726073303936307, -16.14774885094461965 ) ) ;
#35084 = CARTESIAN_POINT ( 'NONE',  ( 63.17554510063945372, -31.34889167039416691, -21.89321520033831092 ) ) ;
#35085 = CARTESIAN_POINT ( 'NONE',  ( 93.93057702947278642, -25.99489077589524300, -13.39321520033831447 ) ) ;
#35086 = CARTESIAN_POINT ( 'NONE',  ( 121.8158014775786171, -4.153390946401325223, -8.397313243818185668 ) ) ;
#35087 = EDGE_LOOP ( 'NONE', ( #29287, #30192, #40119, #12 ) ) ;
#35088 = DIRECTION ( 'NONE',  ( 0.000000000000000000, 0.000000000000000000, 1.000000000000000000 ) ) ;
#35089 = CARTESIAN_POINT ( 'NONE',  ( 116.5402214775786405, 0.2603800115204892296, -16.42320221600525088 ) ) ;
#35090 = CARTESIAN_POINT ( 'NONE',  ( 125.3895814775786448, -2.084020599724406786, -8.691656652584148546 ) ) ;
#35091 = ORIENTED_EDGE ( 'NONE', *, *, #10044, .F. ) ;
#35092 = CARTESIAN_POINT ( 'NONE',  ( 136.2315975805936148, 0.5549518486163793618, -11.18187001423429727 ) ) ;
#35093 = CARTESIAN_POINT ( 'NONE',  ( 120.7379948109119709, -10.63000616557722466, -14.87417383870573495 ) ) ;
#35094 = AXIS2_PLACEMENT_3D ( 'NONE', #18948, #16614, #27096 ) ;
#35095 = CARTESIAN_POINT ( 'NONE',  ( 108.6767858795247861, -0.7896495226426338832, -17.46756447353520159 ) ) ;
#35096 = CARTESIAN_POINT ( 'NONE',  ( 119.3765548109119834, -10.15424416112533912, -14.75197769757731336 ) ) ;
#35097 = ORIENTED_EDGE ( 'NONE', *, *, #19220, .T. ) ;
#35098 = CIRCLE ( 'NONE', #35827, 1.009117809157100254 ) ;
#35099 = CARTESIAN_POINT ( 'NONE',  ( 114.4980614775786592, -7.893985811506177619, -18.51759400769804742 ) ) ;
#35100 = CARTESIAN_POINT ( 'NONE',  ( 123.9146881442452894, -10.15424416112533912, -14.75197769757731336 ) ) ;
#35101 = CARTESIAN_POINT ( 'NONE',  ( 79.52666107723024425, 5.086845235696775269, -20.29072895152215494 ) ) ;
#35102 = AXIS2_PLACEMENT_3D ( 'NONE', #28676, #15434, #35944 ) ;
#35103 = CARTESIAN_POINT ( 'NONE',  ( -6.962123463324043193, -11.49046785505262136, -8.593215200338315540 ) ) ;
#35104 = CARTESIAN_POINT ( 'NONE',  ( 124.9924948109119924, -4.089484607189486809, -7.948022111789456723 ) ) ;
#35105 = EDGE_CURVE ( 'NONE', #16022, #30207, #22732, .T. ) ;
#35106 = CARTESIAN_POINT ( 'NONE',  ( 122.8775937114597241, -6.208002839291213881, -18.65814938918611077 ) ) ;
#35107 = CONICAL_SURFACE ( 'NONE', #43147, 2.445500000000004448, 0.9599310885968757034 ) ;
#35108 = CARTESIAN_POINT ( 'NONE',  ( 105.2294421295247844, -9.051693226400931991, -21.89321520033831447 ) ) ;
#35109 = CARTESIAN_POINT ( 'NONE',  ( 123.9146881442452894, 0.9020085738987339008, -11.91225656197089222 ) ) ;
#35111 = CARTESIAN_POINT ( 'NONE',  ( 122.3830681442452857, -1.833838273342659697, -17.42832698103878286 ) ) ;
#35110 = CARTESIAN_POINT ( 'NONE',  ( 122.3830681442452857, -8.166667518702819706, -8.995218007635861213 ) ) ;
#35112 = CARTESIAN_POINT ( 'NONE',  ( 120.6245414775786458, -0.1624402480850797581, -16.17319339645315424 ) ) ;
#35113 = DIRECTION ( 'NONE',  ( -0.7871354856660202071, 0.6167752151498580027, 0.002461946824133919541 ) ) ;
#35114 = CARTESIAN_POINT ( 'NONE',  ( 115.9729548109119861, -6.344957434206662583, -7.627207830600332805 ) ) ;
#35115 = VERTEX_POINT ( 'NONE', #44402 ) ;
#35116 = CARTESIAN_POINT ( 'NONE',  ( 116.0842780030094872, -0.02021311778663964498, -12.14321520033831625 ) ) ;
#35117 = CARTESIAN_POINT ( 'NONE',  ( 105.8292077545248446, -7.250697342233347165, -7.631215200338321125 ) ) ;
#35118 = CARTESIAN_POINT ( 'NONE',  ( 110.0658483795247804, -8.402594152722688392, -16.93181055722141792 ) ) ;
#35119 = CARTESIAN_POINT ( 'NONE',  ( 115.0664733795247798, -1.325403438956436419, -9.854619843455211026 ) ) ;
#35120 = CARTESIAN_POINT ( 'NONE',  ( 125.1059481442452750, -8.166667518702819706, -8.995218007635861213 ) ) ;
#35121 = CARTESIAN_POINT ( 'NONE',  ( 125.9568481442452850, -3.505236298600246325, -18.68346056562440793 ) ) ;
#35122 = EDGE_LOOP ( 'NONE', ( #33546, #6171, #1957, #12141 ) ) ;
#35123 = CARTESIAN_POINT ( 'NONE',  ( 113.8740681442453138, -9.859900752359374465, -12.68260735090039404 ) ) ;
#35124 = CARTESIAN_POINT ( 'NONE',  ( 113.8163171295247764, -10.62599879583958540, -13.39321520033831447 ) ) ;
#35125 = CARTESIAN_POINT ( 'NONE',  ( 61.73532138647689038, -39.51680623670656445, -6.460275505913305238 ) ) ;
#35126 = ADVANCED_FACE ( 'NONE', ( #6313 ), #42766, .T. ) ;
#35127 = CARTESIAN_POINT ( 'NONE',  ( 123.6877814775786533, -3.383040157471821630, -19.15922257007629170 ) ) ;
#35128 = CARTESIAN_POINT ( 'NONE',  ( 125.4463081442452932, -5.638512984488999180, -18.83840828888717311 ) ) ;
#35129 = CARTESIAN_POINT ( 'NONE',  ( -12.36826994950264513, -4.374949827406456215, -19.39321520033831447 ) ) ;
#35130 = CARTESIAN_POINT ( 'NONE',  ( 116.1431348109119881, -10.30919188438810075, -12.61870101168855918 ) ) ;
#35131 = VECTOR ( 'NONE', #33014, 1000.000000000000114 ) ;
#35132 = CARTESIAN_POINT ( 'NONE',  ( 114.0246765045248196, -7.250697342233347165, -19.15521520033831138 ) ) ;
#35133 = CARTESIAN_POINT ( 'NONE',  ( 114.4413952545248350, -9.868328341294098749, -15.46607636864997204 ) ) ;
#35134 = VERTEX_POINT ( 'NONE', #26388 ) ;
#35135 = CYLINDRICAL_SURFACE ( 'NONE', #7761, 0.8718221387495478369 ) ;
#35136 = CARTESIAN_POINT ( 'NONE',  ( 115.4056881442453459, -2.084020599724406786, -8.691656652584148546 ) ) ;
#35137 = AXIS2_PLACEMENT_3D ( 'NONE', #42512, #1000, #28156 ) ;
#35138 = CARTESIAN_POINT ( 'NONE',  ( 113.4769814775786330, -10.63000616557722466, -14.87417383870573495 ) ) ;
#35139 = B_SPLINE_CURVE_WITH_KNOTS ( 'NONE', 3,
 ( #39282, #8047, #35844, #4617, #18538, #32429, #10581, #24481, #11922, #36521, #22176, #29024, #25822 ),
 .UNSPECIFIED., .F., .F.,
 ( 4, 3, 3, 3, 4 ),
 ( 1.568264261493034943E-06, 2.784814680393055196E-05, 5.575405619718069985E-05, 9.782819182226189052E-05, 0.0001187612790815211953 ),
 .UNSPECIFIED. ) ;
#35140 = CARTESIAN_POINT ( 'NONE',  ( 114.0941296295247867, -4.863998795839590272, -19.15521520033831493 ) ) ;
#35141 = FACE_OUTER_BOUND ( 'NONE', #8958, .T. ) ;
#35142 = CARTESIAN_POINT ( 'NONE',  ( 120.7947214775786193, -0.8288870151387760510, -10.36305467784173118 ) ) ;
#35143 = UNCERTAINTY_MEASURE_WITH_UNIT (LENGTH_MEASURE( 1.000000000000000082E-05 ), #10523, 'distance_accuracy_value', 'NONE');
#35144 = CARTESIAN_POINT ( 'NONE',  ( 120.6812681442452941, 0.1319031606808879209, -14.10382304977623669 ) ) ;
#35145 = CARTESIAN_POINT ( 'NONE',  ( 126.2404814775786264, -9.261995988541697145, -16.69588392320189030 ) ) ;
#35146 = VERTEX_POINT ( 'NONE', #19322 ) ;
#35147 = STYLED_ITEM ( 'NONE', ( #7235 ), #24824 ) ;
#35148 = CARTESIAN_POINT ( 'NONE',  ( 124.4252281442452812, -0.8288870151387760510, -10.36305467784173118 ) ) ;
#35149 = CARTESIAN_POINT ( 'NONE',  ( 88.07785292173620917, -26.60966817898065884, -11.90521360603286816 ) ) ;
#35150 = CARTESIAN_POINT ( 'NONE',  ( 113.4769814775786330, 0.4262465694468514643, -12.03445270309931736 ) ) ;
#35151 = ORIENTED_EDGE ( 'NONE', *, *, #9703, .T. ) ;
#35152 = CARTESIAN_POINT ( 'NONE',  ( 126.3999550322210155, -9.219482243445801473, -16.02874797595598366 ) ) ;
#35153 = CARTESIAN_POINT ( 'NONE',  ( 87.41631446019775353, -25.38011337280982715, -14.88121679464376257 ) ) ;
#35154 = CARTESIAN_POINT ( 'NONE',  ( 112.4967077545247633, -2.791137627527939813, -18.39754474579286025 ) ) ;
#35155 = ORIENTED_EDGE ( 'NONE', *, *, #40638, .T. ) ;
#35156 = CARTESIAN_POINT ( 'NONE',  ( 117.6747548109119919, -7.643976991954077427, -18.09477374809248928 ) ) ;
#35157 = CARTESIAN_POINT ( 'NONE',  ( 114.7816948109119863, -9.859900752359374465, -12.68260735090039404 ) ) ;
#35158 = CARTESIAN_POINT ( 'NONE',  ( 124.5817866277113382, -9.804771881367848607, -14.18055866627750738 ) ) ;
#35159 = EDGE_CURVE ( 'NONE', #4412, #11942, #2430, .T. ) ;
#35160 = CARTESIAN_POINT ( 'NONE',  ( 123.9800954359119771, -11.07370829466463569, -12.81314460846529002 ) ) ;
#35161 = ORIENTED_EDGE ( 'NONE', *, *, #40713, .F. ) ;
#35162 = AXIS2_PLACEMENT_3D ( 'NONE', #2926, #20715, #34595 ) ;
#35163 = CARTESIAN_POINT ( 'NONE',  ( 83.82415148905927538, -46.76310523276723785, -6.893215200338315363 ) ) ;
#35164 = CARTESIAN_POINT ( 'NONE',  ( 124.9774582099985025, -0.3480505516612068528, -7.274636164916885583 ) ) ;
#35165 = CARTESIAN_POINT ( 'NONE',  ( 106.3848327545248651, -6.936859964151250502, -8.388885654883777576 ) ) ;
#35166 = AXIS2_PLACEMENT_3D ( 'NONE', #40666, #9418, #44321 ) ;
#35167 = CARTESIAN_POINT ( 'NONE',  ( 113.6471614775786492, -5.638512984488999180, -18.83840828888717311 ) ) ;
#35168 = CARTESIAN_POINT ( 'NONE',  ( 124.9357681442453014, -7.643976991954077427, -18.09477374809248928 ) ) ;
#35169 = CARTESIAN_POINT ( 'NONE',  ( 116.1431348109119881, 0.1319031606808879209, -14.10382304977623669 ) ) ;
#35170 = CARTESIAN_POINT ( 'NONE',  ( 70.19189222814998175, -53.54563792646638376, -34.62107767336419073 ) ) ;
#35171 = VERTEX_POINT ( 'NONE', #22962 ) ;
#35172 = CARTESIAN_POINT ( 'NONE',  ( 117.7314814775786260, -5.574606645277164318, -18.38911715685844683 ) ) ;
#35173 = CARTESIAN_POINT ( 'NONE',  ( 116.5249890045247980, 0.8980012041604421569, -15.77991374673208469 ) ) ;
#35174 = CARTESIAN_POINT ( 'NONE',  ( 85.02738910321417620, -28.58808629434043524, -8.794714412758365185 ) ) ;
#35175 = CARTESIAN_POINT ( 'NONE',  ( 116.3860827545247787, -2.477300249445798297, -19.15521520033831138 ) ) ;
#35176 = EDGE_CURVE ( 'NONE', #5526, #23066, #7807, .T. ) ;
#35177 = CARTESIAN_POINT ( 'NONE',  ( 115.0653281442453277, -6.344957434206662583, -7.627207830600332805 ) ) ;
#35178 = EDGE_LOOP ( 'NONE', ( #15988, #32955, #3726, #37445 ) ) ;
#35179 = CARTESIAN_POINT ( 'NONE',  ( 116.9373081442452929, -8.166667518702817929, -8.995218007635861213 ) ) ;
#35180 = CARTESIAN_POINT ( 'NONE',  ( 114.2711548109119946, -9.988377603198976828, -10.36322818467138340 ) ) ;
#35181 = CARTESIAN_POINT ( 'NONE',  ( 112.7745202545247878, -10.62599879583958717, -15.77991374673208469 ) ) ;
#35182 = CARTESIAN_POINT ( 'NONE',  ( 112.1155414775786454, 0.9020085738987339008, -11.91225656197089222 ) ) ;
#35183 = CARTESIAN_POINT ( 'NONE',  ( 113.3635281442453504, -9.988377603198976828, -10.36322818467138340 ) ) ;
#35184 = DIRECTION ( 'NONE',  ( 0.000000000000000000, -1.000000000000000000, 0.000000000000000000 ) ) ;
#35185 = FACE_OUTER_BOUND ( 'NONE', #33566, .T. ) ;
#35186 = CARTESIAN_POINT ( 'NONE',  ( 111.3854577545248645, -2.791137627527939813, -18.39754474579286025 ) ) ;
#35188 = ORIENTED_EDGE ( 'NONE', *, *, #30594, .T. ) ;
#35187 = STYLED_ITEM ( 'NONE', ( #30292 ), #16689 ) ;
#35189 = CARTESIAN_POINT ( 'NONE',  ( 96.54708369096698561, -27.78532125115470208, -14.69016690077367926 ) ) ;
#35190 = CARTESIAN_POINT ( 'NONE',  ( 109.2294493580808989, -5.173074444957243223, -18.58748577876895425 ) ) ;
#35191 = CARTESIAN_POINT ( 'NONE',  ( 115.9162281442453235, -5.574606645277164318, -18.38911715685844683 ) ) ;
#35192 = B_SPLINE_CURVE_WITH_KNOTS ( 'NONE', 3,
 ( #16257, #43614, #41114, #16484, #30384, #44307, #37439, #6210, #30607, #44524 ),
 .UNSPECIFIED., .F., .F.,
 ( 4, 3, 3, 4 ),
 ( 3.127317220692749988E-18, 0.0002476486808869855175, 0.0004952973797228669853, 0.0009539399846111519445 ),
 .UNSPECIFIED. ) ;
#35193 = LINE ( 'NONE', #42743, #3722 ) ;
#35194 = CARTESIAN_POINT ( 'NONE',  ( 122.8169364575754798, -1.016270020561755860, -17.26805140881366896 ) ) ;
#35195 = CARTESIAN_POINT ( 'NONE',  ( 108.6767858795247861, -0.7896495226426338832, -17.46756447353520159 ) ) ;
#35196 = CARTESIAN_POINT ( 'NONE',  ( 127.2313854077063979, -5.268148382571362198, -7.901566705240425925 ) ) ;
#35197 = CARTESIAN_POINT ( 'NONE',  ( 125.4463081442452932, -5.638512984488999180, -18.83840828888717311 ) ) ;
#35198 = CARTESIAN_POINT ( 'NONE',  ( 138.2184548109119930, -2.520019956603805511, -15.26558354049377009 ) ) ;
#35199 =( BOUNDED_SURFACE ( )  B_SPLINE_SURFACE ( 1, 2, ( 
 ( #38971, #11617, #35993, #42411, #11175, #11398, #21204, #18465, #32355, #25307, #22105, #31905, #4764, #18233, #39201, #4082, #7740 ),
 ( #29163, #43077, #24850, #7288, #21651, #35083, #35542, #3863, #17785, #14364, #28278, #38742, #21427, #7512, #35311, #670, #2468 ) ),
 .UNSPECIFIED., .F., .F., .T. ) 
 B_SPLINE_SURFACE_WITH_KNOTS ( ( 2, 2 ),
 ( 3, 2, 2, 2, 2, 2, 2, 2, 3 ),
 ( 0.000000000000000000, 1.000000000000000000 ),
 ( 0.000000000000000000, 0.1250000000000000000, 0.2500000000000000000, 0.3750000000000000000, 0.5000000000000000000, 0.6250000000000000000, 0.7500000000000000000, 0.8750000000000000000, 1.000000000000000000 ),
 .UNSPECIFIED. ) 
 GEOMETRIC_REPRESENTATION_ITEM ( )  RATIONAL_B_SPLINE_SURFACE ( (
 ( 1.000000000000000000, 0.9238795325112869605, 1.000000000000000000, 0.9238795325112869605, 1.000000000000000000, 0.9238795325112869605, 1.000000000000000000, 0.9238795325112869605, 1.000000000000000000, 0.9238795325112869605, 1.000000000000000000, 0.9238795325112869605, 1.000000000000000000, 0.9238795325112869605, 1.000000000000000000, 0.9238795325112869605, 1.000000000000000000),
 ( 1.000000000000000000, 0.9238795325112869605, 1.000000000000000000, 0.9238795325112869605, 1.000000000000000000, 0.9238795325112869605, 1.000000000000000000, 0.9238795325112869605, 1.000000000000000000, 0.9238795325112869605, 1.000000000000000000, 0.9238795325112869605, 1.000000000000000000, 0.9238795325112869605, 1.000000000000000000, 0.9238795325112869605, 1.000000000000000000) ) ) 
 REPRESENTATION_ITEM ( '' )  SURFACE ( )  );
#35200 = CARTESIAN_POINT ( 'NONE',  ( 124.7088614775786226, 0.2603800115204892296, -16.42320221600525088 ) ) ;
#35201 = CARTESIAN_POINT ( 'NONE',  ( 115.0086014775786509, -4.089484607189486809, -7.948022111789456723 ) ) ;
#35202 = VERTEX_POINT ( 'NONE', #23197 ) ;
#35203 = CONICAL_SURFACE ( 'NONE', #39585, 2.000000000000000444, 0.9599310885968830309 ) ;
#35204 = CARTESIAN_POINT ( 'NONE',  ( 115.6893214775786447, -9.859900752359374465, -12.68260735090039404 ) ) ;
#35205 = CIRCLE ( 'NONE', #19830, 2.000000000000000444 ) ;
#35206 = CARTESIAN_POINT ( 'NONE',  ( 125.9001214775786224, -4.089484607189486809, -7.948022111789456723 ) ) ;
#35208 = EDGE_CURVE ( 'NONE', #37055, #11127, #40066, .T. ) ;
#35207 = CARTESIAN_POINT ( 'NONE',  ( 119.1496481442453046, -3.383040157471821630, -19.15922257007629170 ) ) ;
#35209 = CARTESIAN_POINT ( 'NONE',  ( 116.6536748109119941, -10.15424416112533912, -14.75197769757731336 ) ) ;
#35210 = ORIENTED_EDGE ( 'NONE', *, *, #18365, .T. ) ;
#35211 = CARTESIAN_POINT ( 'NONE',  ( 119.8870948109119752, -0.8288870151387760510, -10.36305467784173118 ) ) ;
#35212 = CIRCLE ( 'NONE', #31582, 2.000000000000000444 ) ;
#35213 = CARTESIAN_POINT ( 'NONE',  ( 116.5969481442453031, 0.5811942927096154232, -14.16772938898807155 ) ) ;
#35214 = CARTESIAN_POINT ( 'NONE',  ( 136.1682244357625109, 0.5463004873506387415, -15.67897323516908159 ) ) ;
#35215 = CARTESIAN_POINT ( 'NONE',  ( 109.9963952545248134, 0.8980012041604421569, -11.00651665394454071 ) ) ;
#35216 = DIRECTION ( 'NONE',  ( -0.000000000000000000, -0.9284778069183721172, -0.3713878862591650232 ) ) ;
#35217 = FACE_OUTER_BOUND ( 'NONE', #10483, .T. ) ;
#35218 = FACE_BOUND ( 'NONE', #43601, .T. ) ;
#35219 = CARTESIAN_POINT ( 'NONE',  ( 116.1431348109119881, -10.30919188438810075, -12.61870101168855918 ) ) ;
#35220 = CARTESIAN_POINT ( 'NONE',  ( 136.0320772899216877, -10.73234492129708428, -14.10229740280723476 ) ) ;
#35221 = CARTESIAN_POINT ( 'NONE',  ( 70.19189222814998175, -100.0979043305785581, -53.24182196210380624 ) ) ;
#35222 = CARTESIAN_POINT ( 'NONE',  ( 111.6379010812576809, -0.01829820670803256055, -12.14321520033831625 ) ) ;
#35223 = CARTESIAN_POINT ( 'NONE',  ( 117.5613014775786525, -10.15424416112534267, -14.75197769757730804 ) ) ;
#35224 = CARTESIAN_POINT ( 'NONE',  ( 116.0388171295248014, 0.1403307496149613920, -13.39321520033831447 ) ) ;
#35225 = CARTESIAN_POINT ( 'NONE',  ( 113.4769814775786330, 0.4262465694468514643, -12.03445270309931736 ) ) ;
#35226 = CARTESIAN_POINT ( 'NONE',  ( 111.9261565460472099, -2.191907684172563986, -18.20049396185734025 ) ) ;
#35228 = CARTESIAN_POINT ( 'NONE',  ( 117.7882081442453170, -6.344957434206665248, -7.627207830600338134 ) ) ;
#35227 = CARTESIAN_POINT ( 'NONE',  ( 118.5823814775786502, -1.834011780172310591, -8.268836392978581529 ) ) ;
#35229 = CARTESIAN_POINT ( 'NONE',  ( 124.3685014775786328, 0.4262465694468514643, -12.03445270309931736 ) ) ;
#35230 = CARTESIAN_POINT ( 'NONE',  ( 120.3976348109119812, -7.643976991954077427, -18.09477374809248928 ) ) ;
#35231 = VERTEX_POINT ( 'NONE', #37312 ) ;
#35232 = CARTESIAN_POINT ( 'NONE',  ( 136.2315975805923074, -7.075343981943422733, -7.974264555883486594 ) ) ;
#35233 = CARTESIAN_POINT ( 'NONE',  ( 121.8158014775786171, -5.638512984488999180, -18.83840828888717311 ) ) ;
#35234 = CARTESIAN_POINT ( 'NONE',  ( 113.8163171295247764, 0.1403307496149613920, -13.39321520033831447 ) ) ;
#35235 = CARTESIAN_POINT ( 'NONE',  ( 120.5678148109119832, -1.833838273342659253, -17.42832698103878286 ) ) ;
#35236 = CARTESIAN_POINT ( 'NONE',  ( 114.0442481442453300, -7.643976991954077427, -18.09477374809248928 ) ) ;
#35237 = CARTESIAN_POINT ( 'NONE',  ( 86.02111790076683917, -27.18318332158748518, -8.573249023392461865 ) ) ;
#35238 = CARTESIAN_POINT ( 'NONE',  ( 112.9828796295247884, -4.863998795839590272, -19.15521520033831493 ) ) ;
#35239 = CARTESIAN_POINT ( 'NONE',  ( 119.3198281442452924, -9.859900752359374465, -12.68260735090039404 ) ) ;
#35240 = CARTESIAN_POINT ( 'NONE',  ( 121.8158014775786171, -4.153390946401325223, -8.397313243818185668 ) ) ;
#35241 = DIRECTION ( 'NONE',  ( 0.000000000000000000, 0.6004852223388321697, -0.7996358532186279566 ) ) ;
#35242 = FACE_OUTER_BOUND ( 'NONE', #27508, .T. ) ;
#35243 = CARTESIAN_POINT ( 'NONE',  ( 121.8965016859119856, -9.665098340737509730, -17.37397104707595474 ) ) ;
#35244 = CARTESIAN_POINT ( 'NONE',  ( 111.1770983795247787, -8.402594152722688392, -16.93181055722141792 ) ) ;
#35245 = CARTESIAN_POINT ( 'NONE',  ( 117.1385944202825442, 1.513614675977436264, -21.43912135226106486 ) ) ;
#35246 = CARTESIAN_POINT ( 'NONE',  ( 119.0361948109119652, -7.893985811506177619, -18.51759400769804742 ) ) ;
#35247 = CARTESIAN_POINT ( 'NONE',  ( 113.7038881442453402, -3.383040157471821630, -19.15922257007629170 ) ) ;
#35248 = CARTESIAN_POINT ( 'NONE',  ( 112.8439733795247832, -8.938348069036489818, -17.46756447353520159 ) ) ;
#35249 = CARTESIAN_POINT ( 'NONE',  ( 114.5547881442453217, -5.638512984488999180, -18.83840828888717311 ) ) ;
#35250 = ORIENTED_EDGE ( 'NONE', *, *, #32097, .T. ) ;
#35251 = DIRECTION ( 'NONE',  ( 0.000000000000000000, -0.9242245927363029745, -0.3818493186865927758 ) ) ;
#35252 = AXIS2_PLACEMENT_3D ( 'NONE', #26796, #9465, #19721 ) ;
#35253 = CARTESIAN_POINT ( 'NONE',  ( 121.2485348109119769, -0.4660016031367893996, -10.09054647747474043 ) ) ;
#35254 = CARTESIAN_POINT ( 'NONE',  ( 116.5402214775786405, 0.2603800115204892296, -16.42320221600525088 ) ) ;
#35255 = CARTESIAN_POINT ( 'NONE',  ( 122.0427081442452817, -9.859900752359378018, -12.68260735090039759 ) ) ;
#35256 = CARTESIAN_POINT ( 'NONE',  ( 111.8319081442453182, -4.153390946401321671, -8.397313243818183892 ) ) ;
#35257 = CARTESIAN_POINT ( 'NONE',  ( 123.3474214775786209, -9.988377603198976828, -10.36322818467138340 ) ) ;
#35258 = VECTOR ( 'NONE', #21619, 1000.000000000000000 ) ;
#35259 = CARTESIAN_POINT ( 'NONE',  ( 115.0664733795247798, -8.938348069036489818, -17.46756447353520159 ) ) ;
#35260 = CARTESIAN_POINT ( 'NONE',  ( 117.4478481442453131, -9.565557343593413364, -10.61323700422348004 ) ) ;
#35261 = CARTESIAN_POINT ( 'NONE',  ( 123.6800462736033239, -5.999693504163852609, -18.26366844790029731 ) ) ;
#35262 = ORIENTED_EDGE ( 'NONE', *, *, #4120, .F. ) ;
#35263 = CARTESIAN_POINT ( 'NONE',  ( 120.9649014775786355, -3.383040157471821630, -19.15922257007629170 ) ) ;
#35264 = ADVANCED_FACE ( 'NONE', ( #5850 ), #26161, .T. ) ;
#35265 = CARTESIAN_POINT ( 'NONE',  ( 124.0495485609119584, -10.36940331770106916, -15.09355782777062061 ) ) ;
#35266 = CARTESIAN_POINT ( 'NONE',  ( 120.8514481442452961, -7.893985811506177619, -18.51759400769804742 ) ) ;
#35267 = ORIENTED_EDGE ( 'NONE', *, *, #4967, .T. ) ;
#35268 = CARTESIAN_POINT ( 'NONE',  ( 115.8999108795247821, -8.938348069036489818, -9.318865927141430916 ) ) ;
#35269 = CARTESIAN_POINT ( 'NONE',  ( 124.7088614775786226, 0.2603800115204892296, -16.42320221600525088 ) ) ;
#35270 = CARTESIAN_POINT ( 'NONE',  ( 119.9481648144346622, -2.280480477428469488, -18.08254604495227014 ) ) ;
#35271 = CARTESIAN_POINT ( 'NONE',  ( 117.0507614775786465, 0.1319031606808879209, -14.10382304977623669 ) ) ;
#35272 =( BOUNDED_CURVE ( )  B_SPLINE_CURVE ( 3, ( #3340, #17259, #6987, #31148 ),
 .UNSPECIFIED., .F., .T. ) 
 B_SPLINE_CURVE_WITH_KNOTS ( ( 4, 4 ),
 ( 1.570796326794904996, 3.141592653589790007 ),
 .UNSPECIFIED. ) 
 CURVE ( )  GEOMETRIC_REPRESENTATION_ITEM ( )  RATIONAL_B_SPLINE_CURVE ( ( 1.000000000000000000, 0.8047378541243679351, 0.8047378541243679351, 1.000000000000000000 ) ) 
 REPRESENTATION_ITEM ( '' )  );
#35273 = CARTESIAN_POINT ( 'NONE',  ( 67.84197459855160162, -55.51165166589005651, -36.13664933202900897 ) ) ;
#35274 = CARTESIAN_POINT ( 'NONE',  ( 120.8514481442452961, -2.084020599724406786, -8.691656652584148546 ) ) ;
#35275 = CARTESIAN_POINT ( 'NONE',  ( 121.7590748109119687, -7.893985811506158079, -18.51759400769805453 ) ) ;
#35276 = CARTESIAN_POINT ( 'NONE',  ( 121.5321681442453183, -0.1624402480850797581, -16.17319339645315424 ) ) ;
#35277 = VECTOR ( 'NONE', #23482, 1000.000000000000227 ) ;
#35278 = CARTESIAN_POINT ( 'NONE',  ( 70.19189222814998175, -56.33107134722149567, -35.73524133214168330 ) ) ;
#35279 = CARTESIAN_POINT ( 'NONE',  ( 117.6747548109119919, -7.643976991954077427, -18.09477374809248928 ) ) ;
#35280 = CARTESIAN_POINT ( 'NONE',  ( 122.7993923109119692, -9.959231468620755479, -10.70263013195267199 ) ) ;
#35281 = CARTESIAN_POINT ( 'NONE',  ( 115.0086014775786509, -4.089484607189486809, -7.948022111789456723 ) ) ;
#35282 = CARTESIAN_POINT ( 'NONE',  ( 125.3895814775786448, -2.084020599724406786, -8.691656652584148546 ) ) ;
#35283 = CARTESIAN_POINT ( 'NONE',  ( 109.2294421295247844, 0.8460904216231607267, -19.39321520033831447 ) ) ;
#35284 = VECTOR ( 'NONE', #17209, 1000.000000000000000 ) ;
#35285 = CARTESIAN_POINT ( 'NONE',  ( 119.2063748109119814, -7.894159318335828068, -9.358103419637847864 ) ) ;
#35286 = ORIENTED_EDGE ( 'NONE', *, *, #13645, .T. ) ;
#35287 = CARTESIAN_POINT ( 'NONE',  ( 116.6536748109119941, 0.9020085738987339008, -11.91225656197089222 ) ) ;
#35288 = CARTESIAN_POINT ( 'NONE',  ( 114.7192077545248594, -2.791137627527939813, -18.39754474579286025 ) ) ;
#35289 = EDGE_CURVE ( 'NONE', #33790, #5920, #3444, .T. ) ;
#35290 = CARTESIAN_POINT ( 'NONE',  ( 121.9470836909669913, -24.14644159042263993, -12.62951656296512937 ) ) ;
#35291 = CARTESIAN_POINT ( 'NONE',  ( 70.19189222814998175, -52.61716011954800365, -34.24968978710501943 ) ) ;
#35292 = CARTESIAN_POINT ( 'NONE',  ( 121.7575954359119521, 0.5291689781388270175, -13.89700978578772705 ) ) ;
#35293 = CARTESIAN_POINT ( 'NONE',  ( 121.0216281442452981, -1.561330072975668948, -17.79121239304076951 ) ) ;
#35294 = VERTEX_POINT ( 'NONE', #6079 ) ;
#35295 = CARTESIAN_POINT ( 'NONE',  ( 127.4620922276975818, -9.182459662741596418, -9.793643861152926178 ) ) ;
#35296 = CARTESIAN_POINT ( 'NONE',  ( 122.0427081442452817, -9.859900752359378018, -12.68260735090039759 ) ) ;
#35297 = EDGE_CURVE ( 'NONE', #17020, #27501, #13648, .T. ) ;
#35298 = CARTESIAN_POINT ( 'NONE',  ( 120.8547048109119686, -7.554583864224885481, -18.48844787311982785 ) ) ;
#35299 = CARTESIAN_POINT ( 'NONE',  ( 125.4584548109119737, -7.476587315910852460, -21.06050163197695824 ) ) ;
#35300 = CARTESIAN_POINT ( 'NONE',  ( 125.6732148109119862, 0.5811942927096110934, -14.16772938898807510 ) ) ;
#35301 = EDGE_CURVE ( 'NONE', #10099, #21089, #25286, .T. ) ;
#35302 = CARTESIAN_POINT ( 'NONE',  ( 111.0381921295247878, -9.868328341294093420, -13.39321520033831447 ) ) ;
#35303 = ORIENTED_EDGE ( 'NONE', *, *, #22638, .F. ) ;
#35304 = CARTESIAN_POINT ( 'NONE',  ( 114.3846081442453197, -10.63000616557722466, -14.87417383870573495 ) ) ;
#35305 = CARTESIAN_POINT ( 'NONE',  ( 126.0135748109119902, -1.833838273342660141, -17.42832698103878286 ) ) ;
#35306 = CARTESIAN_POINT ( 'NONE',  ( 124.5386814775786206, -5.638512984488999180, -18.83840828888717311 ) ) ;
#35307 = CARTESIAN_POINT ( 'NONE',  ( 120.3976348109119812, -7.643976991954077427, -18.09477374809248928 ) ) ;
#35308 = CARTESIAN_POINT ( 'NONE',  ( 126.3509913982043571, -3.720841214467113911, -8.457387538663136084 ) ) ;
#35309 = DIRECTION ( 'NONE',  ( 0.9970811988817437355, -0.07634843047859309062, -9.125038414728249219E-18 ) ) ;
#35310 = CARTESIAN_POINT ( 'NONE',  ( 122.2696148109119889, -4.089484607189486809, -7.948022111789456723 ) ) ;
#35311 = CARTESIAN_POINT ( 'NONE',  ( 112.0126281442453120, -9.814174330883659536, -12.68911139247490105 ) ) ;
#35312 = CARTESIAN_POINT ( 'NONE',  ( 63.10250807381770244, -31.76310523276724140, -22.30742876271141029 ) ) ;
#35313 = CARTESIAN_POINT ( 'NONE',  ( 91.11246428952674137, -26.75858941326842810, -11.54476601486570964 ) ) ;
#35314 = CARTESIAN_POINT ( 'NONE',  ( 112.0588148109119828, 0.5811942927096154232, -14.16772938898807155 ) ) ;
#35315 = ORIENTED_EDGE ( 'NONE', *, *, #41490, .F. ) ;
#35316 = CIRCLE ( 'NONE', #22967, 3.499999999999998668 ) ;
#35317 = CARTESIAN_POINT ( 'NONE',  ( 116.1777233795247781, -1.325403438956436419, -9.854619843455211026 ) ) ;
#35318 = CARTESIAN_POINT ( 'NONE',  ( 120.4543614775786295, -4.089484607189486809, -7.948022111789456723 ) ) ;
#35319 = CARTESIAN_POINT ( 'NONE',  ( 135.3184548109119874, -10.44474571748257041, -15.59668151425567650 ) ) ;
#35320 = ORIENTED_EDGE ( 'NONE', *, *, #22839, .T. ) ;
#35321 = EDGE_CURVE ( 'NONE', #38363, #8497, #43703, .T. ) ;
#35322 = DIRECTION ( 'NONE',  ( -1.734723475976807094E-15, -1.000000000000000000, 0.000000000000000000 ) ) ;
#35323 = ADVANCED_FACE ( 'NONE', ( #30032 ), #10555, .T. ) ;
#35324 = ADVANCED_FACE ( 'NONE', ( #27299 ), #41875, .T. ) ;
#35325 = CARTESIAN_POINT ( 'NONE',  ( 123.3474214775786209, -9.988377603198976828, -10.36322818467138340 ) ) ;
#35326 = VECTOR ( 'NONE', #34705, 1000.000000000000114 ) ;
#35327 = CARTESIAN_POINT ( 'NONE',  ( 108.5378796295247810, -4.863998795839590272, -19.15521520033831493 ) ) ;
#35328 = CARTESIAN_POINT ( 'NONE',  ( 122.2696148109119889, -5.574606645277164318, -18.38911715685844683 ) ) ;
#35329 = ORIENTED_EDGE ( 'NONE', *, *, #23091, .T. ) ;
#35330 = CARTESIAN_POINT ( 'NONE',  ( 114.6115148109119986, -3.383040157471821630, -19.15922257007629170 ) ) ;
#35331 = DIRECTION ( 'NONE',  ( 1.000000000000000000, 0.000000000000000000, 0.000000000000000000 ) ) ;
#35332 = DIRECTION ( 'NONE',  ( 1.000000000000000000, 0.000000000000000000, -0.000000000000000000 ) ) ;
#35333 = DIRECTION ( 'NONE',  ( -0.0009519285464165692153, 0.9999995469159186356, 0.000000000000000000 ) ) ;
#35334 = CARTESIAN_POINT ( 'NONE',  ( 124.3117748109119844, -10.30919188438810075, -12.61870101168855918 ) ) ;
#35335 = DIRECTION ( 'NONE',  ( 0.000000000000000000, 0.000000000000000000, 1.000000000000000000 ) ) ;
#35336 = PLANE ( 'NONE',  #440 ) ;
#35337 = CARTESIAN_POINT ( 'NONE',  ( 122.2128881442453263, -1.834011780172310813, -8.268836392978581529 ) ) ;
#35339 = CARTESIAN_POINT ( 'NONE',  ( 122.4965214775786251, 0.1319031606808879209, -14.10382304977623669 ) ) ;
#35338 = CARTESIAN_POINT ( 'NONE',  ( 121.5888948109119809, -10.30919188438810075, -12.61870101168855918 ) ) ;
#35340 = CARTESIAN_POINT ( 'NONE',  ( 118.6958348109119754, -3.505236298600246325, -18.68346056562440793 ) ) ;
#35341 = DIRECTION ( 'NONE',  ( -1.000000000000000000, 0.000000000000000000, -0.000000000000000000 ) ) ;
#35342 = CARTESIAN_POINT ( 'NONE',  ( 118.5256548109119876, -0.4660016031367893996, -10.09054647747474043 ) ) ;
#35343 = ORIENTED_EDGE ( 'NONE', *, *, #41310, .T. ) ;
#35344 = CARTESIAN_POINT ( 'NONE',  ( 112.2883483795247770, -0.7896495226426338832, -9.318865927141420258 ) ) ;
#35345 = CARTESIAN_POINT ( 'NONE',  ( 69.36136150295220659, -62.04407695266556289, -34.91561601123756731 ) ) ;
#35346 = AXIS2_PLACEMENT_3D ( 'NONE', #28528, #4108, #42210 ) ;
#35347 = CARTESIAN_POINT ( 'NONE',  ( 114.0246765045248196, -2.791137627527939813, -8.388885654883777576 ) ) ;
#35348 = CARTESIAN_POINT ( 'NONE',  ( 108.8156921295247912, -9.868328341294093420, -13.39321520033831447 ) ) ;
#35349 = CARTESIAN_POINT ( 'NONE',  ( 113.3301452545248083, -9.868328341294098749, -15.46607636864997204 ) ) ;
#35350 = CARTESIAN_POINT ( 'NONE',  ( 126.2404814775786264, -9.261995988541697145, -16.69588392320189030 ) ) ;
#35351 = CARTESIAN_POINT ( 'NONE',  ( 112.9097148109120070, 0.2603800115204892296, -16.42320221600525088 ) ) ;
#35352 = ORIENTED_EDGE ( 'NONE', *, *, #12095, .F. ) ;
#35353 = CARTESIAN_POINT ( 'NONE',  ( 112.9097148109120070, -9.565557343593413364, -10.61323700422348004 ) ) ;
#35354 = CARTESIAN_POINT ( 'NONE',  ( 113.7468640045248236, -10.62599879583958717, -11.00651665394454604 ) ) ;
#35355 = CARTESIAN_POINT ( 'NONE',  ( 119.1496481442453046, -6.222761293078222344, -8.102969835052219238 ) ) ;
#35356 = CARTESIAN_POINT ( 'NONE',  ( 111.2646872982215029, -8.898115269823104967, -16.42473896082089269 ) ) ;
#35357 = CARTESIAN_POINT ( 'NONE',  ( 123.3474214775786209, -9.988377603198976828, -10.36322818467138340 ) ) ;
#35359 = AXIS2_PLACEMENT_3D ( 'NONE', #21054, #25159, #28133 ) ;
#35358 = DIRECTION ( 'NONE',  ( 0.000000000000000000, -0.9242245927363028635, -0.3818493186865930533 ) ) ;
#35360 = CARTESIAN_POINT ( 'NONE',  ( 117.7882081442453170, -6.344957434206665248, -7.627207830600338134 ) ) ;
#35361 = EDGE_CURVE ( 'NONE', #30793, #38132, #10418, .T. ) ;
#35362 = CARTESIAN_POINT ( 'NONE',  ( 113.9552233795247815, -8.938348069036489818, -17.46756447353520159 ) ) ;
#35363 = CARTESIAN_POINT ( 'NONE',  ( 112.4967077545247633, -2.791137627527939813, -18.39754474579286025 ) ) ;
#35364 = ORIENTED_EDGE ( 'NONE', *, *, #2472, .T. ) ;
#35365 = DIRECTION ( 'NONE',  ( 0.6049664196031343533, -0.7962509850245488296, 0.000000000000000000 ) ) ;
#35366 = CARTESIAN_POINT ( 'NONE',  ( 116.1431348109119881, 0.1319031606808879209, -14.10382304977623669 ) ) ;
#35367 = CARTESIAN_POINT ( 'NONE',  ( 126.3539348109119800, -4.153390946401325223, -8.397313243818185668 ) ) ;
#35368 = CARTESIAN_POINT ( 'NONE',  ( 112.9664414775786412, 0.5811942927096154232, -14.16772938898807155 ) ) ;
#35369 = CARTESIAN_POINT ( 'NONE',  ( 124.1983214775786166, -1.833838273342659697, -17.42832698103878286 ) ) ;
#35370 = CARTESIAN_POINT ( 'NONE',  ( 119.4332814775786318, -8.899110576539710493, -16.42337572283490132 ) ) ;
#35371 = CARTESIAN_POINT ( 'NONE',  ( 114.7816948109119863, -9.859900752359374465, -12.68260735090039404 ) ) ;
#35372 = ORIENTED_EDGE ( 'NONE', *, *, #35560, .F. ) ;
#35373 = CARTESIAN_POINT ( 'NONE',  ( 125.6164881442453094, -9.565557343593413364, -10.61323700422348004 ) ) ;
#35374 = AXIS2_PLACEMENT_3D ( 'NONE', #22427, #16274, #5992 ) ;
#35375 = CARTESIAN_POINT ( 'NONE',  ( 95.62170725701133733, -25.05980814603879026, -13.56410367930211969 ) ) ;
#35376 = CARTESIAN_POINT ( 'NONE',  ( 114.0442481442453300, -7.643976991954077427, -18.09477374809248928 ) ) ;
#35377 = ORIENTED_EDGE ( 'NONE', *, *, #20311, .T. ) ;
#35378 = DIRECTION ( 'NONE',  ( 0.000000000000000000, 0.4669533266896293000, 0.8842819633428516957 ) ) ;
#35379 = EDGE_CURVE ( 'NONE', #16139, #24584, #20680, .T. ) ;
#35380 = CARTESIAN_POINT ( 'NONE',  ( 105.4819421295248247, 0.8980012041604618078, -13.39321520033831447 ) ) ;
#35381 = CARTESIAN_POINT ( 'NONE',  ( 111.4549108795247747, -1.325403438956436419, -16.93181055722141792 ) ) ;
#35382 = CARTESIAN_POINT ( 'NONE',  ( 123.4608748109119745, 0.4262465694468514643, -12.03445270309931736 ) ) ;
#35383 = AXIS2_PLACEMENT_3D ( 'NONE', #38941, #21174, #28026 ) ;
#35384 = VERTEX_POINT ( 'NONE', #34340 ) ;
#35385 = EDGE_CURVE ( 'NONE', #36318, #7179, #8327, .T. ) ;
#35386 = CARTESIAN_POINT ( 'NONE',  ( 118.0718414775786442, -0.8288870151387760510, -10.36305467784173118 ) ) ;
#35387 = CARTESIAN_POINT ( 'NONE',  ( 118.2987481442453088, -7.894159318335828068, -9.358103419637847864 ) ) ;
#35388 = EDGE_CURVE ( 'NONE', #2916, #30417, #23020, .T. ) ;
#35389 = CARTESIAN_POINT ( 'NONE',  ( 70.19189222814998175, -52.97765562947117957, -34.39388673445118627 ) ) ;
#35390 = AXIS2_PLACEMENT_3D ( 'NONE', #11400, #42188, #17786 ) ;
#35391 = CARTESIAN_POINT ( 'NONE',  ( 123.7022829359119811, -4.283928203966213211, -7.183505701512925334 ) ) ;
#35392 = ORIENTED_EDGE ( 'NONE', *, *, #32414, .F. ) ;
#35393 = CARTESIAN_POINT ( 'NONE',  ( 121.1141531944929284, -1.036737761566197014, -17.24079555149560861 ) ) ;
#35394 = CARTESIAN_POINT ( 'NONE',  ( 125.1028739313145905, -0.5192815678331393903, -7.317066403780624562 ) ) ;
#35395 = CARTESIAN_POINT ( 'NONE',  ( 110.0658483795247804, -0.7896495226426338832, -9.318865927141430916 ) ) ;
#35396 = CARTESIAN_POINT ( 'NONE',  ( 113.0231681442453322, 0.9020085738987339008, -11.91225656197089222 ) ) ;
#35397 = CARTESIAN_POINT ( 'NONE',  ( 113.3068014775786594, -8.166667518702817929, -8.995218007635859436 ) ) ;
#35398 = CARTESIAN_POINT ( 'NONE',  ( 116.7671281442453335, -7.643976991954077427, -18.09477374809248928 ) ) ;
#35399 = CARTESIAN_POINT ( 'NONE',  ( 128.2184548109119930, -10.44474571748257041, -15.59668151425567650 ) ) ;
#35400 = ORIENTED_EDGE ( 'NONE', *, *, #3827, .F. ) ;
#35401 = CARTESIAN_POINT ( 'NONE',  ( 114.4413348109119823, -0.8288870151387760510, -10.36305467784173118 ) ) ;
#35402 = CARTESIAN_POINT ( 'NONE',  ( 116.1082702545247827, -10.62599879583958717, -15.77991374673208469 ) ) ;
#35403 = CARTESIAN_POINT ( 'NONE',  ( 66.04840902401572578, -36.51491089899629827, -5.214988841577086198 ) ) ;
#35404 = CARTESIAN_POINT ( 'NONE',  ( 116.5944421295247793, 0.8980012041604618078, -13.39321520033831447 ) ) ;
#35405 = AXIS2_PLACEMENT_3D ( 'NONE', #34708, #41815, #31967 ) ;
#35406 = CARTESIAN_POINT ( 'NONE',  ( 115.0086014775786509, -4.089484607189486809, -7.948022111789456723 ) ) ;
#35407 = ORIENTED_EDGE ( 'NONE', *, *, #39042, .T. ) ;
#35408 = CARTESIAN_POINT ( 'NONE',  ( 116.7104014775786425, -0.4660016031367893996, -10.09054647747474043 ) ) ;
#35409 = CARTESIAN_POINT ( 'NONE',  ( 61.69189222814998175, -40.21211973637273474, -4.893215200338314474 ) ) ;
#35410 = CARTESIAN_POINT ( 'NONE',  ( 111.8021765045248372, -7.250697342233347165, -19.15521520033831138 ) ) ;
#35411 = CARTESIAN_POINT ( 'NONE',  ( 114.3278814775786429, -10.30919188438810075, -12.61870101168855918 ) ) ;
#35412 = CARTESIAN_POINT ( 'NONE',  ( 113.5904348109119866, -7.893985811506177619, -18.51759400769804742 ) ) ;
#35413 = CARTESIAN_POINT ( 'NONE',  ( 61.00489063115648491, -4.079117376897293923, -19.39321520033831092 ) ) ;
#35414 = DIRECTION ( 'NONE',  ( 0.000000000000000000, -0.9242245927363028635, -0.3818493186865930533 ) ) ;
#35415 = CARTESIAN_POINT ( 'NONE',  ( 109.0935046295247872, -4.863998795839590272, -18.39754474579285315 ) ) ;
#35416 = AXIS2_PLACEMENT_3D ( 'NONE', #36373, #25906, #12683 ) ;
#35417 = ORIENTED_EDGE ( 'NONE', *, *, #37729, .F. ) ;
#35418 = DIRECTION ( 'NONE',  ( 0.9609149988134837450, -0.1028163501681639419, 0.2570431154366518145 ) ) ;
#35419 = CARTESIAN_POINT ( 'NONE',  ( 109.2294282733528519, -3.755413602395687445, -18.41110207307550084 ) ) ;
#35420 = CARTESIAN_POINT ( 'NONE',  ( 116.9373081442452929, -1.833838273342659253, -17.42832698103878286 ) ) ;
#35421 = CARTESIAN_POINT ( 'NONE',  ( 65.05177286768275735, -13.36142499895917446, -11.78221109098726771 ) ) ;
#35422 = CARTESIAN_POINT ( 'NONE',  ( 116.2471765045247594, -2.791137627527939813, -8.388885654883777576 ) ) ;
#35423 = CARTESIAN_POINT ( 'NONE',  ( 108.1211608795247798, -8.938348069036489818, -9.318865927141430916 ) ) ;
#35424 = CARTESIAN_POINT ( 'NONE',  ( 127.3669547543521929, -5.331670183757885262, -7.838481523644200699 ) ) ;
#35425 = CARTESIAN_POINT ( 'NONE',  ( 116.0864081442453113, -0.1624402480850797581, -16.17319339645315424 ) ) ;
#35426 = CARTESIAN_POINT ( 'NONE',  ( 135.4185995790644483, 1.087834318095270758, -12.63462434935058276 ) ) ;
#35427 = CARTESIAN_POINT ( 'NONE',  ( 122.4397948109119767, -9.988377603198976828, -10.36322818467138340 ) ) ;
#35428 = CARTESIAN_POINT ( 'NONE',  ( 117.6180281442453150, -0.4660016031367893996, -10.09054647747474043 ) ) ;
#35430 = VERTEX_POINT ( 'NONE', #30262 ) ;
#35429 = ADVANCED_FACE ( 'NONE', ( #38429 ), #2942, .T. ) ;
#35431 = AXIS2_PLACEMENT_3D ( 'NONE', #13220, #27119, #20282 ) ;
#35432 = CARTESIAN_POINT ( 'NONE',  ( 114.1577014775786552, -3.505236298600246325, -18.68346056562440793 ) ) ;
#35433 = CARTESIAN_POINT ( 'NONE',  ( 112.3991748109119868, -8.166667518702817929, -8.995218007635859436 ) ) ;
#35434 = CARTESIAN_POINT ( 'NONE',  ( 117.2776681442452968, -5.638512984488999180, -18.83840828888717311 ) ) ;
#35435 = CARTESIAN_POINT ( 'NONE',  ( 115.1220548109119761, -1.833838273342658809, -17.42832698103878286 ) ) ;
#35436 = ORIENTED_EDGE ( 'NONE', *, *, #23419, .F. ) ;
#35437 = CARTESIAN_POINT ( 'NONE',  ( 122.1561614775786353, -8.899110576539710493, -16.42337572283490132 ) ) ;
#35438 = CARTESIAN_POINT ( 'NONE',  ( 117.4478481442453131, 0.2603800115204892296, -16.42320221600525088 ) ) ;
#35439 = CARTESIAN_POINT ( 'NONE',  ( 136.6755514030890026, 0.3990558587189101947, -15.48381416683688094 ) ) ;
#35440 = AXIS2_PLACEMENT_3D ( 'NONE', #22721, #4940, #11799 ) ;
#35441 = CARTESIAN_POINT ( 'NONE',  ( 110.9687390045248350, 0.8980012041604421569, -15.77991374673208469 ) ) ;
#35442 = CARTESIAN_POINT ( 'NONE',  ( 90.04708369096697140, -25.51891511063604767, -13.19656280121471958 ) ) ;
#35443 = CARTESIAN_POINT ( 'NONE',  ( 116.5944421295247793, -9.863109299026486809, -13.29890625629612622 ) ) ;
#35444 = VECTOR ( 'NONE', #9510, 1000.000000000000000 ) ;
#35445 = CARTESIAN_POINT ( 'NONE',  ( 113.3995983795247895, -8.402594152722688392, -16.93181055722141792 ) ) ;
#35446 = CARTESIAN_POINT ( 'NONE',  ( 115.8595014775786609, -1.834011780172310813, -8.268836392978581529 ) ) ;
#35447 = CARTESIAN_POINT ( 'NONE',  ( 135.7778351054948587, -10.78233002638890348, -14.13261394578744579 ) ) ;
#35448 = CARTESIAN_POINT ( 'NONE',  ( 114.0442481442453300, -7.643976991954077427, -18.09477374809248928 ) ) ;
#35449 = DIRECTION ( 'NONE',  ( 0.000000000000000000, 0.000000000000000000, 1.000000000000000000 ) ) ;
#35450 = CARTESIAN_POINT ( 'NONE',  ( 117.1642148109119859, -0.8288870151387769392, -10.36305467784172940 ) ) ;
#35451 = CARTESIAN_POINT ( 'NONE',  ( 113.8857702545248003, 0.1403307496149616695, -11.32035403202665336 ) ) ;
#35452 = VECTOR ( 'NONE', #15227, 1000.000000000000114 ) ;
#35453 = CARTESIAN_POINT ( 'NONE',  ( 114.9716510812576757, -0.01829820670803256055, -12.14321520033831625 ) ) ;
#35454 = SURFACE_SIDE_STYLE ('',( #25217 ) ) ;
#35455 = FACE_BOUND ( 'NONE', #4841, .T. ) ;
#35457 = CARTESIAN_POINT ( 'NONE',  ( 118.5256548109119876, -0.4660016031367893996, -10.09054647747474043 ) ) ;
#35456 = CARTESIAN_POINT ( 'NONE',  ( 65.48165112743714644, -14.20078584921842868, -9.574444890468706504 ) ) ;
#35458 = CARTESIAN_POINT ( 'NONE',  ( 118.2987481442453088, -7.894159318335828068, -9.358103419637847864 ) ) ;
#35459 = CARTESIAN_POINT ( 'NONE',  ( 112.4559014775786778, -0.1624402480850797581, -16.17319339645315424 ) ) ;
#35460 = VERTEX_POINT ( 'NONE', #26620 ) ;
#35461 = FACE_OUTER_BOUND ( 'NONE', #2996, .T. ) ;
#35462 = CARTESIAN_POINT ( 'NONE',  ( 122.6099748109119929, -9.261995988541697145, -16.69588392320189030 ) ) ;
#35463 = CARTESIAN_POINT ( 'NONE',  ( 112.5661608795247872, -1.325403438956436419, -16.93181055722141792 ) ) ;
#35464 = CARTESIAN_POINT ( 'NONE',  ( 118.3554748109119998, -9.565557343593413364, -10.61323700422348004 ) ) ;
#35465 =( BOUNDED_SURFACE ( )  B_SPLINE_SURFACE ( 1, 2, ( 
 ( #18692, #22332, #32134, #42862, #29397, #25982, #29168, #11622, #4993, #25533, #42638, #39439, #903, #21435, #35317, #28734, #32794, #11407, #32360, #38979, #28511, #4089, #18471, #11182, #8427, #18011, #35775, #8200, #42416, #22109, #35999, #675, #1568, #32580, #15490, #1350, #43082, #43307, #25757, #39663, #36227, #31910, #7747, #21658, #12529, #16173, #8873, #20046, #33465, #5217, #30522, #19583, #36449, #44223, #19135, #33701, #40797, #2243, #9101, #23002, #22771, #26431, #33018, #30078, #12304, #33248, #36670, #40109, #5441, #2473, #37118, #26203, #12984, #16398, #23469, #2021, #30296, #36895, #1792, #19361, #40337, #15946, #22549, #43992, #44444, #13211, #43763, #9552, #26879, #5664, #29847, #12753, #26654, #37355, #29620, #6127, #40568, #5891, #15718, #9328, #23235, #33929, #19813, #2699, #43535, #16627, #39886, #8649, #24142, #31407, #20719, #35028, #23700, #27110, #6811, #34158, #3811, #24361, #38247, #34811, #10457, #17302, #21154, #14090, #17509, #13656, #31632, #3596, #3160, #174, #7027, #28008, #24581, #34598, #10679, #41915, #38034, #17082, #38465, #7239, #13436, #20498, #3383, #31193, #45113, #23926, #17734, #37589, #6361, #13871, #400, #41033, #9788, #27781, #20272, #41694, #30974, #20939, #10018, #2929, #16858 ),
 ( #30750, #44673, #34379, #27339, #41260, #27563, #37807, #6582, #44898, #41478, #10235, #32309, #24800, #18636, #39153, #8150, #38919, #38691, #22054, #14767, #18852, #21376, #35259, #14316, #32744, #4719, #21603, #43028, #35721, #28901, #28679, #7457, #42138, #32526, #25704, #845, #11344, #21827, #42583, #4035, #11572, #11123, #28232, #1075, #10900, #17957, #35947, #1299, #35490, #31857, #625, #22279, #28453, #7688, #42811, #15211, #14987, #14537, #25479, #25024, #11796, #42362, #39610, #29116, #4263, #18182, #32077, #7917, #39385, #25256, #4494, #8372, #18415, #36172, #4938, #43485, #30018, #33642, #15666, #12932, #12702, #16117, #29567, #1518, #40741, #40286, #6066, #15437, #12254, #33192, #19079, #5611, #5393, #2189, #9049, #22950, #23413, #5163, #26148, #43704, #19312, #37300, #36842, #12024, #22497, #37064, #25926, #15894, #43936, #16343, #40051, #19534, #8598, #8818, #12477, #23186, #26375, #5837, #33410, #9498, #43258, #29345, #26602, #36391, #19986, #40515, #9278, #19761, #2418, #30246, #39835, #44170, #26830, #1968, #32965, #1742, #22719, #36618, #29793, #7580, #31969, #28123, #18074, #24916, #296, #23874, #11015, #21495, #20220, #27288, #10792, #14209, #24689, #30699, #25148, #30469, #44389, #7355, #31526, #37529, #35380 ) ),
 .UNSPECIFIED., .F., .F., .T. ) 
 B_SPLINE_SURFACE_WITH_KNOTS ( ( 2, 2 ),
 ( 3, 2, 2, 2, 2, 2, 2, 2, 2, 2, 2, 2, 2, 2, 2, 2, 2, 2, 2, 2, 2, 2, 2, 2, 2, 2, 2, 2, 2, 2, 2, 2, 2, 2, 2, 2, 2, 2, 2, 2, 2, 2, 2, 2, 2, 2, 2, 2, 2, 2, 2, 2, 2, 2, 2, 2, 2, 2, 2, 2, 2, 2, 2, 2, 2, 2, 2, 2, 2, 2, 2, 2, 2, 2, 2, 2, 2, 2, 2, 2, 3 ),
 ( 0.000000000000000000, 1.000000000000000000 ),
 ( 0.000000000000000000, 0.01250000000000000069, 0.02500000000000000139, 0.03749999999999999861, 0.05000000000000000278, 0.06250000000000000000, 0.07499999999999999722, 0.08749999999999999445, 0.1000000000000000056, 0.1125000000000000028, 0.1250000000000000000, 0.1375000000000000111, 0.1499999999999999944, 0.1625000000000000056, 0.1749999999999999889, 0.1875000000000000000, 0.2000000000000000111, 0.2124999999999999944, 0.2250000000000000056, 0.2374999999999999889, 0.2500000000000000000, 0.2625000000000000111, 0.2750000000000000222, 0.2874999999999999778, 0.2999999999999999889, 0.3125000000000000000, 0.3250000000000000111, 0.3375000000000000222, 0.3499999999999999778, 0.3624999999999999889, 0.3750000000000000000, 0.3875000000000000111, 0.4000000000000000222, 0.4124999999999999778, 0.4249999999999999889, 0.4375000000000000000, 0.4500000000000000111, 0.4625000000000000222, 0.4749999999999999778, 0.4874999999999999889, 0.5000000000000000000, 0.5124999999999999556, 0.5250000000000000222, 0.5374999999999999778, 0.5500000000000000444, 0.5625000000000000000, 0.5749999999999999556, 0.5875000000000000222, 0.5999999999999999778, 0.6125000000000000444, 0.6250000000000000000, 0.6374999999999999556, 0.6500000000000000222, 0.6624999999999999778, 0.6750000000000000444, 0.6875000000000000000, 0.6999999999999999556, 0.7125000000000000222, 0.7249999999999999778, 0.7375000000000000444, 0.7500000000000000000, 0.7624999999999999556, 0.7750000000000000222, 0.7874999999999999778, 0.8000000000000000444, 0.8125000000000000000, 0.8249999999999999556, 0.8375000000000000222, 0.8499999999999999778, 0.8625000000000000444, 0.8750000000000000000, 0.8874999999999999556, 0.9000000000000000222, 0.9124999999999999778, 0.9250000000000000444, 0.9375000000000000000, 0.9499999999999999556, 0.9625000000000000222, 0.9749999999999999778, 0.9875000000000000444, 1.000000000000000000 ),
 .UNSPECIFIED. ) 
 GEOMETRIC_REPRESENTATION_ITEM ( )  RATIONAL_B_SPLINE_SURFACE ( (
 ( 1.000000000000000000, 0.9238795325112869605, 1.000000000000000000, 0.9238795325112869605, 1.000000000000000000, 0.9238795325112869605, 1.000000000000000000, 0.9238795325112869605, 1.000000000000000000, 0.9238795325112869605, 1.000000000000000000, 0.9238795325112869605, 1.000000000000000000, 0.9238795325112869605, 1.000000000000000000, 0.9238795325112869605, 1.000000000000000000, 0.9238795325112869605, 1.000000000000000000, 0.9238795325112869605, 1.000000000000000000, 0.9238795325112869605, 1.000000000000000000, 0.9238795325112869605, 1.000000000000000000, 0.9238795325112869605, 1.000000000000000000, 0.9238795325112869605, 1.000000000000000000, 0.9238795325112869605, 1.000000000000000000, 0.9238795325112869605, 1.000000000000000000, 0.9238795325112869605, 1.000000000000000000, 0.9238795325112869605, 1.000000000000000000, 0.9238795325112869605, 1.000000000000000000, 0.9238795325112869605, 1.000000000000000000, 0.9238795325112869605, 1.000000000000000000, 0.9238795325112869605, 1.000000000000000000, 0.9238795325112869605, 1.000000000000000000, 0.9238795325112869605, 1.000000000000000000, 0.9238795325112869605, 1.000000000000000000, 0.9238795325112869605, 1.000000000000000000, 0.9238795325112869605, 1.000000000000000000, 0.9238795325112869605, 1.000000000000000000, 0.9238795325112869605, 1.000000000000000000, 0.9238795325112869605, 1.000000000000000000, 0.9238795325112869605, 1.000000000000000000, 0.9238795325112869605, 1.000000000000000000, 0.9238795325112869605, 1.000000000000000000, 0.9238795325112869605, 1.000000000000000000, 0.9238795325112869605, 1.000000000000000000, 0.9238795325112869605, 1.000000000000000000, 0.9238795325112869605, 1.000000000000000000, 0.9238795325112869605, 1.000000000000000000, 0.9238795325112869605, 1.000000000000000000, 0.9238795325112869605, 1.000000000000000000, 0.9238795325112869605, 1.000000000000000000, 0.9238795325112869605, 1.000000000000000000, 0.9238795325112869605, 1.000000000000000000, 0.9238795325112869605, 1.000000000000000000, 0.9238795325112869605, 1.000000000000000000, 0.9238795325112869605, 1.000000000000000000, 0.9238795325112869605, 1.000000000000000000, 0.9238795325112869605, 1.000000000000000000, 0.9238795325112869605, 1.000000000000000000, 0.9238795325112869605, 1.000000000000000000, 0.9238795325112869605, 1.000000000000000000, 0.9238795325112869605, 1.000000000000000000, 0.9238795325112869605, 1.000000000000000000, 0.9238795325112869605, 1.000000000000000000, 0.9238795325112869605, 1.000000000000000000, 0.9238795325112869605, 1.000000000000000000, 0.9238795325112869605, 1.000000000000000000, 0.9238795325112869605, 1.000000000000000000, 0.9238795325112869605, 1.000000000000000000, 0.9238795325112869605, 1.000000000000000000, 0.9238795325112869605, 1.000000000000000000, 0.9238795325112869605, 1.000000000000000000, 0.9238795325112869605, 1.000000000000000000, 0.9238795325112869605, 1.000000000000000000, 0.9238795325112869605, 1.000000000000000000, 0.9238795325112869605, 1.000000000000000000, 0.9238795325112869605, 1.000000000000000000, 0.9238795325112869605, 1.000000000000000000, 0.9238795325112869605, 1.000000000000000000, 0.9238795325112869605, 1.000000000000000000, 0.9238795325112869605, 1.000000000000000000, 0.9238795325112869605, 1.000000000000000000, 0.9238795325112869605, 1.000000000000000000, 0.9238795325112869605, 1.000000000000000000, 0.9238795325112869605, 1.000000000000000000, 0.9238795325112869605, 1.000000000000000000, 0.9238795325112869605, 1.000000000000000000, 0.9238795325112869605, 1.000000000000000000, 0.9238795325112869605, 1.000000000000000000, 0.9238795325112869605, 1.000000000000000000),
 ( 1.000000000000000000, 0.9238795325112869605, 1.000000000000000000, 0.9238795325112869605, 1.000000000000000000, 0.9238795325112869605, 1.000000000000000000, 0.9238795325112869605, 1.000000000000000000, 0.9238795325112869605, 1.000000000000000000, 0.9238795325112869605, 1.000000000000000000, 0.9238795325112869605, 1.000000000000000000, 0.9238795325112869605, 1.000000000000000000, 0.9238795325112869605, 1.000000000000000000, 0.9238795325112869605, 1.000000000000000000, 0.9238795325112869605, 1.000000000000000000, 0.9238795325112869605, 1.000000000000000000, 0.9238795325112869605, 1.000000000000000000, 0.9238795325112869605, 1.000000000000000000, 0.9238795325112869605, 1.000000000000000000, 0.9238795325112869605, 1.000000000000000000, 0.9238795325112869605, 1.000000000000000000, 0.9238795325112869605, 1.000000000000000000, 0.9238795325112869605, 1.000000000000000000, 0.9238795325112869605, 1.000000000000000000, 0.9238795325112869605, 1.000000000000000000, 0.9238795325112869605, 1.000000000000000000, 0.9238795325112869605, 1.000000000000000000, 0.9238795325112869605, 1.000000000000000000, 0.9238795325112869605, 1.000000000000000000, 0.9238795325112869605, 1.000000000000000000, 0.9238795325112869605, 1.000000000000000000, 0.9238795325112869605, 1.000000000000000000, 0.9238795325112869605, 1.000000000000000000, 0.9238795325112869605, 1.000000000000000000, 0.9238795325112869605, 1.000000000000000000, 0.9238795325112869605, 1.000000000000000000, 0.9238795325112869605, 1.000000000000000000, 0.9238795325112869605, 1.000000000000000000, 0.9238795325112869605, 1.000000000000000000, 0.9238795325112869605, 1.000000000000000000, 0.9238795325112869605, 1.000000000000000000, 0.9238795325112869605, 1.000000000000000000, 0.9238795325112869605, 1.000000000000000000, 0.9238795325112869605, 1.000000000000000000, 0.9238795325112869605, 1.000000000000000000, 0.9238795325112869605, 1.000000000000000000, 0.9238795325112869605, 1.000000000000000000, 0.9238795325112869605, 1.000000000000000000, 0.9238795325112869605, 1.000000000000000000, 0.9238795325112869605, 1.000000000000000000, 0.9238795325112869605, 1.000000000000000000, 0.9238795325112869605, 1.000000000000000000, 0.9238795325112869605, 1.000000000000000000, 0.9238795325112869605, 1.000000000000000000, 0.9238795325112869605, 1.000000000000000000, 0.9238795325112869605, 1.000000000000000000, 0.9238795325112869605, 1.000000000000000000, 0.9238795325112869605, 1.000000000000000000, 0.9238795325112869605, 1.000000000000000000, 0.9238795325112869605, 1.000000000000000000, 0.9238795325112869605, 1.000000000000000000, 0.9238795325112869605, 1.000000000000000000, 0.9238795325112869605, 1.000000000000000000, 0.9238795325112869605, 1.000000000000000000, 0.9238795325112869605, 1.000000000000000000, 0.9238795325112869605, 1.000000000000000000, 0.9238795325112869605, 1.000000000000000000, 0.9238795325112869605, 1.000000000000000000, 0.9238795325112869605, 1.000000000000000000, 0.9238795325112869605, 1.000000000000000000, 0.9238795325112869605, 1.000000000000000000, 0.9238795325112869605, 1.000000000000000000, 0.9238795325112869605, 1.000000000000000000, 0.9238795325112869605, 1.000000000000000000, 0.9238795325112869605, 1.000000000000000000, 0.9238795325112869605, 1.000000000000000000, 0.9238795325112869605, 1.000000000000000000, 0.9238795325112869605, 1.000000000000000000, 0.9238795325112869605, 1.000000000000000000, 0.9238795325112869605, 1.000000000000000000, 0.9238795325112869605, 1.000000000000000000, 0.9238795325112869605, 1.000000000000000000, 0.9238795325112869605, 1.000000000000000000, 0.9238795325112869605, 1.000000000000000000) ) ) 
 REPRESENTATION_ITEM ( '' )  SURFACE ( )  );
#35466 = CARTESIAN_POINT ( 'NONE',  ( 116.6536748109119941, -10.15424416112533912, -14.75197769757731336 ) ) ;
#35467 = CARTESIAN_POINT ( 'NONE',  ( 96.21525317080913453, -25.71306530104311605, -15.42404253659028335 ) ) ;
#35468 = CARTESIAN_POINT ( 'NONE',  ( 111.1770983795247787, -0.7896495226426338832, -9.318865927141430916 ) ) ;
#35469 = CARTESIAN_POINT ( 'NONE',  ( 121.5888948109119809, 0.1319031606808879209, -14.10382304977623669 ) ) ;
#35470 = CARTESIAN_POINT ( 'NONE',  ( 125.3328548109119964, -0.8288870151387760510, -10.36305467784173118 ) ) ;
#35471 = CARTESIAN_POINT ( 'NONE',  ( 116.2471765045247594, -2.791137627527887410, -8.388885654883788234 ) ) ;
#35472 = CARTESIAN_POINT ( 'NONE',  ( 109.2294423643528347, -4.911049476578604356, -7.814831654473923805 ) ) ;
#35473 = CARTESIAN_POINT ( 'NONE',  ( 119.1878298109119783, -7.200787124940443817, -17.81845355600750835 ) ) ;
#35474 = VECTOR ( 'NONE', #17699, 1000.000000000000000 ) ;
#35475 = CARTESIAN_POINT ( 'NONE',  ( 113.1912390045248031, 0.8980012041604421569, -15.77991374673208469 ) ) ;
#35476 = DIRECTION ( 'NONE',  ( 1.000000000000000000, 1.671245155169139691E-16, 0.000000000000000000 ) ) ;
#35477 = CARTESIAN_POINT ( 'NONE',  ( 116.8238548109119819, -4.089484607189486809, -7.948022111789456723 ) ) ;
#35478 = CARTESIAN_POINT ( 'NONE',  ( 114.6682414775786469, -1.561330072975668060, -17.79121239304076596 ) ) ;
#35479 = CARTESIAN_POINT ( 'NONE',  ( 110.5520202545248054, -10.62599879583958717, -15.77991374673208469 ) ) ;
#35480 = CARTESIAN_POINT ( 'NONE',  ( 114.2144281442453178, -8.166667518702817929, -8.995218007635859436 ) ) ;
#35481 = ORIENTED_EDGE ( 'NONE', *, *, #25820, .F. ) ;
#35482 = DIRECTION ( 'NONE',  ( -0.000000000000000000, -0.9284778069183721172, -0.3713878862591650232 ) ) ;
#35483 = CARTESIAN_POINT ( 'NONE',  ( 124.5386814775786206, -5.638512984488999180, -18.83840828888717311 ) ) ;
#35484 = CARTESIAN_POINT ( 'NONE',  ( 116.1998614775786507, -10.63000616557722466, -14.87417383870573495 ) ) ;
#35485 = CARTESIAN_POINT ( 'NONE',  ( 121.1350814775786233, -9.859900752359378018, -12.68260735090039759 ) ) ;
#35486 = APPLICATION_PROTOCOL_DEFINITION ( 'draft international standard', 'automotive_design', 1998, #11383 ) ;
#35487 = CARTESIAN_POINT ( 'NONE',  ( 123.8012348109119642, 0.2603800115204892296, -16.42320221600525088 ) ) ;
#35488 = CARTESIAN_POINT ( 'NONE',  ( 122.4965214775786251, -10.30919188438810075, -12.61870101168855918 ) ) ;
#35489 = AXIS2_PLACEMENT_3D ( 'NONE', #32716, #15636, #26574 ) ;
#35490 = CARTESIAN_POINT ( 'NONE',  ( 113.2606921295247702, 0.8980012041604618078, -13.39321520033831447 ) ) ;
#35491 = ADVANCED_FACE ( 'NONE', ( #2207 ), #5505, .F. ) ;
#35492 = CARTESIAN_POINT ( 'NONE',  ( 117.3911214775786505, -7.894159318335828068, -9.358103419637847864 ) ) ;
#35493 = CARTESIAN_POINT ( 'NONE',  ( 123.6328298109119714, -2.173413727453600508, -8.297982527556802879 ) ) ;
#35494 = CARTESIAN_POINT ( 'NONE',  ( 121.9470836909669913, -27.84333996136784961, -14.15691383771150136 ) ) ;
#35495 = ORIENTED_EDGE ( 'NONE', *, *, #24743, .T. ) ;
#35496 = CARTESIAN_POINT ( 'NONE',  ( 120.4543614775786295, -4.089484607189486809, -7.948022111789456723 ) ) ;
#35497 = CARTESIAN_POINT ( 'NONE',  ( 120.0907204359119760, -10.25716656981731489, -12.88942061488890545 ) ) ;
#35498 = CARTESIAN_POINT ( 'NONE',  ( 120.1140014775786398, -1.561330072975668504, -17.79121239304076951 ) ) ;
#35499 = ORIENTED_EDGE ( 'NONE', *, *, #22969, .F. ) ;
#35500 = CARTESIAN_POINT ( 'NONE',  ( 115.9693640045247776, -10.62599879583958717, -11.00651665394454604 ) ) ;
#35501 = CARTESIAN_POINT ( 'NONE',  ( -13.37983193548284611, -5.027122839767540263, -8.598763672831253757 ) ) ;
#35503 = CARTESIAN_POINT ( 'NONE',  ( 119.6392035773848761, -2.467220198592778413, -17.83387418641524391 ) ) ;
#35502 = CIRCLE ( 'NONE', #27528, 0.3000000000000022093 ) ;
#35504 = CARTESIAN_POINT ( 'NONE',  ( 116.8238548109119819, -5.574606645277164318, -18.38911715685844683 ) ) ;
#35505 = CARTESIAN_POINT ( 'NONE',  ( 88.93653725331050452, -10.83229915613791761, -14.14321520033831625 ) ) ;
#35506 = CARTESIAN_POINT ( 'NONE',  ( 124.5176775718272069, -9.754195700035083405, -12.35076824631977566 ) ) ;
#35507 = CARTESIAN_POINT ( 'NONE',  ( 119.3765548109119834, -10.15424416112533912, -14.75197769757731336 ) ) ;
#35508 = DIRECTION ( 'NONE',  ( 0.000000000000000000, -0.3818493186865927203, 0.9242245927363029745 ) ) ;
#35509 = CARTESIAN_POINT ( 'NONE',  ( 120.1707281442453166, -9.565557343593413364, -10.61323700422348004 ) ) ;
#35510 = CARTESIAN_POINT ( 'NONE',  ( 125.3303382280814020, -10.92430497713086979, -9.659021213111804727 ) ) ;
#35511 = CARTESIAN_POINT ( 'NONE',  ( 118.0151148109119816, 0.4262465694468514643, -12.03445270309931736 ) ) ;
#35512 = CARTESIAN_POINT ( 'NONE',  ( 111.9453614775786434, -1.561330072975668060, -17.79121239304076596 ) ) ;
#35513 = CARTESIAN_POINT ( 'NONE',  ( 117.9583881442453048, -10.30919188438810075, -12.61870101168855918 ) ) ;
#35514 = CARTESIAN_POINT ( 'NONE',  ( 113.1366214775786432, -1.834011780172310813, -8.268836392978581529 ) ) ;
#35515 = FACE_OUTER_BOUND ( 'NONE', #41576, .T. ) ;
#35516 = CARTESIAN_POINT ( 'NONE',  ( 120.3976348109119812, -7.643976991954077427, -18.09477374809248928 ) ) ;
#35517 = ORIENTED_EDGE ( 'NONE', *, *, #36407, .F. ) ;
#35518 = CARTESIAN_POINT ( 'NONE',  ( 121.8725281442453223, -3.383040157471821630, -19.15922257007629170 ) ) ;
#35519 = CARTESIAN_POINT ( 'NONE',  ( 114.5803015045248117, -6.936859964151250502, -18.39754474579286025 ) ) ;
#35520 = CARTESIAN_POINT ( 'NONE',  ( 69.69189222814998175, -41.76310523276723785, -6.393215200338315363 ) ) ;
#35521 = CARTESIAN_POINT ( 'NONE',  ( 128.2184548109119930, 1.087851763053662602, -12.63461456455805276 ) ) ;
#35522 = CARTESIAN_POINT ( 'NONE',  ( 122.4280705993907645, -9.245649465415468171, -16.16453161350215950 ) ) ;
#35523 = CARTESIAN_POINT ( 'NONE',  ( 124.7655881442452852, 0.5811942927096110934, -14.16772938898807510 ) ) ;
#35524 = VERTEX_POINT ( 'NONE', #10425 ) ;
#35525 = APPLICATION_CONTEXT ( 'automotive_design' ) ;
#35526 = CARTESIAN_POINT ( 'NONE',  ( 70.19189222814998175, -53.90613343638955968, -34.76527462071035046 ) ) ;
#35527 = CARTESIAN_POINT ( 'NONE',  ( 120.1140014775786398, -7.894159318335828068, -9.358103419637847864 ) ) ;
#35528 = CARTESIAN_POINT ( 'NONE',  ( 74.43213512091445239, -36.61236768192972590, -12.39321520033831447 ) ) ;
#35529 = CARTESIAN_POINT ( 'NONE',  ( 62.52445501936042405, -14.54538235898669285, -17.51060916224595942 ) ) ;
#35530 = CARTESIAN_POINT ( 'NONE',  ( 114.6490365460471992, -2.191907684172563986, -18.20049396185734025 ) ) ;
#35531 = CARTESIAN_POINT ( 'NONE',  ( 110.6214733795247867, -1.325403438956436419, -9.854619843455211026 ) ) ;
#35532 = ORIENTED_EDGE ( 'NONE', *, *, #39875, .F. ) ;
#35533 = CARTESIAN_POINT ( 'NONE',  ( 114.4980614775786592, -7.893985811506177619, -18.51759400769804742 ) ) ;
#35534 = CARTESIAN_POINT ( 'NONE',  ( 114.4980614775786592, -7.893985811506177619, -18.51759400769804742 ) ) ;
#35535 = CARTESIAN_POINT ( 'NONE',  ( 88.50659967646818416, -11.40089054768302468, -13.90724332495447868 ) ) ;
#35536 = CARTESIAN_POINT ( 'NONE',  ( 120.2841814775786276, -10.15424416112533912, -14.75197769757731336 ) ) ;
#35537 = VECTOR ( 'NONE', #7493, 1000.000000000000000 ) ;
#35538 = CARTESIAN_POINT ( 'NONE',  ( 112.3424481442453384, -3.505236298600246325, -18.68346056562440793 ) ) ;
#35539 = B_SPLINE_CURVE_WITH_KNOTS ( 'NONE', 3,
 ( #29485, #11496, #25401, #11944, #39531, #36312, #39299, #42949, #39748, #5082, #19229, #12395, #43398, #22643, #8069, #26295, #33110, #4861, #8968, #40202, #19448 ),
 .UNSPECIFIED., .F., .F.,
 ( 4, 2, 2, 1, 1, 2, 2, 2, 1, 2, 2, 4 ),
 ( 0.000000000000000000, 0.2500000000000362488, 0.3750000000000469624, 0.4375000000000521250, 0.4687500000000549005, 0.4843750000000563438, 0.5000000000000577316, 0.6250000000000136557, 0.6875000000000022204, 0.7187499999999964473, 0.7499999999999905631, 1.000000000000000000 ),
 .UNSPECIFIED. ) ;
#35540 = SURFACE_SIDE_STYLE ('',( #17562 ) ) ;
#35541 = CARTESIAN_POINT ( 'NONE',  ( 121.9859814775786333, 0.2603800115204892296, -16.42320221600525088 ) ) ;
#35542 = CARTESIAN_POINT ( 'NONE',  ( 111.5588148109119828, 0.08617673920517221475, -14.09731900820172967 ) ) ;
#35543 = CARTESIAN_POINT ( 'NONE',  ( 27.57768543387103222, -14.97172645945875935, -8.893215200338314474 ) ) ;
#35544 = CARTESIAN_POINT ( 'NONE',  ( 84.49707967414211396, -26.75858941326842810, -11.54476601486570964 ) ) ;
#35545 = FACE_OUTER_BOUND ( 'NONE', #36655, .T. ) ;
#35546 = VERTEX_POINT ( 'NONE', #24333 ) ;
#35547 = DIRECTION ( 'NONE',  ( -1.000000000000000000, 0.000000000000000000, 0.000000000000000000 ) ) ;
#35548 = CARTESIAN_POINT ( 'NONE',  ( 118.9794681442453026, -9.261995988541697145, -16.69588392320189030 ) ) ;
#35549 = CARTESIAN_POINT ( 'NONE',  ( 136.5935259641917412, -10.11762552186683450, -15.62548657175932476 ) ) ;
#35550 = EDGE_LOOP ( 'NONE', ( #41647, #33688, #7461, #5721, #39619, #32748 ) ) ;
#35551 = CARTESIAN_POINT ( 'NONE',  ( 136.2632467228194173, 0.5429805449437086207, -11.18076796992574806 ) ) ;
#35552 = CARTESIAN_POINT ( 'NONE',  ( 125.4463081442452932, -5.638512984488999180, -18.83840828888717311 ) ) ;
#35553 = CARTESIAN_POINT ( 'NONE',  ( 111.3160046295247838, -4.863998795839541422, -18.39754474579285315 ) ) ;
#35554 = CARTESIAN_POINT ( 'NONE',  ( 124.4252281442452812, -0.8288870151387760510, -10.36305467784173118 ) ) ;
#35555 = EDGE_LOOP ( 'NONE', ( #34930, #11462, #42613, #39930 ) ) ;
#35556 = CARTESIAN_POINT ( 'NONE',  ( 119.8303681442453126, -10.63000616557722466, -14.87417383870573495 ) ) ;
#35557 = DIRECTION ( 'NONE',  ( 0.000000000000000000, -0.3818493186865927203, 0.9242245927363029745 ) ) ;
#35558 = CARTESIAN_POINT ( 'NONE',  ( 120.5678148109119832, -8.166667518702801942, -8.995218007635848778 ) ) ;
#35559 = CARTESIAN_POINT ( 'NONE',  ( 135.7778351054869859, -5.603397541288348549, -7.474883969788649551 ) ) ;
#35560 = EDGE_CURVE ( 'NONE', #4821, #32198, #25806, .T. ) ;
#35561 = CARTESIAN_POINT ( 'NONE',  ( 126.2404814775786264, -9.261995988541697145, -16.69588392320189030 ) ) ;
#35562 = CARTESIAN_POINT ( 'NONE',  ( 122.6540948253202998, -6.059724811980599313, -18.37735133589800540 ) ) ;
#35563 = AXIS2_PLACEMENT_3D ( 'NONE', #34148, #30286, #13426 ) ;
#35564 = DIRECTION ( 'NONE',  ( -0.4461977533474357771, -0.3417300876246960328, 0.8271203734159368048 ) ) ;
#35565 = CARTESIAN_POINT ( 'NONE',  ( 124.9924948109119924, -4.089484607189486809, -7.948022111789456723 ) ) ;
#35567 = CARTESIAN_POINT ( 'NONE',  ( 121.7590748109119687, -2.084020599724406786, -8.691656652584148546 ) ) ;
#35566 = CARTESIAN_POINT ( 'NONE',  ( 121.9859814775786333, 0.2603800115204892296, -16.42320221600525088 ) ) ;
#35568 = CARTESIAN_POINT ( 'NONE',  ( 120.2990798109119766, -7.200787124940443817, -17.81845355600750835 ) ) ;
#35569 = CARTESIAN_POINT ( 'NONE',  ( 122.7801548109119665, -6.222761293078241884, -8.102969835052219238 ) ) ;
#35570 = CARTESIAN_POINT ( 'NONE',  ( 113.3068014775786594, -1.833838273342658809, -17.42832698103878286 ) ) ;
#35571 = CARTESIAN_POINT ( 'NONE',  ( 121.2485348109119769, -0.4660016031367893996, -10.09054647747474043 ) ) ;
#35572 = ORIENTED_EDGE ( 'NONE', *, *, #861, .F. ) ;
#35573 = ORIENTED_EDGE ( 'NONE', *, *, #21018, .T. ) ;
#35574 = DIRECTION ( 'NONE',  ( 0.000000000000000000, 0.3818493186865927203, -0.9242245927363029745 ) ) ;
#35575 = DIRECTION ( 'NONE',  ( 1.000000000000000000, 0.000000000000000000, -0.000000000000000000 ) ) ;
#35576 = CARTESIAN_POINT ( 'NONE',  ( 115.6220983795247861, -8.402594152722688392, -16.93181055722141792 ) ) ;
#35577 = CARTESIAN_POINT ( 'NONE',  ( 114.3719421295247827, -9.868328341294093420, -13.39321520033831447 ) ) ;
#35578 = CARTESIAN_POINT ( 'NONE',  ( 125.7866681442452688, -0.4660016031367893996, -10.09054647747474043 ) ) ;
#35579 = CARTESIAN_POINT ( 'NONE',  ( 113.0798948109119948, -0.4660016031367893996, -10.09054647747474043 ) ) ;
#35580 = VERTEX_POINT ( 'NONE', #17268 ) ;
#35581 = ADVANCED_FACE ( 'NONE', ( #30941 ), #34782, .T. ) ;
#35582 = CARTESIAN_POINT ( 'NONE',  ( 114.2144281442453178, -1.833838273342658809, -17.42832698103878286 ) ) ;
#35583 = CARTESIAN_POINT ( 'NONE',  ( 108.3989733795248753, -8.938348069036489818, -17.46756447353520159 ) ) ;
#35584 = CARTESIAN_POINT ( 'NONE',  ( 61.69189222814998175, -40.21211973637273474, -6.893215200338315363 ) ) ;
#35585 = CARTESIAN_POINT ( 'NONE',  ( 119.8730187714538005, -6.306599966548167124, -18.84486539759072699 ) ) ;
#35586 = EDGE_CURVE ( 'NONE', #29714, #9856, #11088, .T. ) ;
#35587 = EDGE_CURVE ( 'NONE', #21924, #19363, #3252, .T. ) ;
#35588 = CARTESIAN_POINT ( 'NONE',  ( 109.2294647402427472, -0.3627424684288433343, -15.75041896508675521 ) ) ;
#35589 = DIRECTION ( 'NONE',  ( -1.000000000000000000, 0.000000000000000000, 0.000000000000000000 ) ) ;
#35590 = CARTESIAN_POINT ( 'NONE',  ( 115.0086014775786509, -4.089484607189486809, -7.948022111789456723 ) ) ;
#35591 = CARTESIAN_POINT ( 'NONE',  ( 115.9693640045247776, -10.62599879583958717, -11.00651665394454604 ) ) ;
#35592 = CARTESIAN_POINT ( 'NONE',  ( 110.4131140045248287, 0.1403307496149616695, -15.46607636864997204 ) ) ;
#35593 = EDGE_LOOP ( 'NONE', ( #20183, #44739, #10738, #976, #21706 ) ) ;
#35594 = CARTESIAN_POINT ( 'NONE',  ( 90.48265143217095385, -26.80230621008286107, -13.72680406592863456 ) ) ;
#35595 = CARTESIAN_POINT ( 'NONE',  ( 115.5191414775786569, -6.222761293078241884, -8.102969835052219238 ) ) ;
#35596 = CARTESIAN_POINT ( 'NONE',  ( 117.6180281442453150, -0.4660016031367893996, -10.09054647747474043 ) ) ;
#35597 = CARTESIAN_POINT ( 'NONE',  ( 125.4463081442452932, -4.153390946401325223, -8.397313243818185668 ) ) ;
#35598 = UNCERTAINTY_MEASURE_WITH_UNIT (LENGTH_MEASURE( 1.000000000000000082E-05 ), #33697, 'distance_accuracy_value', 'NONE');
#35599 = CARTESIAN_POINT ( 'NONE',  ( 119.8303681442453126, 0.4262465694468514643, -12.03445270309931736 ) ) ;
#35600 = CARTESIAN_POINT ( 'NONE',  ( 117.2776681442452968, -4.153390946401325223, -8.397313243818185668 ) ) ;
#35601 = VERTEX_POINT ( 'NONE', #31822 ) ;
#35602 = CARTESIAN_POINT ( 'NONE',  ( 120.5768923109119868, -9.959231468620755479, -10.70263013195267199 ) ) ;
#35603 = CIRCLE ( 'NONE', #30516, 2.999999999999998668 ) ;
#35604 = CARTESIAN_POINT ( 'NONE',  ( 121.7634181477679789, -2.280480477428469488, -18.08254604495227014 ) ) ;
#35605 = CARTESIAN_POINT ( 'NONE',  ( 116.3133148109120043, -2.084020599724406786, -8.691656652584148546 ) ) ;
#35606 = EDGE_LOOP ( 'NONE', ( #21944, #13259, #19422, #22649 ) ) ;
#35607 = CIRCLE ( 'NONE', #41474, 2.000000000000000444 ) ;
#35608 = CARTESIAN_POINT ( 'NONE',  ( 46.84966980880212617, -19.07391775237791620, -8.593215200338315540 ) ) ;
#35609 = CARTESIAN_POINT ( 'NONE',  ( 116.8805814775786445, -6.344957434206662583, -7.627207830600332805 ) ) ;
#35610 = CARTESIAN_POINT ( 'NONE',  ( 107.2877233795247776, -1.325403438956436419, -9.854619843455211026 ) ) ;
#35611 = CARTESIAN_POINT ( 'NONE',  ( 69.17459910784975818, -26.47815602666253909, -5.893215200338315363 ) ) ;
#35612 = EDGE_CURVE ( 'NONE', #2745, #27644, #15613, .T. ) ;
#35613 = VERTEX_POINT ( 'NONE', #17477 ) ;
#35614 = ORIENTED_EDGE ( 'NONE', *, *, #8956, .T. ) ;
#35615 = CARTESIAN_POINT ( 'NONE',  ( 118.9227414775786542, 0.4262465694468514643, -12.03445270309931736 ) ) ;
#35616 = CARTESIAN_POINT ( 'NONE',  ( 119.1496481442453046, -6.222761293078241884, -8.102969835052219238 ) ) ;
#35617 = CARTESIAN_POINT ( 'NONE',  ( 124.5747187774675808, -9.832980137052690139, -13.97121560461364709 ) ) ;
#35618 = EDGE_CURVE ( 'NONE', #19331, #19315, #4398, .T. ) ;
#35619 = CARTESIAN_POINT ( 'NONE',  ( 123.6328298109119714, -2.173413727453600508, -8.297982527556802879 ) ) ;
#35620 = EDGE_LOOP ( 'NONE', ( #34784, #30008, #30059 ) ) ;
#35621 = CARTESIAN_POINT ( 'NONE',  ( 85.15861813568058380, -24.14644159042263993, -12.62951656296512937 ) ) ;
#35622 = FACE_OUTER_BOUND ( 'NONE', #39520, .T. ) ;
#35623 = EDGE_CURVE ( 'NONE', #35134, #279, #36009, .T. ) ;
#35624 = CARTESIAN_POINT ( 'NONE',  ( 109.7185827545247889, -2.477300249445798297, -19.15521520033831138 ) ) ;
#35625 = CARTESIAN_POINT ( 'NONE',  ( 113.5904348109119866, -7.893985811506177619, -18.51759400769804742 ) ) ;
#35626 = CARTESIAN_POINT ( 'NONE',  ( 126.5241148109119393, -9.565557343593413364, -10.61323700422348004 ) ) ;
#35627 = CARTESIAN_POINT ( 'NONE',  ( 117.8449348109119938, -1.833838273342659253, -17.42832698103878286 ) ) ;
#35628 = DIRECTION ( 'NONE',  ( 0.2768435750659241079, 0.3568721902840695792, -0.8921882507333129819 ) ) ;
#35629 = VERTEX_POINT ( 'NONE', #41444 ) ;
#35630 = CARTESIAN_POINT ( 'NONE',  ( 118.6958348109119754, -3.505236298600246325, -18.68346056562440793 ) ) ;
#35631 = DIRECTION ( 'NONE',  ( 1.000000000000000000, 0.000000000000000000, -0.000000000000000000 ) ) ;
#35632 = CARTESIAN_POINT ( 'NONE',  ( 85.61003441325739516, -27.00049153487613651, -8.010338156994905034 ) ) ;
#35633 = CARTESIAN_POINT ( 'NONE',  ( 116.5944421295247793, -0.02276961308034231024, -12.14321520033831625 ) ) ;
#35634 = CIRCLE ( 'NONE', #5790, 2.999999999999996003 ) ;
#35635 = CARTESIAN_POINT ( 'NONE',  ( 116.5969481442453031, 0.5811942927096154232, -14.16772938898807155 ) ) ;
#35636 = VERTEX_POINT ( 'NONE', #7205 ) ;
#35637 = EDGE_CURVE ( 'NONE', #40373, #44289, #10202, .T. ) ;
#35638 = CARTESIAN_POINT ( 'NONE',  ( 117.2209414775786485, -7.893985811506177619, -18.51759400769804742 ) ) ;
#35639 = CARTESIAN_POINT ( 'NONE',  ( 114.4413348109119823, -9.261995988541698921, -16.69588392320188674 ) ) ;
#35640 = CARTESIAN_POINT ( 'NONE',  ( 113.6079577545248043, -7.250697342233347165, -7.631215200338321125 ) ) ;
#35641 = CARTESIAN_POINT ( 'NONE',  ( 116.4834948109119779, -1.561330072975668504, -17.79121239304076951 ) ) ;
#35642 = EDGE_CURVE ( 'NONE', #33098, #26479, #42576, .T. ) ;
#35643 = ADVANCED_FACE ( 'NONE', ( #6778 ), #22187, .T. ) ;
#35644 = CARTESIAN_POINT ( 'NONE',  ( 115.1787814775786387, -9.988377603198976828, -10.36322818467138340 ) ) ;
#35645 = DIRECTION ( 'NONE',  ( 0.000000000000000000, 0.000000000000000000, -1.000000000000000000 ) ) ;
#35646 = CARTESIAN_POINT ( 'NONE',  ( 70.19189222814998175, -57.98054017398621340, -36.39502311309316696 ) ) ;
#35647 = CARTESIAN_POINT ( 'NONE',  ( 107.6349890045248401, -9.868328341294098749, -11.32035403202665869 ) ) ;
#35648 = ORIENTED_EDGE ( 'NONE', *, *, #22385, .T. ) ;
#35649 = CARTESIAN_POINT ( 'NONE',  ( 115.7610046295247912, -4.863998795839590272, -7.631215200338315796 ) ) ;
#35650 = CARTESIAN_POINT ( 'NONE',  ( 109.2294894120781805, -5.138589313339342546, -18.58794946807955384 ) ) ;
#35651 = CARTESIAN_POINT ( 'NONE',  ( 117.3911214775786505, -7.894159318335828068, -9.358103419637847864 ) ) ;
#35652 = CARTESIAN_POINT ( 'NONE',  ( 64.64935471094501906, -13.15280763797862207, -11.37863450522776532 ) ) ;
#35653 = CARTESIAN_POINT ( 'NONE',  ( 116.8028015045247940, -6.936859964151250502, -18.39754474579286025 ) ) ;
#35654 = CARTESIAN_POINT ( 'NONE',  ( 114.5108483795247878, -8.402594152722688392, -16.93181055722141792 ) ) ;
#35655 = AXIS2_PLACEMENT_3D ( 'NONE', #43387, #1426, #4851 ) ;
#35656 = DIRECTION ( 'NONE',  ( -0.6383198453882292789, -0.7697712484781092934, 0.000000000000000000 ) ) ;
#35657 = CARTESIAN_POINT ( 'NONE',  ( 115.4624148109119943, -4.153390946401321671, -8.397313243818183892 ) ) ;
#35658 = CARTESIAN_POINT ( 'NONE',  ( 88.07785292173620917, -26.60966817898065884, -11.90521360603286816 ) ) ;
#35659 = B_SPLINE_CURVE_WITH_KNOTS ( 'NONE', 3,
 ( #15516, #4796, #32386, #42666, #29423, #19386, #33275, #5247, #18718, #19164 ),
 .UNSPECIFIED., .F., .F.,
 ( 4, 3, 3, 4 ),
 ( 0.000000000000000000, 0.0001671877548681254834, 0.0003343755096277640170, 0.0006463528481650629171 ),
 .UNSPECIFIED. ) ;
#35660 = CARTESIAN_POINT ( 'NONE',  ( 124.9924948109119924, -4.089484607189486809, -7.948022111789456723 ) ) ;
#35661 = CARTESIAN_POINT ( 'NONE',  ( 120.2274548109119934, 0.5811942927096110934, -14.16772938898807510 ) ) ;
#35662 = ORIENTED_EDGE ( 'NONE', *, *, #15439, .F. ) ;
#35663 = CARTESIAN_POINT ( 'NONE',  ( 119.3765548109119834, -10.15424416112533912, -14.75197769757731336 ) ) ;
#35664 = CARTESIAN_POINT ( 'NONE',  ( 89.12784890491134604, -25.99489077589524300, -13.39321520033831625 ) ) ;
#35665 = CARTESIAN_POINT ( 'NONE',  ( 118.7525614775786380, -8.166667518702819706, -8.995218007635861213 ) ) ;
#35666 = CARTESIAN_POINT ( 'NONE',  ( 118.1285681442453068, -2.084020599724406786, -8.691656652584148546 ) ) ;
#35667 = ORIENTED_EDGE ( 'NONE', *, *, #38421, .F. ) ;
#35668 = CARTESIAN_POINT ( 'NONE',  ( 120.9649014775786355, -6.222761293078241884, -8.102969835052219238 ) ) ;
#35669 = CARTESIAN_POINT ( 'NONE',  ( 121.5321681442453183, -9.988377603198976828, -10.36322818467138340 ) ) ;
#35670 = CIRCLE ( 'NONE', #22560, 2.445500000000004448 ) ;
#35671 = LINE ( 'NONE', #352, #4143 ) ;
#35672 = CARTESIAN_POINT ( 'NONE',  ( 109.7880358795247986, -0.7896495226426338832, -17.46756447353520159 ) ) ;
#35673 = DIRECTION ( 'NONE',  ( 0.000000000000000000, -0.3818493186865927203, 0.9242245927363029745 ) ) ;
#35674 = CARTESIAN_POINT ( 'NONE',  ( 111.8021765045248372, -2.791137627527939813, -8.388885654883777576 ) ) ;
#35675 = CARTESIAN_POINT ( 'NONE',  ( 118.0151148109119816, -10.63000616557722466, -14.87417383870573495 ) ) ;
#35676 = AXIS2_PLACEMENT_3D ( 'NONE', #38997, #28297, #920 ) ;
#35677 = CARTESIAN_POINT ( 'NONE',  ( 79.79010115959992788, 5.106172230548961188, -4.893215200338314474 ) ) ;
#35678 = CARTESIAN_POINT ( 'NONE',  ( 115.6893214775786447, -9.859900752359374465, -12.68260735090039404 ) ) ;
#35679 = DIRECTION ( 'NONE',  ( 0.000000000000000000, 0.000000000000000000, 1.000000000000000000 ) ) ;
#35680 = ADVANCED_FACE ( 'NONE', ( #369 ), #13482, .T. ) ;
#35681 = CARTESIAN_POINT ( 'NONE',  ( 119.7434548109119703, -12.49632558250451986, -9.362893955355607645 ) ) ;
#35682 = CARTESIAN_POINT ( 'NONE',  ( 109.8574890045247940, -9.868328341294098749, -11.32035403202665869 ) ) ;
#35683 = CARTESIAN_POINT ( 'NONE',  ( 122.0666209388149355, -2.287189184988711155, -18.07361239780447448 ) ) ;
#35684 = LINE ( 'NONE', #14277, #39152 ) ;
#35685 = DIRECTION ( 'NONE',  ( 1.000000000000000000, 0.000000000000000000, -0.000000000000000000 ) ) ;
#35687 = CARTESIAN_POINT ( 'NONE',  ( 120.6245414775786458, -9.988377603198976828, -10.36322818467138340 ) ) ;
#35686 = CARTESIAN_POINT ( 'NONE',  ( 60.37456837578754687, -13.41642734739171239, -7.433439893800085407 ) ) ;
#35688 = CARTESIAN_POINT ( 'NONE',  ( 118.9227414775786542, 0.4262465694468514643, -12.03445270309931736 ) ) ;
#35689 = CARTESIAN_POINT ( 'NONE',  ( 111.7751814775786556, -2.084020599724406786, -8.691656652584148546 ) ) ;
#35690 = ORIENTED_EDGE ( 'NONE', *, *, #13042, .T. ) ;
#35691 = CARTESIAN_POINT ( 'NONE',  ( 90.67797751089673852, -17.83979763915464289, -21.89321520033831447 ) ) ;
#35692 = CARTESIAN_POINT ( 'NONE',  ( 122.5532481442453019, -10.63000616557722466, -14.87417383870573495 ) ) ;
#35693 = CARTESIAN_POINT ( 'NONE',  ( 114.7886608795247696, -1.325403438956436419, -16.93181055722141792 ) ) ;
#35694 = CARTESIAN_POINT ( 'NONE',  ( 119.0929214775786278, -4.153390946401325223, -8.397313243818185668 ) ) ;
#35695 = CARTESIAN_POINT ( 'NONE',  ( 115.4624148109119943, -4.153390946401321671, -8.397313243818183892 ) ) ;
#35696 = CARTESIAN_POINT ( 'NONE',  ( 95.62170725701142260, -26.16577925485904288, -14.32829783019477432 ) ) ;
#35697 = CARTESIAN_POINT ( 'NONE',  ( 108.6767858795247861, -0.7896495226426338832, -17.46756447353520159 ) ) ;
#35698 = CARTESIAN_POINT ( 'NONE',  ( 120.0005481442453146, -4.153390946401325223, -8.397313243818185668 ) ) ;
#35699 = CARTESIAN_POINT ( 'NONE',  ( 123.4608748109119745, 0.4262465694468514643, -12.03445270309931736 ) ) ;
#35700 = CARTESIAN_POINT ( 'NONE',  ( 115.8048964071292914, 0.2518737723193609224, -14.64321520033831447 ) ) ;
#35701 = AXIS2_PLACEMENT_3D ( 'NONE', #40320, #26861, #12512 ) ;
#35702 = CARTESIAN_POINT ( 'NONE',  ( 109.2294487058530024, -3.686508270684544009, -7.993684625048021353 ) ) ;
#35703 = CARTESIAN_POINT ( 'NONE',  ( 121.6186891859119896, -1.406689858478933353, -17.56299727309130887 ) ) ;
#35704 = CARTESIAN_POINT ( 'NONE',  ( 116.2471765045247594, -7.250697342233347165, -19.15521520033831138 ) ) ;
#35705 = LINE ( 'NONE', #32510, #13154 ) ;
#35706 = CARTESIAN_POINT ( 'NONE',  ( 116.3133148109119759, -7.893985811506177619, -18.51759400769804742 ) ) ;
#35707 = CARTESIAN_POINT ( 'NONE',  ( 117.1642148109119859, -9.261995988541697145, -16.69588392320189030 ) ) ;
#35708 = CARTESIAN_POINT ( 'NONE',  ( 111.8021765045248372, -7.250697342233347165, -19.15521520033831138 ) ) ;
#35709 = EDGE_CURVE ( 'NONE', #11722, #23894, #41453, .T. ) ;
#35710 = CARTESIAN_POINT ( 'NONE',  ( 113.1366214775786432, -1.834011780172310813, -8.268836392978581529 ) ) ;
#35711 = ORIENTED_EDGE ( 'NONE', *, *, #15305, .F. ) ;
#35712 = CARTESIAN_POINT ( 'NONE',  ( 117.2537553496756715, -1.087735405160632718, -17.17288456429612253 ) ) ;
#35713 = TOROIDAL_SURFACE ( 'NONE', #43742, 1.500000000000000000, 0.5000000000000000000 ) ;
#35714 = CARTESIAN_POINT ( 'NONE',  ( 114.7816948109119863, 0.5811942927096154232, -14.16772938898807155 ) ) ;
#35715 = CARTESIAN_POINT ( 'NONE',  ( 122.7234281442452755, -4.153390946401325223, -8.397313243818185668 ) ) ;
#35717 = B_SPLINE_CURVE_WITH_KNOTS ( 'NONE', 3,
 ( #39105, #8103, #42538, #14490, #28185, #25657, #42314, #14268, #42092, #10855, #7875, #11073, #24750, #21783, #18586, #581, #28404, #11299, #38638, #24977, #15163, #1252, #7193, #7642, #18368, #18135, #7411, #21331, #29068, #42979 ),
 .UNSPECIFIED., .F., .F.,
 ( 4, 2, 2, 1, 1, 1, 2, 2, 2, 1, 1, 1, 2, 2, 1, 1, 2, 2, 4 ),
 ( 0.000000000000000000, 0.2499999999999678590, 0.3749999999999364952, 0.4374999999999213407, 0.4687499999999293343, 0.4843749999999326650, 0.4921874999999179545, 0.4999999999999032441, 0.6249999999998178124, 0.6874999999997751798, 0.7187499999997664091, 0.7343749999997620792, 0.7421874999997711830, 0.7499999999997802869, 0.8124999999998421263, 0.8437499999998633315, 0.8593749999998809841, 0.8749999999998986366, 1.000000000000000000 ),
 .UNSPECIFIED. ) ;
#35716 = CARTESIAN_POINT ( 'NONE',  ( 0.000000000000000000, 0.000000000000000000, 0.000000000000000000 ) ) ;
#35718 = VECTOR ( 'NONE', #2490, 1000.000000000000114 ) ;
#35719 = CARTESIAN_POINT ( 'NONE',  ( 111.9453614775786434, -7.894159318335828068, -9.358103419637847864 ) ) ;
#35720 = CARTESIAN_POINT ( 'NONE',  ( 123.6310548109119765, -5.638512984488999180, -18.83840828888717311 ) ) ;
#35721 = CARTESIAN_POINT ( 'NONE',  ( 114.6497546295247929, -4.863998795839590272, -7.631215200338315796 ) ) ;
#35722 = CARTESIAN_POINT ( 'NONE',  ( 117.9016614775786280, -0.1624402480850797581, -16.17319339645315424 ) ) ;
#35723 = CARTESIAN_POINT ( 'NONE',  ( 122.8688454359119646, -11.07370829466463569, -12.81314460846529002 ) ) ;
#35724 = LINE ( 'NONE', #35950, #25017 ) ;
#35725 = EDGE_LOOP ( 'NONE', ( #17065, #15263, #5002, #33519, #18047 ) ) ;
#35726 = CARTESIAN_POINT ( 'NONE',  ( 119.8823610609119754, -6.340755971794695078, -8.611740276972781771 ) ) ;
#35727 = CARTESIAN_POINT ( 'NONE',  ( 119.4900081442453086, -1.834011780172310813, -8.268836392978581529 ) ) ;
#35728 = ORIENTED_EDGE ( 'NONE', *, *, #29196, .T. ) ;
#35729 = CARTESIAN_POINT ( 'NONE',  ( 68.07789357685331311, -68.58957386525776201, -38.44539312525987640 ) ) ;
#35730 = CARTESIAN_POINT ( 'NONE',  ( 70.19189222814998175, -52.40967333247598248, -34.16669579553818181 ) ) ;
#35731 = AXIS2_PLACEMENT_3D ( 'NONE', #20746, #17328, #17543 ) ;
#35732 = CARTESIAN_POINT ( 'NONE',  ( 84.87879901378997261, -30.44422003934618814, -7.893215200338315363 ) ) ;
#35733 = CARTESIAN_POINT ( 'NONE',  ( 114.7249681442453237, -9.565557343593413364, -10.61323700422348004 ) ) ;
#35734 = CARTESIAN_POINT ( 'NONE',  ( 126.8848614667774939, -1.093441926320177338, -17.16528547817962291 ) ) ;
#35735 = CARTESIAN_POINT ( 'NONE',  ( 123.7644531642484225, -2.215723800389698184, -18.16877924232191788 ) ) ;
#35736 =( BOUNDED_CURVE ( )  B_SPLINE_CURVE ( 2, ( #24292, #27488, #38179, #45040, #6956, #20861, #34741, #33851, #25180, #39078, #17662, #7848, #3963, #7614, #327, #11502, #24949 ),
 .UNSPECIFIED., .F., .T. ) 
 B_SPLINE_CURVE_WITH_KNOTS ( ( 3, 2, 2, 2, 2, 2, 2, 2, 3 ),
 ( 0.3040431156034944515, 0.3125000000000000000, 0.3250000000000000111, 0.3375000000000000222, 0.3499999999999999778, 0.3624999999999999889, 0.3750000000000000000, 0.3875000000000000111, 0.3959568843965060037 ),
 .UNSPECIFIED. ) 
 CURVE ( )  GEOMETRIC_REPRESENTATION_ITEM ( )  RATIONAL_B_SPLINE_CURVE ( ( 0.9666851417651740608, 0.9485006404992000206, 1.000000000000000000, 0.9238795325112869605, 1.000000000000000000, 0.9238795325112869605, 1.000000000000000000, 0.9238795325112869605, 1.000000000000000000, 0.9238795325112869605, 1.000000000000000000, 0.9238795325112869605, 1.000000000000000000, 0.9238795325112869605, 1.000000000000000000, 0.9485006404991980222, 0.9666851417651760592 ) ) 
 REPRESENTATION_ITEM ( '' )  );
#35737 = CARTESIAN_POINT ( 'NONE',  ( 120.3976348109119812, -7.643976991954077427, -18.09477374809248928 ) ) ;
#35738 = CARTESIAN_POINT ( 'NONE',  ( 83.82415148905927538, -46.76310523276723785, -23.89321520033831803 ) ) ;
#35739 = CARTESIAN_POINT ( 'NONE',  ( 122.6099748109119929, -0.8288870151387760510, -10.36305467784173118 ) ) ;
#35740 = CIRCLE ( 'NONE', #40120, 5.500000000000001776 ) ;
#35741 = CARTESIAN_POINT ( 'NONE',  ( 125.0048763211397187, -12.00734914858023039, -10.87324543638115237 ) ) ;
#35742 = CARTESIAN_POINT ( 'NONE',  ( 124.1415948109119540, -3.505236298600246325, -18.68346056562440793 ) ) ;
#35743 = AXIS2_PLACEMENT_3D ( 'NONE', #22345, #39219, #915 ) ;
#35744 = CARTESIAN_POINT ( 'NONE',  ( 112.2857214775786474, -4.089484607189486809, -7.948022111789456723 ) ) ;
#35745 = CARTESIAN_POINT ( 'NONE',  ( 118.2420214775786320, -3.383040157471821630, -19.15922257007629170 ) ) ;
#35746 = CARTESIAN_POINT ( 'NONE',  ( 112.5126281442453120, -10.30919188438810075, -12.61870101168855918 ) ) ;
#35747 = DIRECTION ( 'NONE',  ( 0.000000000000000000, 0.000000000000000000, 1.000000000000000000 ) ) ;
#35748 = CARTESIAN_POINT ( 'NONE',  ( 119.4332814775786318, -8.899110576539710493, -16.42337572283490132 ) ) ;
#35749 = EDGE_LOOP ( 'NONE', ( #4615, #32428, #44027, #42573 ) ) ;
#35750 = CARTESIAN_POINT ( 'NONE',  ( 120.7379948109119709, -10.63000616557722466, -14.87417383870573495 ) ) ;
#35751 = CARTESIAN_POINT ( 'NONE',  ( 111.5938171295247940, 0.1403307496149613920, -13.39321520033831447 ) ) ;
#35752 = CARTESIAN_POINT ( 'NONE',  ( -1.932019669644797988, -4.762702382056356321, -19.39321520033831447 ) ) ;
#35753 = CARTESIAN_POINT ( 'NONE',  ( 91.38554522942851577, -26.60966817898065884, -11.90521360603286816 ) ) ;
#35754 = EDGE_CURVE ( 'NONE', #35430, #24400, #2150, .T. ) ;
#35755 = CARTESIAN_POINT ( 'NONE',  ( 118.7735460444391862, -1.267766418764730840, -16.93314635290706605 ) ) ;
#35756 = CARTESIAN_POINT ( 'NONE',  ( 124.4819548109119722, -7.893985811506177619, -18.51759400769804742 ) ) ;
#35757 = ORIENTED_EDGE ( 'NONE', *, *, #12253, .T. ) ;
#35758 = DIRECTION ( 'NONE',  ( -0.9908103287288504424, 0.1352586133457950590, -4.625929269271490844E-15 ) ) ;
#35759 = CARTESIAN_POINT ( 'NONE',  ( 120.8514481442452961, -2.084020599724406786, -8.691656652584148546 ) ) ;
#35760 = CARTESIAN_POINT ( 'NONE',  ( -13.38024818871938670, -5.026574971259677227, -18.19321520033831874 ) ) ;
#35761 = CARTESIAN_POINT ( 'NONE',  ( 61.87547515407200649, -14.47097414721605446, -17.80504224133693114 ) ) ;
#35762 = DIRECTION ( 'NONE',  ( 0.000000000000000000, 0.000000000000000000, -1.000000000000000000 ) ) ;
#35763 = CARTESIAN_POINT ( 'NONE',  ( 105.6208483795248299, -8.402594152722688392, -16.93181055722141792 ) ) ;
#35764 = ORIENTED_EDGE ( 'NONE', *, *, #31449, .T. ) ;
#35765 = CARTESIAN_POINT ( 'NONE',  ( 115.5758681442453053, -1.561330072975668060, -17.79121239304076951 ) ) ;
#35766 = CARTESIAN_POINT ( 'NONE',  ( 71.02242295334774269, -57.83840141005237712, -39.44297575155226809 ) ) ;
#35767 = AXIS2_PLACEMENT_3D ( 'NONE', #41070, #13908, #3194 ) ;
#35768 = CARTESIAN_POINT ( 'NONE',  ( 122.3830681442452857, -1.833838273342659697, -17.42832698103878286 ) ) ;
#35769 = CARTESIAN_POINT ( 'NONE',  ( 126.2940345447970998, -3.831033905170792675, -8.462449267509514428 ) ) ;
#35770 = CARTESIAN_POINT ( 'NONE',  ( 121.9292548109119849, -1.561330072975668948, -17.79121239304076951 ) ) ;
#35771 = CARTESIAN_POINT ( 'NONE',  ( 75.95778847736514194, -3.256761025687008537, -19.39321520033831447 ) ) ;
#35772 = DIRECTION ( 'NONE',  ( -0.9908103287288504424, 0.1352586133457950590, 0.000000000000000000 ) ) ;
#35773 =( LENGTH_UNIT ( ) NAMED_UNIT ( * ) SI_UNIT ( .MILLI., .METRE. ) );
#35774 = ORIENTED_EDGE ( 'NONE', *, *, #10847, .F. ) ;
#35775 = CARTESIAN_POINT ( 'NONE',  ( 115.3442858795247759, -8.402594152722688392, -9.854619843455216355 ) ) ;
#35776 = VECTOR ( 'NONE', #13017, 1000.000000000000000 ) ;
#35777 = EDGE_CURVE ( 'NONE', #21643, #28223, #37455, .T. ) ;
#35778 = CARTESIAN_POINT ( 'NONE',  ( 119.7736414775786358, -10.30919188438810075, -12.61870101168855918 ) ) ;
#35779 = CARTESIAN_POINT ( 'NONE',  ( 137.4443952029541549, -8.589549469794567571, -16.85306431102494074 ) ) ;
#35780 = ORIENTED_EDGE ( 'NONE', *, *, #40922, .F. ) ;
#35781 = CARTESIAN_POINT ( 'NONE',  ( 112.2289948109119848, -1.834011780172310813, -8.268836392978581529 ) ) ;
#35782 = CARTESIAN_POINT ( 'NONE',  ( 111.3213681442453264, -7.643976991954077427, -18.09477374809248928 ) ) ;
#35783 = CARTESIAN_POINT ( 'NONE',  ( 127.2313854076960808, -4.459849209109382429, -18.88486369543121413 ) ) ;
#35784 = CARTESIAN_POINT ( 'NONE',  ( 123.7445081442452874, -7.894159318335828068, -9.358103419637847864 ) ) ;
#35785 = EDGE_LOOP ( 'NONE', ( #27454, #11287, #14153, #29647 ) ) ;
#35786 = CARTESIAN_POINT ( 'NONE',  ( 117.1642148109119859, -9.261995988541697145, -16.69588392320189030 ) ) ;
#35787 = DIRECTION ( 'NONE',  ( 0.000000000000000000, 0.000000000000000000, -1.000000000000000000 ) ) ;
#35788 = DIRECTION ( 'NONE',  ( -0.2768435750659241079, -0.3568721902840695792, 0.8921882507333129819 ) ) ;
#35789 = CYLINDRICAL_SURFACE ( 'NONE', #16348, 1.587500000000000355 ) ;
#35790 = CARTESIAN_POINT ( 'NONE',  ( 111.8319081442453182, -4.153390946401321671, -8.397313243818183892 ) ) ;
#35791 = CARTESIAN_POINT ( 'NONE',  ( 78.69189222814998175, -49.76310523276715969, -40.89321520033831092 ) ) ;
#35792 = DIRECTION ( 'NONE',  ( -0.5735764363510450492, -0.3127926500124816878, 0.7570804645221038687 ) ) ;
#35793 = CARTESIAN_POINT ( 'NONE',  ( 121.8725281442453223, -3.383040157471821630, -19.15922257007629170 ) ) ;
#35794 = CARTESIAN_POINT ( 'NONE',  ( 123.9714148109119805, -8.899110576539710493, -16.42337572283490132 ) ) ;
#35795 = CARTESIAN_POINT ( 'NONE',  ( 116.7089049431057788, -7.157548453469082972, -17.96581380690969709 ) ) ;
#35796 = CARTESIAN_POINT ( 'NONE',  ( 122.4965214775786251, 0.1319031606808879209, -14.10382304977623669 ) ) ;
#35797 = CARTESIAN_POINT ( 'NONE',  ( 112.2857214775786474, -5.574606645277164318, -18.38911715685844683 ) ) ;
#35798 = CARTESIAN_POINT ( 'NONE',  ( 118.1285681442453068, -7.893985811506177619, -18.51759400769804742 ) ) ;
#35799 = VERTEX_POINT ( 'NONE', #16080 ) ;
#35800 = VERTEX_POINT ( 'NONE', #13119 ) ;
#35801 = CARTESIAN_POINT ( 'NONE',  ( 126.3115243456364709, -8.670208513534547023, -16.70688709793458671 ) ) ;
#35802 = CARTESIAN_POINT ( 'NONE',  ( 91.65862616933031859, -27.84333996136784961, -14.15691383771150136 ) ) ;
#35803 = CARTESIAN_POINT ( 'NONE',  ( 105.6208483795248299, -0.7896495226426338832, -9.318865927141430916 ) ) ;
#35804 = CARTESIAN_POINT ( 'NONE',  ( 112.3578015045248861, -6.936859964151250502, -18.39754474579286025 ) ) ;
#35805 = CARTESIAN_POINT ( 'NONE',  ( 125.1059481442453034, -1.833838273341870773, -17.42832698103818956 ) ) ;
#35806 = CARTESIAN_POINT ( 'NONE',  ( 113.4202548109119846, -10.30919188438810075, -12.61870101168855918 ) ) ;
#35807 = ORIENTED_EDGE ( 'NONE', *, *, #32097, .F. ) ;
#35808 = CARTESIAN_POINT ( 'NONE',  ( 111.8886348109120092, -6.222761293078241884, -8.102969835052219238 ) ) ;
#35809 = DIRECTION ( 'NONE',  ( -0.7962509850245486076, -0.6049664196031347974, 0.000000000000000000 ) ) ;
#35810 = DIRECTION ( 'NONE',  ( -1.000000000000000000, 0.000000000000000000, 0.000000000000000000 ) ) ;
#35811 = CARTESIAN_POINT ( 'NONE',  ( 112.3424481442453384, -3.505236298600246325, -18.68346056562440793 ) ) ;
#35812 = CARTESIAN_POINT ( 'NONE',  ( 122.7234281442452755, -4.153390946401307460, -8.397313243818183892 ) ) ;
#35813 = DIRECTION ( 'NONE',  ( 1.000000000000000000, 0.000000000000000000, -0.000000000000000000 ) ) ;
#35814 = CARTESIAN_POINT ( 'NONE',  ( 115.1787814775786387, -9.988377603198976828, -10.36322818467138340 ) ) ;
#35815 = DIRECTION ( 'NONE',  ( 1.000000000000000000, 0.000000000000000000, -0.000000000000000000 ) ) ;
#35816 = CARTESIAN_POINT ( 'NONE',  ( 111.6632702545248605, 0.1403307496149616695, -11.32035403202665336 ) ) ;
#35817 = ORIENTED_EDGE ( 'NONE', *, *, #18655, .T. ) ;
#35818 = CARTESIAN_POINT ( 'NONE',  ( 126.6390922358795734, -7.341185092770153631, -8.808989803355210313 ) ) ;
#35819 = CARTESIAN_POINT ( 'NONE',  ( 117.2209414775786485, -2.084020599724406786, -8.691656652584148546 ) ) ;
#35820 = CARTESIAN_POINT ( 'NONE',  ( 115.8027748109119841, -0.4660016031367893996, -10.09054647747474043 ) ) ;
#35821 = DIRECTION ( 'NONE',  ( 0.000000000000000000, 0.000000000000000000, 1.000000000000000000 ) ) ;
#35822 = CARTESIAN_POINT ( 'NONE',  ( 123.7445081442452874, -7.894159318335828068, -9.358103419637847864 ) ) ;
#35823 = CARTESIAN_POINT ( 'NONE',  ( 120.7379948109119709, 0.4262465694468514643, -12.03445270309931736 ) ) ;
#35824 = CARTESIAN_POINT ( 'NONE',  ( 114.5547881442453217, -4.153390946401321671, -8.397313243818183892 ) ) ;
#35825 = ORIENTED_EDGE ( 'NONE', *, *, #36601, .F. ) ;
#35826 = CARTESIAN_POINT ( 'NONE',  ( 119.8129079359119942, -5.444069387712269226, -19.60292469916370450 ) ) ;
#35827 = AXIS2_PLACEMENT_3D ( 'NONE', #4797, #35575, #4121 ) ;
#35828 = DIRECTION ( 'NONE',  ( -0.000000000000000000, -0.9284778069183721172, -0.3713878862591650232 ) ) ;
#35829 = CARTESIAN_POINT ( 'NONE',  ( 116.4834948109119779, -7.894159318335828068, -9.358103419637847864 ) ) ;
#35830 = ORIENTED_EDGE ( 'NONE', *, *, #17762, .F. ) ;
#35831 = CARTESIAN_POINT ( 'NONE',  ( 128.2184548109119930, -10.44474571748257041, -15.59668151425567650 ) ) ;
#35832 = CARTESIAN_POINT ( 'NONE',  ( 115.3489614775786407, -9.261995988541697145, -16.69588392320189030 ) ) ;
#35833 = CARTESIAN_POINT ( 'NONE',  ( 106.3848327545248651, -6.936859964151250502, -8.388885654883777576 ) ) ;
#35834 = CARTESIAN_POINT ( 'NONE',  ( 113.4769814775786330, 0.4262465694468514643, -12.03445270309931736 ) ) ;
#35835 = VERTEX_POINT ( 'NONE', #1934 ) ;
#35836 = CIRCLE ( 'NONE', #890, 1.610000000000000986 ) ;
#35837 = ORIENTED_EDGE ( 'NONE', *, *, #11933, .T. ) ;
#35838 = CARTESIAN_POINT ( 'NONE',  ( 123.2906948109119867, -1.833838273342659697, -17.42832698103878286 ) ) ;
#35839 = CARTESIAN_POINT ( 'NONE',  ( 117.3343948109119737, -6.222761293078241884, -8.102969835052219238 ) ) ;
#35840 = CARTESIAN_POINT ( 'NONE',  ( 124.5370249113216801, -9.838819348832451794, -12.88702400009979065 ) ) ;
#35841 = EDGE_CURVE ( 'NONE', #37865, #33593, #41503, .T. ) ;
#35842 = CARTESIAN_POINT ( 'NONE',  ( 121.0630641859119976, -0.8832429491016019485, -18.19431474523657855 ) ) ;
#35843 = EDGE_LOOP ( 'NONE', ( #2803, #21237 ) ) ;
#35844 = CARTESIAN_POINT ( 'NONE',  ( 112.1344032980735363, -8.920344330785875187, -16.33470576110396522 ) ) ;
#35845 = CARTESIAN_POINT ( 'NONE',  ( 112.5661608795247872, -8.938348069036489818, -9.318865927141430916 ) ) ;
#35846 = CARTESIAN_POINT ( 'NONE',  ( 112.9097148109120070, 0.2603800115204892296, -16.42320221600525088 ) ) ;
#35847 = CARTESIAN_POINT ( 'NONE',  ( 112.3424481442453384, -6.344957434206662583, -7.627207830600332805 ) ) ;
#35848 = CARTESIAN_POINT ( 'NONE',  ( 121.5888948109119809, 0.1319031606808879209, -14.10382304977623669 ) ) ;
#35849 = CARTESIAN_POINT ( 'NONE',  ( 143.3676850761856940, -71.37806158163373027, -41.02281774838946404 ) ) ;
#35850 = VERTEX_POINT ( 'NONE', #29985 ) ;
#35851 = CARTESIAN_POINT ( 'NONE',  ( 121.5321681442453183, -0.1624402480850797581, -16.17319339645315424 ) ) ;
#35852 = CARTESIAN_POINT ( 'NONE',  ( 71.31713442278437753, 2.423123680056944007, -15.89321520033831447 ) ) ;
#35853 = CIRCLE ( 'NONE', #42463, 5.500000000000001776 ) ;
#35854 = LINE ( 'NONE', #8963, #9294 ) ;
#35855 = CARTESIAN_POINT ( 'NONE',  ( 116.0388171295248014, -10.62599879583958540, -13.39321520033831447 ) ) ;
#35856 = CARTESIAN_POINT ( 'NONE',  ( 117.1642148109119859, -9.261995988541697145, -16.69588392320189030 ) ) ;
#35857 = VERTEX_POINT ( 'NONE', #40251 ) ;
#35858 = CARTESIAN_POINT ( 'NONE',  ( 116.5969481442453031, 0.5811942927096154232, -14.16772938898807155 ) ) ;
#35859 = CARTESIAN_POINT ( 'NONE',  ( 115.1796143740715763, -2.419733177069680607, -17.89711025544712442 ) ) ;
#35860 = CARTESIAN_POINT ( 'NONE',  ( 113.3301452545248083, 0.8980012041604421569, -11.00651665394454071 ) ) ;
#35861 = CARTESIAN_POINT ( 'NONE',  ( 115.2922348109119781, -10.63000616557722466, -14.87417383870573495 ) ) ;
#35862 = CARTESIAN_POINT ( 'NONE',  ( 117.3911214775786505, -1.561330072975668504, -17.79121239304076951 ) ) ;
#35863 = PRODUCT_DEFINITION_FORMATION_WITH_SPECIFIED_SOURCE ( 'ANY', '', #35013, .NOT_KNOWN. ) ;
#35864 = CARTESIAN_POINT ( 'NONE',  ( 126.5254139958964572, -10.01703884201283223, -13.32492638032154098 ) ) ;
#35865 = DIRECTION ( 'NONE',  ( 0.000000000000000000, 0.000000000000000000, -1.000000000000000000 ) ) ;
#35866 = CARTESIAN_POINT ( 'NONE',  ( 107.8433483795247838, -8.402594152722688392, -16.93181055722141792 ) ) ;
#35867 = ADVANCED_FACE ( 'NONE', ( #40706 ), #23377, .T. ) ;
#35868 = ORIENTED_EDGE ( 'NONE', *, *, #22583, .F. ) ;
#35869 = AXIS2_PLACEMENT_3D ( 'NONE', #24749, #35216, #25207 ) ;
#35870 = DIRECTION ( 'NONE',  ( -0.2425356250363335242, -0.5825562349001200957, 0.7757607258473654399 ) ) ;
#35871 = CARTESIAN_POINT ( 'NONE',  ( 109.2294421713136359, -9.862771980732020438, -10.64487995292914668 ) ) ;
#35872 = CARTESIAN_POINT ( 'NONE',  ( 120.3976348109119812, -7.643976991954077427, -18.09477374809248928 ) ) ;
#35873 = CARTESIAN_POINT ( 'NONE',  ( 112.0799890045248475, -9.868328341294098749, -11.32035403202665869 ) ) ;
#35874 = CARTESIAN_POINT ( 'NONE',  ( 114.2330358795247776, -8.402594152722688392, -9.854619843455216355 ) ) ;
#35875 = DIRECTION ( 'NONE',  ( 0.000000000000000000, -0.9242245927363028635, -0.3818493186865930533 ) ) ;
#35876 = CARTESIAN_POINT ( 'NONE',  ( 112.7395348109119766, -4.153390946401321671, -8.397313243818183892 ) ) ;
#35877 = DIRECTION ( 'NONE',  ( 0.000000000000000000, 0.9284778069183722282, 0.3713878862591645791 ) ) ;
#35878 = EDGE_CURVE ( 'NONE', #14664, #37700, #15348, .T. ) ;
#35879 = CARTESIAN_POINT ( 'NONE',  ( 123.4608748109119745, -10.63000616557722466, -14.87417383870573495 ) ) ;
#35880 = CARTESIAN_POINT ( 'NONE',  ( 118.6958348109119754, -6.344957434206665248, -7.627207830600338134 ) ) ;
#35881 = ORIENTED_EDGE ( 'NONE', *, *, #44846, .T. ) ;
#35882 = ADVANCED_FACE ( 'NONE', ( #9695 ), #20735, .T. ) ;
#35883 = CARTESIAN_POINT ( 'NONE',  ( 117.5045748109119756, -9.859900752359374465, -12.68260735090039404 ) ) ;
#35884 = FACE_OUTER_BOUND ( 'NONE', #36712, .T. ) ;
#35885 = CARTESIAN_POINT ( 'NONE',  ( 119.7736414775786358, -10.30919188438810075, -12.61870101168855918 ) ) ;
#35886 = CARTESIAN_POINT ( 'NONE',  ( 120.7947214775786193, -0.8288870151387760510, -10.36305467784173118 ) ) ;
#35887 = VERTEX_POINT ( 'NONE', #16312 ) ;
#35888 = CARTESIAN_POINT ( 'NONE',  ( 116.3069962859068909, -1.111561923218680858, -17.14115599315434935 ) ) ;
#35889 = EDGE_CURVE ( 'NONE', #18915, #17900, #22940, .T. ) ;
#35890 = CIRCLE ( 'NONE', #13375, 4.500000000000003553 ) ;
#35891 = CIRCLE ( 'NONE', #19900, 2.000000000000000444 ) ;
#35892 = CARTESIAN_POINT ( 'NONE',  ( 119.0929214775786278, -5.638512984488999180, -18.83840828888717311 ) ) ;
#35893 = CARTESIAN_POINT ( 'NONE',  ( 124.9774582100001510, -5.997229896066199828, -5.873468846220863071 ) ) ;
#35894 = CARTESIAN_POINT ( 'NONE',  ( 110.7603796295247918, -4.863998795839590272, -19.15521520033831493 ) ) ;
#35895 = EDGE_CURVE ( 'NONE', #44381, #10447, #3950, .T. ) ;
#35896 = EDGE_CURVE ( 'NONE', #43873, #31663, #17801, .T. ) ;
#35897 = ADVANCED_FACE ( 'NONE', ( #33607 ), #33842, .T. ) ;
#35898 = CARTESIAN_POINT ( 'NONE',  ( 62.36331481590491421, -14.51968798477309797, -9.194700042550184804 ) ) ;
#35899 = CARTESIAN_POINT ( 'NONE',  ( 138.2184548109119930, -5.849744126848086090, -20.32346094940048786 ) ) ;
#35900 = CARTESIAN_POINT ( 'NONE',  ( 112.2883483795247770, -8.402594152722688392, -16.93181055722141792 ) ) ;
#35901 = CIRCLE ( 'NONE', #12633, 2.999999999999999556 ) ;
#35902 = CARTESIAN_POINT ( 'NONE',  ( 117.5045748109119756, 0.5811942927096110934, -14.16772938898807510 ) ) ;
#35903 = CARTESIAN_POINT ( 'NONE',  ( 136.3568202015727024, -10.22787683451856999, -11.16363433356868562 ) ) ;
#35904 = CARTESIAN_POINT ( 'NONE',  ( 116.1998614775786507, 0.4262465694468514643, -12.03445270309931736 ) ) ;
#35905 = CARTESIAN_POINT ( 'NONE',  ( 124.5954081442453116, -3.383040157471821630, -19.15922257007629170 ) ) ;
#35906 = DIRECTION ( 'NONE',  ( 0.9609149988134837450, -0.1028163501681639419, 0.2570431154366518145 ) ) ;
#35907 = CARTESIAN_POINT ( 'NONE',  ( 112.3807811052981691, 0.4930828106259610433, -12.14321520033829849 ) ) ;
#35908 = CARTESIAN_POINT ( 'NONE',  ( 111.3160046295247838, -4.863998795839590272, -18.39754474579285315 ) ) ;
#35909 = CARTESIAN_POINT ( 'NONE',  ( 114.2144281442453178, -1.833838273342658809, -17.42832698103878286 ) ) ;
#35910 = CARTESIAN_POINT ( 'NONE',  ( 87.41631446019775353, -25.99489077589524300, -13.39321520033831625 ) ) ;
#35911 = FACE_OUTER_BOUND ( 'NONE', #24021, .T. ) ;
#35913 = CARTESIAN_POINT ( 'NONE',  ( 119.3198281442452924, 0.5811942927096110934, -14.16772938898807510 ) ) ;
#35912 = CARTESIAN_POINT ( 'NONE',  ( 64.65536759514621679, -15.48292270431935336, -11.12858986817582441 ) ) ;
#35914 = CARTESIAN_POINT ( 'NONE',  ( 120.1140014775786398, -7.894159318335828068, -9.358103419637847864 ) ) ;
#35915 = CARTESIAN_POINT ( 'NONE',  ( 113.9875214775786532, -8.899110576539710493, -16.42337572283490132 ) ) ;
#35916 = ORIENTED_EDGE ( 'NONE', *, *, #11278, .T. ) ;
#35917 = DIRECTION ( 'NONE',  ( 0.5735764363510499342, 0.3127926500124801890, -0.7570804645221008711 ) ) ;
#35918 = CARTESIAN_POINT ( 'NONE',  ( 122.8368814775786291, -1.561330072975668948, -17.79121239304076951 ) ) ;
#35919 = CARTESIAN_POINT ( 'NONE',  ( 114.9970202545248412, 0.1403307496149616695, -11.32035403202665336 ) ) ;
#35920 = CARTESIAN_POINT ( 'NONE',  ( 120.0572748109119772, -6.222761293078241884, -8.102969835052219238 ) ) ;
#35921 = CARTESIAN_POINT ( 'NONE',  ( 123.0070614775786169, -10.15424416112533912, -14.75197769757731336 ) ) ;
#35923 = CARTESIAN_POINT ( 'NONE',  ( 116.0296814775786345, -1.833838273342658809, -17.42832698103878286 ) ) ;
#35922 = AXIS2_PLACEMENT_3D ( 'NONE', #1509, #439, #10938 ) ;
#35924 = CARTESIAN_POINT ( 'NONE',  ( 86.25676480896552789, -26.61243077327098661, -8.441090345486626845 ) ) ;
#35925 = CARTESIAN_POINT ( 'NONE',  ( 106.5237390045248418, 0.8980012041604421569, -15.77991374673208469 ) ) ;
#35926 = CARTESIAN_POINT ( 'NONE',  ( 124.4819548109119722, -2.084020599724406786, -8.691656652584148546 ) ) ;
#35927 = VECTOR ( 'NONE', #10285, 1000.000000000000114 ) ;
#35928 = CARTESIAN_POINT ( 'NONE',  ( 124.0281414775786146, -7.643976991954077427, -18.09477374809248928 ) ) ;
#35929 = FACE_OUTER_BOUND ( 'NONE', #31749, .T. ) ;
#35930 = CARTESIAN_POINT ( 'NONE',  ( 123.3550173109119612, 0.2312338769422704887, -16.08380026872395874 ) ) ;
#35931 = CARTESIAN_POINT ( 'NONE',  ( 116.4555358795247884, -0.7896495226426338832, -17.46756447353520159 ) ) ;
#35932 = DIRECTION ( 'NONE',  ( -0.2588190451025191297, 0.9659258262890686453, 0.000000000000000000 ) ) ;
#35933 = CARTESIAN_POINT ( 'NONE',  ( 116.3166296295247832, -4.863998795839590272, -19.15521520033831493 ) ) ;
#35934 = CARTESIAN_POINT ( 'NONE',  ( 116.6536748109119941, 0.9020085738987339008, -11.91225656197089222 ) ) ;
#35935 = CARTESIAN_POINT ( 'NONE',  ( 120.2274548109119934, 0.5811942927096110934, -14.16772938898807510 ) ) ;
#35936 = DIRECTION ( 'NONE',  ( -1.000000000000000000, 0.000000000000000000, 0.000000000000000000 ) ) ;
#35937 = CARTESIAN_POINT ( 'NONE',  ( 113.4769814775786330, -10.63000616557722466, -14.87417383870573495 ) ) ;
#35938 = DIRECTION ( 'NONE',  ( -0.5040994586965557023, -0.8636456077245108220, 0.000000000000000000 ) ) ;
#35939 = ORIENTED_EDGE ( 'NONE', *, *, #41607, .T. ) ;
#35940 = CARTESIAN_POINT ( 'NONE',  ( 75.95778847736514194, -3.256761025687008537, -10.39321520033831625 ) ) ;
#35941 = EDGE_CURVE ( 'NONE', #30697, #20261, #27253, .T. ) ;
#35942 = CARTESIAN_POINT ( 'NONE',  ( 117.9583881442453048, -10.30919188438810075, -12.61870101168855918 ) ) ;
#35943 = CARTESIAN_POINT ( 'NONE',  ( 121.7590748109119687, -2.084020599724406786, -8.691656652584148546 ) ) ;
#35944 = DIRECTION ( 'NONE',  ( 1.000000000000000000, 0.000000000000000000, 0.000000000000000000 ) ) ;
#35945 = CARTESIAN_POINT ( 'NONE',  ( 113.4769814775786330, 0.4262465694468514643, -12.03445270309931736 ) ) ;
#35946 = CARTESIAN_POINT ( 'NONE',  ( 122.2128881442453263, -1.834011780172310813, -8.268836392978581529 ) ) ;
#35947 = CARTESIAN_POINT ( 'NONE',  ( 113.3995983795247895, -0.7896495226426338832, -9.318865927141430916 ) ) ;
#35948 = CARTESIAN_POINT ( 'NONE',  ( 116.5969481442453031, -9.859900752359374465, -12.68260735090039404 ) ) ;
#35949 = CARTESIAN_POINT ( 'NONE',  ( 120.2296266859119953, -0.06289925094097943703, -9.412459353600674206 ) ) ;
#35950 = CARTESIAN_POINT ( 'NONE',  ( 77.44400397045842510, -3.459648945705700473, -7.147228641687434880 ) ) ;
#35951 = ORIENTED_EDGE ( 'NONE', *, *, #179, .T. ) ;
#35952 = EDGE_CURVE ( 'NONE', #41727, #1522, #14903, .T. ) ;
#35953 = CARTESIAN_POINT ( 'NONE',  ( 123.7717360609119623, -6.564341423271550902, -7.887810678476487425 ) ) ;
#35954 = CARTESIAN_POINT ( 'NONE',  ( 118.2987481442453088, -1.561330072975668504, -17.79121239304076951 ) ) ;
#35955 = ORIENTED_EDGE ( 'NONE', *, *, #14423, .F. ) ;
#35956 = CYLINDRICAL_SURFACE ( 'NONE', #16774, 3.000000000000001776 ) ;
#35957 = CARTESIAN_POINT ( 'NONE',  ( 111.3780948109119890, -5.574606645277172312, -18.38911715685844683 ) ) ;
#35958 = FILL_AREA_STYLE_COLOUR ( '', #4880 ) ;
#35959 = CARTESIAN_POINT ( 'NONE',  ( 115.1787814775786387, -0.1624402480850797581, -16.17319339645315424 ) ) ;
#35960 = CARTESIAN_POINT ( 'NONE',  ( 66.31316073997737703, -0.09061936939670083013, -16.39321520033831447 ) ) ;
#35961 = ADVANCED_FACE ( 'NONE', ( #10150 ), #17574, .T. ) ;
#35962 = CARTESIAN_POINT ( 'NONE',  ( 124.5101297936590754, -9.706096323638551127, -12.14509628965581278 ) ) ;
#35963 = CARTESIAN_POINT ( 'NONE',  ( 122.2128881442453263, -7.643976991954077427, -18.09477374809248928 ) ) ;
#35964 = CARTESIAN_POINT ( 'NONE',  ( 67.84197459855160162, -49.94078482437982558, -33.90832201447402383 ) ) ;
#35965 = CARTESIAN_POINT ( 'NONE',  ( 123.8012348109119642, -9.565557343593413364, -10.61323700422348004 ) ) ;
#35966 = LINE ( 'NONE', #26393, #20162 ) ;
#35967 = CARTESIAN_POINT ( 'NONE',  ( 121.6456214775786293, 0.4262465694468514643, -12.03445270309931736 ) ) ;
#35968 = CARTESIAN_POINT ( 'NONE',  ( 114.2711548109119803, -9.988377603198976828, -10.36322818467138340 ) ) ;
#35969 = CARTESIAN_POINT ( 'NONE',  ( 121.1350814775786233, 0.5811942927096110934, -14.16772938898807510 ) ) ;
#35970 = CARTESIAN_POINT ( 'NONE',  ( 113.8740681442453138, 0.5811942927096154232, -14.16772938898807155 ) ) ;
#35971 = CARTESIAN_POINT ( 'NONE',  ( 135.3184548109119874, -2.475900776146298110, -7.888945235271312306 ) ) ;
#35972 = CARTESIAN_POINT ( 'NONE',  ( 122.2128881442453263, -7.643976991954077427, -18.09477374809248928 ) ) ;
#35973 = VERTEX_POINT ( 'NONE', #7931 ) ;
#35974 = CARTESIAN_POINT ( 'NONE',  ( 120.6812681442452941, -10.30919188438810075, -12.61870101168855918 ) ) ;
#35975 = CARTESIAN_POINT ( 'NONE',  ( 115.3442858795247759, -8.402594152722688392, -9.854619843455216355 ) ) ;
#35976 = DIRECTION ( 'NONE',  ( 0.8636456077245090457, -0.5040994586965586999, 0.000000000000000000 ) ) ;
#35977 = CARTESIAN_POINT ( 'NONE',  ( 113.5337081442453240, -0.8288870151387760510, -10.36305467784173118 ) ) ;
#35978 = CARTESIAN_POINT ( 'NONE',  ( 122.1743141859119817, -8.321307733199551748, -9.223433127585318303 ) ) ;
#35979 = CARTESIAN_POINT ( 'NONE',  ( 115.8304577545247582, -2.791137627527939813, -18.39754474579286025 ) ) ;
#35980 = ORIENTED_EDGE ( 'NONE', *, *, #5532, .T. ) ;
#35981 = CARTESIAN_POINT ( 'NONE',  ( 121.0216281442452981, -7.894159318335828068, -9.358103419637847864 ) ) ;
#35982 = CARTESIAN_POINT ( 'NONE',  ( 121.2019704359119743, 1.345710702986147034, -13.97328579221134426 ) ) ;
#35983 = CARTESIAN_POINT ( 'NONE',  ( 123.0077516859119839, -9.665098340737509730, -17.37397104707595474 ) ) ;
#35984 = LINE ( 'NONE', #886, #8609 ) ;
#35985 = CIRCLE ( 'NONE', #28007, 5.999999999999997335 ) ;
#35986 = CARTESIAN_POINT ( 'NONE',  ( 106.8015515045248378, -6.936859964151250502, -18.39754474579286025 ) ) ;
#35987 = ORIENTED_EDGE ( 'NONE', *, *, #40636, .F. ) ;
#35988 = CARTESIAN_POINT ( 'NONE',  ( 115.9162281442453235, -4.089484607189486809, -7.948022111789456723 ) ) ;
#35989 = LINE ( 'NONE', #14582, #43051 ) ;
#35990 = CARTESIAN_POINT ( 'NONE',  ( 122.4397948109119767, -0.1624402480850797581, -16.17319339645315424 ) ) ;
#35991 = CARTESIAN_POINT ( 'NONE',  ( 112.9097148109120070, -9.565557343593413364, -10.61323700422348004 ) ) ;
#35992 = PRESENTATION_STYLE_ASSIGNMENT (( #39881 ) ) ;
#35993 = CARTESIAN_POINT ( 'NONE',  ( 111.3780948109119890, -5.574606645277164318, -18.38911715685844683 ) ) ;
#35994 = DIRECTION ( 'NONE',  ( -0.7871354856660162103, -0.4483307682966942709, -0.4235767337848251879 ) ) ;
#35995 = DIRECTION ( 'NONE',  ( 0.8636456077245092677, -0.5040994586965584778, 0.000000000000000000 ) ) ;
#35996 = CARTESIAN_POINT ( 'NONE',  ( 111.7751814775786556, -7.893985811506177619, -18.51759400769804742 ) ) ;
#35997 = ORIENTED_EDGE ( 'NONE', *, *, #44845, .F. ) ;
#35998 = EDGE_CURVE ( 'NONE', #29655, #10303, #4493, .T. ) ;
#35999 = CARTESIAN_POINT ( 'NONE',  ( 115.0664733795247798, -1.325403438956436419, -9.854619843455211026 ) ) ;
#36000 = CARTESIAN_POINT ( 'NONE',  ( 119.7169148109119874, -9.988377603198976828, -10.36322818467138340 ) ) ;
#36001 = CARTESIAN_POINT ( 'NONE',  ( 137.2618751061035880, -9.521150726106348827, -15.82766067591523651 ) ) ;
#36002 = ORIENTED_EDGE ( 'NONE', *, *, #30360, .T. ) ;
#36003 =( BOUNDED_CURVE ( )  B_SPLINE_CURVE ( 3, ( #32130, #35084, #35312, #4765 ),
 .UNSPECIFIED., .F., .T. ) 
 B_SPLINE_CURVE_WITH_KNOTS ( ( 4, 4 ),
 ( 1.570796326794899889, 3.141592653589795336 ),
 .UNSPECIFIED. ) 
 CURVE ( )  GEOMETRIC_REPRESENTATION_ITEM ( )  RATIONAL_B_SPLINE_CURVE ( ( 1.000000000000000000, 0.8047378541243659367, 0.8047378541243659367, 1.000000000000000000 ) ) 
 REPRESENTATION_ITEM ( '' )  );
#36004 = CARTESIAN_POINT ( 'NONE',  ( 136.5935259641839252, 0.3896279301912132786, -11.16094382891788861 ) ) ;
#36005 = CARTESIAN_POINT ( 'NONE',  ( 125.3895814775786448, -7.893985811506177619, -18.51759400769804742 ) ) ;
#36006 = CARTESIAN_POINT ( 'NONE',  ( 86.34560043013698305, -9.320000780048239619, -18.64321520033831803 ) ) ;
#36007 = CARTESIAN_POINT ( 'NONE',  ( 124.1415948109119540, -3.505236298600246325, -18.68346056562440793 ) ) ;
#36008 = B_SPLINE_CURVE_WITH_KNOTS ( 'NONE', 3,
 ( #18535, #32647, #11247, #974 ),
 .UNSPECIFIED., .F., .F.,
 ( 4, 4 ),
 ( 0.005429436266171680341, 0.006853839515878830564 ),
 .UNSPECIFIED. ) ;
#36009 = CIRCLE ( 'NONE', #41866, 2.999999999999999556 ) ;
#36010 = ORIENTED_EDGE ( 'NONE', *, *, #3646, .T. ) ;
#36011 = CARTESIAN_POINT ( 'NONE',  ( 119.7736414775786358, -10.30919188438810075, -12.61870101168855918 ) ) ;
#36012 = EDGE_CURVE ( 'NONE', #42758, #36318, #31648, .T. ) ;
#36013 = DIRECTION ( 'NONE',  ( 0.000000000000000000, -0.4669533266896288004, -0.8842819633428518067 ) ) ;
#36014 = CARTESIAN_POINT ( 'NONE',  ( 116.6599933359170507, -2.311015703046737535, -18.04188382666267998 ) ) ;
#36015 = CARTESIAN_POINT ( 'NONE',  ( 124.8603923818566273, -1.444759446862402097, -20.30530361472503387 ) ) ;
#36016 = CARTESIAN_POINT ( 'NONE',  ( 137.4478226697684136, -3.708367563260872579, -8.456766944596608937 ) ) ;
#36017 = VECTOR ( 'NONE', #19774, 1000.000000000000114 ) ;
#36018 = CARTESIAN_POINT ( 'NONE',  ( 112.3424481442453384, -3.505236298600246325, -18.68346056562440793 ) ) ;
#36019 = CARTESIAN_POINT ( 'NONE',  ( 86.84453910206313765, -17.83168818462593919, -19.39321520033831447 ) ) ;
#36020 = DIRECTION ( 'NONE',  ( 0.000000000000000000, 0.000000000000000000, 1.000000000000000000 ) ) ;
#36021 = CARTESIAN_POINT ( 'NONE',  ( 111.5482748109120053, -0.1624402480850797581, -16.17319339645315424 ) ) ;
#36022 = CARTESIAN_POINT ( 'NONE',  ( 125.9568481442452850, -3.505236298600246325, -18.68346056562440793 ) ) ;
#36023 = CARTESIAN_POINT ( 'NONE',  ( 116.6756230178623639, -8.487090413082341911, -16.95583224994113891 ) ) ;
#36024 = CARTESIAN_POINT ( 'NONE',  ( 122.5532481442453019, 0.4262465694468514643, -12.03445270309931736 ) ) ;
#36025 = CARTESIAN_POINT ( 'NONE',  ( 113.4769814775786330, 0.4262465694468514643, -12.03445270309931736 ) ) ;
#36026 = CARTESIAN_POINT ( 'NONE',  ( 120.0005481442453146, -5.638512984488999180, -18.83840828888717311 ) ) ;
#36027 = ORIENTED_EDGE ( 'NONE', *, *, #27184, .T. ) ;
#36028 = CARTESIAN_POINT ( 'NONE',  ( 126.2455040230441341, -8.733555821824001697, -16.58294173486839540 ) ) ;
#36029 = CARTESIAN_POINT ( 'NONE',  ( 114.8581140045248361, -10.62599879583958717, -11.00651665394454604 ) ) ;
#36030 = CARTESIAN_POINT ( 'NONE',  ( 109.0935046295247872, -4.863998795839590272, -18.39754474579285315 ) ) ;
#36031 = CARTESIAN_POINT ( 'NONE',  ( 110.0658483795247804, -8.402594152722688392, -16.93181055722141792 ) ) ;
#36032 = CARTESIAN_POINT ( 'NONE',  ( 125.2761281442453338, 0.4262465694465857324, -12.03445270309828175 ) ) ;
#36033 = CARTESIAN_POINT ( 'NONE',  ( 115.9729548109119861, -6.344957434206662583, -7.627207830600332805 ) ) ;
#36034 = VERTEX_POINT ( 'NONE', #15113 ) ;
#36035 = CARTESIAN_POINT ( 'NONE',  ( 115.2355081442453155, 0.1319031606808879209, -14.10382304977623669 ) ) ;
#36036 = CARTESIAN_POINT ( 'NONE',  ( 108.7462390045248242, 0.8980012041604421569, -15.77991374673208469 ) ) ;
#36037 = DIRECTION ( 'NONE',  ( -0.2768435750659239414, -0.3568721902840664151, 0.8921882507333142032 ) ) ;
#36038 = CARTESIAN_POINT ( 'NONE',  ( 126.2404814775786264, -9.261995988541697145, -16.69588392320189030 ) ) ;
#36039 = FACE_OUTER_BOUND ( 'NONE', #7302, .T. ) ;
#36040 = CARTESIAN_POINT ( 'NONE',  ( -13.49987324484352769, -3.923910153600668860, -18.82182469926544854 ) ) ;
#36041 = CARTESIAN_POINT ( 'NONE',  ( 115.4056881442453459, -7.893985811506177619, -18.51759400769804742 ) ) ;
#36042 = CARTESIAN_POINT ( 'NONE',  ( 110.3436608795247764, -8.938348069036489818, -9.318865927141430916 ) ) ;
#36043 = CARTESIAN_POINT ( 'NONE',  ( 110.6909265045248247, -2.791137627527939813, -8.388885654883777576 ) ) ;
#36044 = AXIS2_PLACEMENT_3D ( 'NONE', #27853, #16698, #41763 ) ;
#36045 = ORIENTED_EDGE ( 'NONE', *, *, #20015, .F. ) ;
#36046 = CARTESIAN_POINT ( 'NONE',  ( 128.2184548109119930, -7.067465109756605912, -7.812468278694988832 ) ) ;
#36047 = CARTESIAN_POINT ( 'NONE',  ( 119.4900081442453086, -7.643976991954077427, -18.09477374809248928 ) ) ;
#36048 = CARTESIAN_POINT ( 'NONE',  ( 114.6682414775786469, -1.561330072975668060, -17.79121239304076596 ) ) ;
#36049 = CARTESIAN_POINT ( 'NONE',  ( 113.4202548109119846, -10.30919188438810075, -12.61870101168855918 ) ) ;
#36050 = CARTESIAN_POINT ( 'NONE',  ( 125.6732148109119862, -9.859900752359378018, -12.68260735090039759 ) ) ;
#36051 = PRODUCT_DEFINITION_CONTEXT ( 'detailed design', #11383, 'design' ) ;
#36052 = CARTESIAN_POINT ( 'NONE',  ( 123.5176014775786228, -0.8288870151387760510, -10.36305467784173118 ) ) ;
#36053 = CARTESIAN_POINT ( 'NONE',  ( 114.7249681442453237, -9.565557343593413364, -10.61323700422348004 ) ) ;
#36054 = ORIENTED_EDGE ( 'NONE', *, *, #27569, .F. ) ;
#36055 = CARTESIAN_POINT ( 'NONE',  ( 120.2990798109119766, -2.173413727453600508, -8.297982527556802879 ) ) ;
#36056 = CARTESIAN_POINT ( 'NONE',  ( 70.19189222814998175, -57.05206236706784040, -36.02363522683400276 ) ) ;
#36057 = CARTESIAN_POINT ( 'NONE',  ( 117.1074881442453233, 0.4262465694468514643, -12.03445270309931736 ) ) ;
#36058 = EDGE_LOOP ( 'NONE', ( #23278, #5280, #128, #33769, #16573, #27555 ) ) ;
#36059 = FACE_OUTER_BOUND ( 'NONE', #9967, .T. ) ;
#36060 = CARTESIAN_POINT ( 'NONE',  ( 116.0296814775786345, -8.166667518702817929, -8.995218007635861213 ) ) ;
#36061 = CARTESIAN_POINT ( 'NONE',  ( 107.1488171295247867, 0.1403307496149613920, -13.39321520033831447 ) ) ;
#36062 = CARTESIAN_POINT ( 'NONE',  ( 112.9097148109120070, -9.565557343593413364, -10.61323700422348004 ) ) ;
#36063 = EDGE_LOOP ( 'NONE', ( #30864, #34077, #34439, #5206 ) ) ;
#36064 = VERTEX_POINT ( 'NONE', #4838 ) ;
#36065 = CARTESIAN_POINT ( 'NONE',  ( 121.3619881442452879, -5.574606645277164318, -18.38911715685844683 ) ) ;
#36066 = EDGE_CURVE ( 'NONE', #3495, #32667, #36008, .T. ) ;
#36067 = CARTESIAN_POINT ( 'NONE',  ( 118.9227414775786542, 0.4262465694468514643, -12.03445270309931736 ) ) ;
#36068 = CARTESIAN_POINT ( 'NONE',  ( 124.5423633126549561, -9.852374207079853008, -13.03727910468368201 ) ) ;
#36069 = CARTESIAN_POINT ( 'NONE',  ( 116.7104014775786425, -8.899110576539721151, -16.42337572283488711 ) ) ;
#36070 = ORIENTED_EDGE ( 'NONE', *, *, #35952, .T. ) ;
#36071 = CARTESIAN_POINT ( 'NONE',  ( 128.2184548109119930, -4.863998795839242995, -13.39321520033831447 ) ) ;
#36072 = CARTESIAN_POINT ( 'NONE',  ( 71.77086717554882966, -26.54201219542348511, -4.893215200338314474 ) ) ;
#36073 = AXIS2_PLACEMENT_3D ( 'NONE', #9863, #10311, #24427 ) ;
#36074 = CARTESIAN_POINT ( 'NONE',  ( 110.3436608795247764, -8.938348069036489818, -9.318865927141430916 ) ) ;
#36075 = CARTESIAN_POINT ( 'NONE',  ( 114.8951481442453115, -0.4660016031367893996, -10.09054647747474043 ) ) ;
#36077 = CARTESIAN_POINT ( 'NONE',  ( 114.4413348109119823, -0.8288870151387760510, -10.36305467784173118 ) ) ;
#36076 = CARTESIAN_POINT ( 'NONE',  ( 112.5126281442453120, -10.30919188438810075, -12.61870101168855918 ) ) ;
#36078 = CARTESIAN_POINT ( 'NONE',  ( 121.9292548109119849, -7.894159318335828068, -9.358103419637847864 ) ) ;
#36079 = CYLINDRICAL_SURFACE ( 'NONE', #35655, 2.999999999999996003 ) ;
#36080 = ORIENTED_EDGE ( 'NONE', *, *, #3335, .F. ) ;
#36081 = CONICAL_SURFACE ( 'NONE', #12810, 2.445500000000004448, 0.9599310885968757034 ) ;
#36082 = CARTESIAN_POINT ( 'NONE',  ( 120.7379948109119709, 0.4262465694468514643, -12.03445270309931736 ) ) ;
#36083 = CARTESIAN_POINT ( 'NONE',  ( 124.3117748109119844, 0.1319031606808879209, -14.10382304977623669 ) ) ;
#36084 = CARTESIAN_POINT ( 'NONE',  ( 67.69189222814998175, -42.70034233532976486, -10.06214201013430909 ) ) ;
#36085 = CARTESIAN_POINT ( 'NONE',  ( 117.8239502440515452, -2.467220198592778413, -17.83387418641524391 ) ) ;
#36086 = CARTESIAN_POINT ( 'NONE',  ( 114.1635827545248389, -2.477300249445798297, -19.15521520033831138 ) ) ;
#36087 = CARTESIAN_POINT ( 'NONE',  ( 117.7314814775786260, -4.089484607189486809, -7.948022111789456723 ) ) ;
#36088 = ORIENTED_EDGE ( 'NONE', *, *, #20436, .T. ) ;
#36089 = CARTESIAN_POINT ( 'NONE',  ( 117.8449348109119938, -8.166667518702817929, -8.995218007635861213 ) ) ;
#36090 = CARTESIAN_POINT ( 'NONE',  ( 115.2974471540078554, -2.348512537728063787, -17.99195118506216318 ) ) ;
#36091 = CARTESIAN_POINT ( 'NONE',  ( 109.2324108795247923, -8.938348069036489818, -9.318865927141430916 ) ) ;
#36092 = CARTESIAN_POINT ( 'NONE',  ( 116.1431348109119881, -10.30919188438810075, -12.61870101168855918 ) ) ;
#36093 = CARTESIAN_POINT ( 'NONE',  ( 117.7882081442453170, -6.344957434206665248, -7.627207830600338134 ) ) ;
#36094 = CARTESIAN_POINT ( 'NONE',  ( 126.9115046738313879, -10.20580091807491030, -13.62532772550883919 ) ) ;
#36095 = CARTESIAN_POINT ( 'NONE',  ( 117.1405054202893155, -11.23569791401464713, -5.537001952796093640 ) ) ;
#36096 = CARTESIAN_POINT ( 'NONE',  ( 105.8292077545248446, -2.791137627527939813, -18.39754474579286025 ) ) ;
#36097 = ORIENTED_EDGE ( 'NONE', *, *, #36154, .F. ) ;
#36098 = CARTESIAN_POINT ( 'NONE',  ( 112.4201593777725208, -1.267766418764741276, -16.93314635290707315 ) ) ;
#36099 = CARTESIAN_POINT ( 'NONE',  ( 109.2294691412240297, -9.956217823165619762, -15.41276842522689350 ) ) ;
#36100 = CARTESIAN_POINT ( 'NONE',  ( 119.7736414775786358, 0.1319031606808879209, -14.10382304977623669 ) ) ;
#36101 = CIRCLE ( 'NONE', #16466, 35.00000000000000000 ) ;
#36102 = CARTESIAN_POINT ( 'NONE',  ( 114.0941296295247867, -4.863998795839590272, -8.388885654883775800 ) ) ;
#36103 = CARTESIAN_POINT ( 'NONE',  ( 114.9970202545248412, 0.1403307496149616695, -11.32035403202665336 ) ) ;
#36104 = CARTESIAN_POINT ( 'NONE',  ( 114.7816948109119863, -9.859900752359374465, -12.68260735090039404 ) ) ;
#36105 = CARTESIAN_POINT ( 'NONE',  ( 0.04488520489200759078, -6.166763362545027327, -19.39321520033831447 ) ) ;
#36106 = CARTESIAN_POINT ( 'NONE',  ( 112.2289948109119848, -7.643976991954077427, -18.09477374809248928 ) ) ;
#36107 = CARTESIAN_POINT ( 'NONE',  ( 118.8660148109119774, -10.30919188438810075, -12.61870101168855918 ) ) ;
#36108 = ORIENTED_EDGE ( 'NONE', *, *, #7185, .T. ) ;
#36109 = VECTOR ( 'NONE', #39225, 1000.000000000000000 ) ;
#36110 = CARTESIAN_POINT ( 'NONE',  ( 118.1285681442453068, -2.084020599724406786, -8.691656652584148546 ) ) ;
#36111 = CARTESIAN_POINT ( 'NONE',  ( 114.8951481442453115, -0.4660016031367893996, -10.09054647747474043 ) ) ;
#36112 = CARTESIAN_POINT ( 'NONE',  ( 121.7023481442452777, -9.261995988541697145, -16.69588392320189030 ) ) ;
#36113 = CARTESIAN_POINT ( 'NONE',  ( 120.2274548109119934, -9.859900752359378018, -12.68260735090039759 ) ) ;
#36114 = ORIENTED_EDGE ( 'NONE', *, *, #33249, .F. ) ;
#36115 = CARTESIAN_POINT ( 'NONE',  ( 124.7088614775786226, -9.565557343593413364, -10.61323700422348004 ) ) ;
#36116 = CIRCLE ( 'NONE', #1907, 2.999999999999998224 ) ;
#36117 = CARTESIAN_POINT ( 'NONE',  ( 122.0427081442452817, 0.5811942927096110934, -14.16772938898807510 ) ) ;
#36118 = CARTESIAN_POINT ( 'NONE',  ( 124.9009360172555034, -8.233366253754685005, -6.504877232558810896 ) ) ;
#36119 = CARTESIAN_POINT ( 'NONE',  ( 63.28220228971554207, -14.74607418325012098, -9.753631345296810196 ) ) ;
#36120 = CARTESIAN_POINT ( 'NONE',  ( 138.1238347578285754, -2.002283765726665887, -15.95502668635790222 ) ) ;
#36121 = ADVANCED_FACE ( 'NONE', ( #18307 ), #25155, .T. ) ;
#36122 = CARTESIAN_POINT ( 'NONE',  ( 115.7610046295247912, -4.863998795839590272, -18.39754474579285315 ) ) ;
#36123 = DIRECTION ( 'NONE',  ( -0.000000000000000000, -0.9284778069183721172, -0.3713878862591650232 ) ) ;
#36124 = LINE ( 'NONE', #4893, #3318 ) ;
#36125 = CARTESIAN_POINT ( 'NONE',  ( 115.5758681442453053, -7.894159318335828068, -9.358103419637847864 ) ) ;
#36126 = CARTESIAN_POINT ( 'NONE',  ( 124.4819548109119722, -7.893985811506177619, -18.51759400769804742 ) ) ;
#36127 = CARTESIAN_POINT ( 'NONE',  ( 64.28447634061448923, -12.99130359988381755, -15.72333420167097096 ) ) ;
#36128 = CARTESIAN_POINT ( 'NONE',  ( 117.0143358795247792, -1.328464889906837199, -16.92874910627105223 ) ) ;
#36129 = CARTESIAN_POINT ( 'NONE',  ( 110.8298327545248299, -6.936859964151250502, -8.388885654883777576 ) ) ;
#36130 = CARTESIAN_POINT ( 'NONE',  ( 116.7671281442453335, -7.643976991954077427, -18.09477374809248928 ) ) ;
#36131 = CARTESIAN_POINT ( 'NONE',  ( 113.4429142554890859, -2.372251574601226043, -17.96033910819752322 ) ) ;
#36132 = ADVANCED_FACE ( 'NONE', ( #42038 ), #36725, .T. ) ;
#36133 = AXIS2_PLACEMENT_3D ( 'NONE', #21792, #10643, #6995 ) ;
#36134 = DIRECTION ( 'NONE',  ( -0.1352586133457952255, -0.9908103287288504424, 0.000000000000000000 ) ) ;
#36136 = CARTESIAN_POINT ( 'NONE',  ( 118.4689281442453392, 0.9020085738987339008, -11.91225656197089222 ) ) ;
#36135 = CARTESIAN_POINT ( 'NONE',  ( 66.40653143407884329, -14.77812736305742547, -10.49134286602717658 ) ) ;
#36137 = CARTESIAN_POINT ( 'NONE',  ( 122.3830681442452857, -1.833838273342659697, -17.42832698103878286 ) ) ;
#36138 = ORIENTED_EDGE ( 'NONE', *, *, #27340, .T. ) ;
#36139 = CARTESIAN_POINT ( 'NONE',  ( 137.0105207745575342, -8.969470875690532807, -9.795839679219671581 ) ) ;
#36140 = CARTESIAN_POINT ( 'NONE',  ( 125.6164881442453094, 0.2603800115204892296, -16.42320221600525088 ) ) ;
#36141 = CARTESIAN_POINT ( 'NONE',  ( 108.8156921295247912, -9.868328341294093420, -13.39321520033831447 ) ) ;
#36142 = CARTESIAN_POINT ( 'NONE',  ( 120.9081748109119872, -4.153390946401325223, -8.397313243818185668 ) ) ;
#36143 = CARTESIAN_POINT ( 'NONE',  ( 120.3409081442453044, -8.899110576539710493, -16.42337572283490132 ) ) ;
#36144 = CIRCLE ( 'NONE', #7778, 1.610000000000000986 ) ;
#36145 = CARTESIAN_POINT ( 'NONE',  ( 117.1642148109119859, -0.8288870151387760510, -10.36305467784173118 ) ) ;
#36146 = CARTESIAN_POINT ( 'NONE',  ( 125.3563494635813242, 1.483268859736976308, -16.45799053132973455 ) ) ;
#36147 = CARTESIAN_POINT ( 'NONE',  ( 106.8710046295248759, -4.863998795839590272, -7.631215200338315796 ) ) ;
#36148 = CARTESIAN_POINT ( 'NONE',  ( 122.8368814775786291, -7.894159318335828068, -9.358103419637847864 ) ) ;
#36149 = CARTESIAN_POINT ( 'NONE',  ( 125.2194014775786286, 0.1319031606808879209, -14.10382304977623669 ) ) ;
#36150 = DIRECTION ( 'NONE',  ( 0.000000000000000000, 0.000000000000000000, 1.000000000000000000 ) ) ;
#36151 = CARTESIAN_POINT ( 'NONE',  ( -13.52873657336266078, -4.831135987035605872, -8.722383338069434444 ) ) ;
#36152 = CARTESIAN_POINT ( 'NONE',  ( 119.4656423109119743, -0.4387604401700512802, -15.73000352943951619 ) ) ;
#36153 = CARTESIAN_POINT ( 'NONE',  ( 116.3860827545247787, -2.477300249445798297, -19.15521520033831138 ) ) ;
#36154 = EDGE_CURVE ( 'NONE', #37642, #10139, #24923, .T. ) ;
#36155 = FACE_OUTER_BOUND ( 'NONE', #26931, .T. ) ;
#36156 = CARTESIAN_POINT ( 'NONE',  ( 122.6099748109119929, -9.261995988541697145, -16.69588392320189030 ) ) ;
#36157 = CARTESIAN_POINT ( 'NONE',  ( 118.4122014775786340, 0.5811942927096110934, -14.16772938898807510 ) ) ;
#36158 = CARTESIAN_POINT ( 'NONE',  ( 106.8710046295248759, -4.863998795839590272, -7.631215200338315796 ) ) ;
#36159 = CARTESIAN_POINT ( 'NONE',  ( 113.2500748109119968, -6.344957434206662583, -7.627207830600332805 ) ) ;
#36160 = EDGE_CURVE ( 'NONE', #26749, #873, #39643, .T. ) ;
#36161 = EDGE_CURVE ( 'NONE', #13861, #6063, #22619, .T. ) ;
#36162 = LINE ( 'NONE', #25916, #27950 ) ;
#36163 = ORIENTED_EDGE ( 'NONE', *, *, #6936, .T. ) ;
#36164 = CARTESIAN_POINT ( 'NONE',  ( 69.36136150295220659, -60.90811235867516160, -34.46123413341155839 ) ) ;
#36165 = CARTESIAN_POINT ( 'NONE',  ( 118.3554748109119998, 0.2603800115204892296, -16.42320221600525088 ) ) ;
#36166 = CARTESIAN_POINT ( 'NONE',  ( 126.0135748109119902, -1.833838273342660141, -17.42832698103878286 ) ) ;
#36167 = VECTOR ( 'NONE', #13914, 1000.000000000000000 ) ;
#36168 = DIRECTION ( 'NONE',  ( 1.000000000000000000, 0.000000000000000000, 0.000000000000000000 ) ) ;
#36169 = CARTESIAN_POINT ( 'NONE',  ( 115.4624148109119943, -4.153390946401321671, -8.397313243818183892 ) ) ;
#36170 = CARTESIAN_POINT ( 'NONE',  ( 125.4463081442452932, -5.638512984488999180, -18.83840828888717311 ) ) ;
#36171 = AXIS2_PLACEMENT_3D ( 'NONE', #44325, #26532, #40442 ) ;
#36172 = CARTESIAN_POINT ( 'NONE',  ( 111.5243640045248412, -10.62599879583958717, -11.00651665394454604 ) ) ;
#36173 = CARTESIAN_POINT ( 'NONE',  ( 120.7379948109119709, 0.4262465694468514643, -12.03445270309931736 ) ) ;
#36174 = CARTESIAN_POINT ( 'NONE',  ( 110.8992858795247827, -0.7896495226426338832, -17.46756447353518382 ) ) ;
#36175 = FACE_OUTER_BOUND ( 'NONE', #21964, .T. ) ;
#36176 = VERTEX_POINT ( 'NONE', #22398 ) ;
#36177 = AXIS2_PLACEMENT_3D ( 'NONE', #37539, #2428, #23194 ) ;
#36178 = CARTESIAN_POINT ( 'NONE',  ( 123.7022829359119811, -4.283928203966213211, -7.183505701512925334 ) ) ;
#36179 = CARTESIAN_POINT ( 'NONE',  ( 118.6391081442452986, -4.089484607189486809, -7.948022111789456723 ) ) ;
#36180 = EDGE_CURVE ( 'NONE', #14958, #20548, #29243, .T. ) ;
#36181 = VERTEX_POINT ( 'NONE', #32866 ) ;
#36182 = CARTESIAN_POINT ( 'NONE',  ( 122.0046199480702569, -6.365377317481695663, -18.95617363400926081 ) ) ;
#36183 = CARTESIAN_POINT ( 'NONE',  ( -13.82468485392153568, -4.441611705562402257, -8.282184520274741502 ) ) ;
#36184 = CARTESIAN_POINT ( 'NONE',  ( 115.4328884760651874, 0.6362173239733635022, -12.14321520033831625 ) ) ;
#36185 = CARTESIAN_POINT ( 'NONE',  ( 118.3554748109119998, -9.565557343593413364, -10.61323700422348004 ) ) ;
#36186 = CYLINDRICAL_SURFACE ( 'NONE', #23707, 1.000000000000000888 ) ;
#36187 = CARTESIAN_POINT ( 'NONE',  ( 64.59495755916755400, -36.13370383219653803, -5.723731037142725242 ) ) ;
#36188 = CARTESIAN_POINT ( 'NONE',  ( 124.6521348109119884, -7.894159318335828068, -9.358103419637847864 ) ) ;
#36189 = MANIFOLD_SOLID_BREP ( 'NONE', #39616 ) ;
#36190 = DIRECTION ( 'NONE',  ( 1.000000000000000000, 0.000000000000000000, -0.000000000000000000 ) ) ;
#36191 = DIRECTION ( 'NONE',  ( 0.000000000000000000, 0.3713878862591638574, -0.9284778069183724503 ) ) ;
#36192 = EDGE_CURVE ( 'NONE', #5874, #11018, #84, .T. ) ;
#36193 = CARTESIAN_POINT ( 'NONE',  ( 125.0874013446012469, -12.26524233522089880, -14.59144684667939629 ) ) ;
#36194 = AXIS2_PLACEMENT_3D ( 'NONE', #14775, #18646, #42820 ) ;
#36195 = CARTESIAN_POINT ( 'NONE',  ( 116.3700414775786527, -4.153390946401321671, -8.397313243818183892 ) ) ;
#36196 = CARTESIAN_POINT ( 'NONE',  ( 124.6521348109119884, -7.894159318335828068, -9.358103419637847864 ) ) ;
#36197 = CARTESIAN_POINT ( 'NONE',  ( 112.5693548109119888, -10.63000616557722466, -14.87417383870573495 ) ) ;
#36198 = CARTESIAN_POINT ( 'NONE',  ( 119.9438214775786378, -7.893985811506177619, -18.51759400769804742 ) ) ;
#36199 = CARTESIAN_POINT ( 'NONE',  ( 117.1074881442453233, -10.63000616557722466, -14.87417383870573495 ) ) ;
#36200 = CARTESIAN_POINT ( 'NONE',  ( 116.8722546295247895, -4.863998795839590272, -18.39754474579285315 ) ) ;
#36201 = CARTESIAN_POINT ( 'NONE',  ( 123.0070614775786169, -10.15424416112533912, -14.75197769757731336 ) ) ;
#36202 = EDGE_LOOP ( 'NONE', ( #29475, #17238, #6667, #8040 ) ) ;
#36203 = CARTESIAN_POINT ( 'NONE',  ( 121.0216281442452981, -1.561330072975668948, -17.79121239304076951 ) ) ;
#36204 = CARTESIAN_POINT ( 'NONE',  ( 113.1912390045248031, 0.8980012041604421569, -15.77991374673208469 ) ) ;
#36205 = CARTESIAN_POINT ( 'NONE',  ( 112.7050671295247923, 0.1403307496149613920, -13.39321520033831447 ) ) ;
#36206 = DIRECTION ( 'NONE',  ( 1.000000000000000000, 0.000000000000000000, -0.000000000000000000 ) ) ;
#36207 = DIRECTION ( 'NONE',  ( -0.000000000000000000, -0.9284778069183721172, -0.3713878862591650232 ) ) ;
#36208 = CARTESIAN_POINT ( 'NONE',  ( 120.0212673109119805, 0.2312338769422704887, -16.08380026872395874 ) ) ;
#36209 = CARTESIAN_POINT ( 'NONE',  ( 124.4252281442452812, -9.261995988541697145, -16.69588392320189030 ) ) ;
#36210 = ORIENTED_EDGE ( 'NONE', *, *, #34328, .T. ) ;
#36211 = CARTESIAN_POINT ( 'NONE',  ( 122.4965214775786251, 0.1319031606808879209, -14.10382304977623669 ) ) ;
#36212 = DIRECTION ( 'NONE',  ( 0.9609149988134837450, -0.1028163501681639419, 0.2570431154366518145 ) ) ;
#36213 = CARTESIAN_POINT ( 'NONE',  ( 123.8411891859119862, -8.844754642576884152, -8.592115655440050404 ) ) ;
#36214 = ADVANCED_FACE ( 'NONE', ( #12828 ), #2087, .T. ) ;
#36215 = AXIS2_PLACEMENT_3D ( 'NONE', #14058, #27975, #41880 ) ;
#36216 = CARTESIAN_POINT ( 'NONE',  ( 111.8991748109119868, -7.866424907533402511, -9.395035934245173692 ) ) ;
#36217 = CARTESIAN_POINT ( 'NONE',  ( 109.8574890045248509, -9.868328341294098749, -11.32035403202665869 ) ) ;
#36218 = EDGE_LOOP ( 'NONE', ( #17035, #29108, #12674, #37661, #25182 ) ) ;
#36219 = CARTESIAN_POINT ( 'NONE',  ( 114.8951481442453115, -0.4660016031367893996, -10.09054647747474043 ) ) ;
#36220 = CARTESIAN_POINT ( 'NONE',  ( 88.72832861070837396, -11.14280042575103558, -14.10090787152131320 ) ) ;
#36221 = CARTESIAN_POINT ( 'NONE',  ( 121.0783548109119749, -9.565557343593413364, -10.61323700422348004 ) ) ;
#36222 = CARTESIAN_POINT ( 'NONE',  ( 113.4202548109119846, 0.1319031606808879209, -14.10382304977623669 ) ) ;
#36223 = CARTESIAN_POINT ( 'NONE',  ( 96.46827370896536991, -25.99489077589524300, -13.39321520033831447 ) ) ;
#36224 = EDGE_CURVE ( 'NONE', #16401, #33252, #23303, .T. ) ;
#36225 = DIRECTION ( 'NONE',  ( -1.000000000000000000, 0.000000000000000000, 0.000000000000000000 ) ) ;
#36226 = ORIENTED_EDGE ( 'NONE', *, *, #25199, .F. ) ;
#36227 = CARTESIAN_POINT ( 'NONE',  ( 114.3719421295247827, -9.868328341294093420, -13.39321520033831447 ) ) ;
#36228 = CIRCLE ( 'NONE', #7829, 4.999999999999998224 ) ;
#36229 = CARTESIAN_POINT ( 'NONE',  ( 120.0572748109119772, -3.383040157471821630, -19.15922257007629170 ) ) ;
#36230 = CARTESIAN_POINT ( 'NONE',  ( 137.2352176311256073, -8.497078852651583247, -17.21982894588502333 ) ) ;
#36231 = ORIENTED_EDGE ( 'NONE', *, *, #31486, .T. ) ;
#36232 = CARTESIAN_POINT ( 'NONE',  ( 113.8173414775786512, 0.2603800115204892296, -16.42320221600525088 ) ) ;
#36233 = CARTESIAN_POINT ( 'NONE',  ( 126.0135748109119902, -8.166667518702819706, -8.995218007635861213 ) ) ;
#36234 = CARTESIAN_POINT ( 'NONE',  ( 111.1770983795247787, -8.402594152722633325, -16.93181055722145345 ) ) ;
#36235 = CARTESIAN_POINT ( 'NONE',  ( 124.4819548109119722, -2.084020599724406786, -8.691656652584148546 ) ) ;
#36236 = ORIENTED_EDGE ( 'NONE', *, *, #20863, .T. ) ;
#36237 = CARTESIAN_POINT ( 'NONE',  ( 119.3198281442452924, 0.5811942927096110934, -14.16772938898807510 ) ) ;
#36238 = CARTESIAN_POINT ( 'NONE',  ( 59.77100663911058120, -14.81899367705580595, -8.593215200338313764 ) ) ;
#36239 = CARTESIAN_POINT ( 'NONE',  ( 110.1353015045248185, -6.936859964151197211, -18.39754474579288512 ) ) ;
#36240 = CARTESIAN_POINT ( 'NONE',  ( 114.9740004229301888, 0.1075849324168598464, -14.64321520033831447 ) ) ;
#36241 = CARTESIAN_POINT ( 'NONE',  ( 111.4281736080169054, -2.492852297122321037, -17.79974121491989436 ) ) ;
#36242 = CARTESIAN_POINT ( 'NONE',  ( 114.5547881442453217, -4.153390946401321671, -8.397313243818183892 ) ) ;
#36243 = CARTESIAN_POINT ( 'NONE',  ( 96.54708369096698561, -27.29184247633061489, -11.60278472507885894 ) ) ;
#36244 = CARTESIAN_POINT ( 'NONE',  ( 125.3334400860417759, -2.410057117798671822, -20.05515415193855944 ) ) ;
#36245 = CARTESIAN_POINT ( 'NONE',  ( 126.1837548109119211, -10.63000616557722466, -14.87417383870573495 ) ) ;
#36246 = CARTESIAN_POINT ( 'NONE',  ( 112.7395348109119766, -5.638512984488999180, -18.83840828888717311 ) ) ;
#36247 = CARTESIAN_POINT ( 'NONE',  ( 121.0630641859119976, -8.321307733199551748, -9.223433127585318303 ) ) ;
#36248 = CARTESIAN_POINT ( 'NONE',  ( 123.2906948109119867, -1.833838273342659697, -17.42832698103878286 ) ) ;
#36249 = DIRECTION ( 'NONE',  ( -0.3445294493088598697, -0.9387755102040815647, 0.000000000000000000 ) ) ;
#36250 = CARTESIAN_POINT ( 'NONE',  ( 119.3198281442452924, 0.5811942927096110934, -14.16772938898807510 ) ) ;
#36251 = ADVANCED_FACE ( 'NONE', ( #8715, #26726 ), #1857, .T. ) ;
#36252 = CARTESIAN_POINT ( 'NONE',  ( 120.6245414775786458, -9.988377603198976828, -10.36322818467138340 ) ) ;
#36253 = ORIENTED_EDGE ( 'NONE', *, *, #13141, .F. ) ;
#36254 = DIRECTION ( 'NONE',  ( 0.000000000000000000, 0.000000000000000000, -1.000000000000000000 ) ) ;
#36255 = CARTESIAN_POINT ( 'NONE',  ( 116.4555358795247884, -0.7896495226426338832, -17.46756447353520159 ) ) ;
#36256 = CARTESIAN_POINT ( 'NONE',  ( 108.3989733795248753, -1.325403438956436419, -9.854619843455211026 ) ) ;
#36257 = CARTESIAN_POINT ( 'NONE',  ( 111.0381921295247878, -9.868328341294093420, -13.39321520033831447 ) ) ;
#36258 = AXIS2_PLACEMENT_3D ( 'NONE', #1113, #3852, #17997 ) ;
#36259 = CARTESIAN_POINT ( 'NONE',  ( 135.3184548109119874, -8.536181032868617180, -18.13822074491315561 ) ) ;
#36260 = CARTESIAN_POINT ( 'NONE',  ( 114.2711548109119803, -9.988377603198976828, -10.36322818467138340 ) ) ;
#36261 = VERTEX_POINT ( 'NONE', #19207 ) ;
#36262 = CARTESIAN_POINT ( 'NONE',  ( 106.7320983795247855, -0.7896495226426338832, -9.318865927141430916 ) ) ;
#36263 = DIRECTION ( 'NONE',  ( -0.000000000000000000, -0.9284778069183721172, -0.3713878862591650232 ) ) ;
#36264 = CARTESIAN_POINT ( 'NONE',  ( 75.63675420052337017, -42.57465691284114939, -15.89321520033831447 ) ) ;
#36265 = CARTESIAN_POINT ( 'NONE',  ( 109.2295757755578762, -0.1086748408276279887, -15.25738775639926992 ) ) ;
#36266 = CARTESIAN_POINT ( 'NONE',  ( 112.6260814775786514, -9.261995988541697145, -16.69588392320189030 ) ) ;
#36267 = CARTESIAN_POINT ( 'NONE',  ( 119.4332814775786318, -0.4660016031367893996, -10.09054647747474043 ) ) ;
#36268 = CARTESIAN_POINT ( 'NONE',  ( 109.6491296295247793, -4.863998795839590272, -19.15521520033831493 ) ) ;
#36269 = CARTESIAN_POINT ( 'NONE',  ( 112.3578015045248861, -6.936859964151250502, -18.39754474579286025 ) ) ;
#36270 = ORIENTED_EDGE ( 'NONE', *, *, #15945, .F. ) ;
#36271 = CARTESIAN_POINT ( 'NONE',  ( 110.9518144685027750, 0.6938714319018670640, -14.64321520033828072 ) ) ;
#36272 = CARTESIAN_POINT ( 'NONE',  ( 119.1496481442453046, -6.222761293078241884, -8.102969835052219238 ) ) ;
#36273 = CARTESIAN_POINT ( 'NONE',  ( 116.4834948109119779, -1.561330072975668504, -17.79121239304076951 ) ) ;
#36274 = CARTESIAN_POINT ( 'NONE',  ( 112.0020881442453344, 0.2603800115204892296, -16.42320221600525088 ) ) ;
#36275 = CARTESIAN_POINT ( 'NONE',  ( 123.6877814775786533, -6.222761293078241884, -8.102969835052219238 ) ) ;
#36276 =( BOUNDED_CURVE ( )  B_SPLINE_CURVE ( 3, ( #8408, #25960, #879, #4749 ),
 .UNSPECIFIED., .F., .T. ) 
 B_SPLINE_CURVE_WITH_KNOTS ( ( 4, 4 ),
 ( 3.141592653589785122, 4.712388980384700332 ),
 .UNSPECIFIED. ) 
 CURVE ( )  GEOMETRIC_REPRESENTATION_ITEM ( )  RATIONAL_B_SPLINE_CURVE ( ( 1.000000000000000000, 0.8047378541243619399, 0.8047378541243619399, 1.000000000000000000 ) ) 
 REPRESENTATION_ITEM ( '' )  );
#36277 = CARTESIAN_POINT ( 'NONE',  ( 122.9503348109119827, -9.859900752359378018, -12.68260735090039759 ) ) ;
#36278 = CARTESIAN_POINT ( 'NONE',  ( 114.0442481442453300, -7.643976991954077427, -18.09477374809248928 ) ) ;
#36279 = VERTEX_POINT ( 'NONE', #40635 ) ;
#36280 = CARTESIAN_POINT ( 'NONE',  ( 123.3550173109119612, -9.289237151508434209, -11.05642687123711276 ) ) ;
#36281 = CARTESIAN_POINT ( 'NONE',  ( 113.5348452706805915, 0.3193521225029610777, -14.64321520033833401 ) ) ;
#36282 = CARTESIAN_POINT ( 'NONE',  ( 117.8449348109119938, -1.833838273342659253, -17.42832698103878286 ) ) ;
#36283 = ORIENTED_EDGE ( 'NONE', *, *, #16530, .F. ) ;
#36284 = CARTESIAN_POINT ( 'NONE',  ( 83.32100367795761997, -14.50187442639529323, -9.893215200338316251 ) ) ;
#36285 = B_SPLINE_CURVE_WITH_KNOTS ( 'NONE', 3,
 ( #19359, #39660, #29844, #40566, #43761, #1345, #12527, #9099, #8422, #22328 ),
 .UNSPECIFIED., .F., .F.,
 ( 4, 3, 3, 4 ),
 ( 0.000000000000000000, 0.0001671877560958109985, 0.0003343755126086574896, 0.0006438490228507209303 ),
 .UNSPECIFIED. ) ;
#36286 = CARTESIAN_POINT ( 'NONE',  ( 115.4624148109119943, -5.638512984488999180, -18.83840828888717311 ) ) ;
#36287 = CARTESIAN_POINT ( 'NONE',  ( 116.1082702545247827, -10.62599879583958717, -15.77991374673208469 ) ) ;
#36288 = CARTESIAN_POINT ( 'NONE',  ( 112.8529881442453302, -7.894159318335828068, -9.358103419637847864 ) ) ;
#36289 = EDGE_LOOP ( 'NONE', ( #2736, #9797, #38976, #457, #16518, #38504, #23012, #38408, #29238, #15863, #5122, #24833, #22489, #4657, #22160, #36495, #28063, #31860, #38415, #1136 ) ) ;
#36290 = ORIENTED_EDGE ( 'NONE', *, *, #39491, .F. ) ;
#36291 = CARTESIAN_POINT ( 'NONE',  ( 121.1350814775786233, -9.859900752359378018, -12.68260735090039759 ) ) ;
#36292 = CARTESIAN_POINT ( 'NONE',  ( 117.9583881442453048, 0.1319031606808879209, -14.10382304977623669 ) ) ;
#36293 = CARTESIAN_POINT ( 'NONE',  ( 83.32100367795761997, -14.50187442639529323, -16.89321520033831447 ) ) ;
#36294 = ORIENTED_EDGE ( 'NONE', *, *, #31968, .T. ) ;
#36295 = DIRECTION ( 'NONE',  ( 0.000000000000000000, 0.000000000000000000, -1.000000000000000000 ) ) ;
#36296 = CARTESIAN_POINT ( 'NONE',  ( 71.62231439647737830, -24.74987456741813929, -4.893215200338314474 ) ) ;
#36297 = CARTESIAN_POINT ( 'NONE',  ( 110.4131140045248287, -10.62599879583958717, -11.00651665394454604 ) ) ;
#36298 = CARTESIAN_POINT ( 'NONE',  ( 116.3700414775786527, -5.638512984488999180, -18.83840828888717311 ) ) ;
#36300 = CARTESIAN_POINT ( 'NONE',  ( 114.8951481442453115, -8.899110576539710493, -16.42337572283490132 ) ) ;
#36299 = CARTESIAN_POINT ( 'NONE',  ( 115.7460481442453357, 0.9020085738987339008, -11.91225656197089222 ) ) ;
#36301 = CARTESIAN_POINT ( 'NONE',  ( 121.0783548109119749, -9.565557343593413364, -10.61323700422348004 ) ) ;
#36302 = CARTESIAN_POINT ( 'NONE',  ( 85.04324155394569118, -25.99489077589524300, -13.39321520033831447 ) ) ;
#36303 = EDGE_LOOP ( 'NONE', ( #36735, #3905, #18038, #12446, #7850 ) ) ;
#36304 = CARTESIAN_POINT ( 'NONE',  ( 118.0718414775786442, -0.8288870151387760510, -10.36305467784173118 ) ) ;
#36305 = CARTESIAN_POINT ( 'NONE',  ( 125.4463081442452932, -4.153390946401325223, -8.397313243818185668 ) ) ;
#36306 = CARTESIAN_POINT ( 'NONE',  ( 112.5661608795247872, -8.938348069036489818, -9.318865927141430916 ) ) ;
#36307 = CARTESIAN_POINT ( 'NONE',  ( 115.9693640045247776, 0.1403307496149616695, -15.46607636864997204 ) ) ;
#36308 = CARTESIAN_POINT ( 'NONE',  ( 110.6214733795247867, -8.938348069036489818, -17.46756447353520159 ) ) ;
#36309 = CARTESIAN_POINT ( 'NONE',  ( 119.8303681442453126, -10.63000616557722466, -14.87417383870573495 ) ) ;
#36310 = ORIENTED_EDGE ( 'NONE', *, *, #797, .T. ) ;
#36311 = CARTESIAN_POINT ( 'NONE',  ( 120.1140014775786398, -1.561330072975668504, -17.79121239304076951 ) ) ;
#36312 = CARTESIAN_POINT ( 'NONE',  ( 62.62167863469137075, -37.39737710839052198, -5.203302251594248418 ) ) ;
#36313 = CARTESIAN_POINT ( 'NONE',  ( 107.0793640045248196, -10.62599879583958717, -11.00651665394454604 ) ) ;
#36314 = CARTESIAN_POINT ( 'NONE',  ( 114.6115148109119986, -3.383040157471821630, -19.15922257007629170 ) ) ;
#36315 = CARTESIAN_POINT ( 'NONE',  ( 119.3198281442452924, 0.5811942927096110934, -14.16772938898807510 ) ) ;
#36316 = CARTESIAN_POINT ( 'NONE',  ( 66.02672340405024443, -2.161076072907569756, -17.98865292984563169 ) ) ;
#36317 = CARTESIAN_POINT ( 'NONE',  ( 117.2221267808402985, -10.92304153767783959, -5.282372476044864484 ) ) ;
#36318 = VERTEX_POINT ( 'NONE', #16012 ) ;
#36319 = FACE_OUTER_BOUND ( 'NONE', #34920, .T. ) ;
#36320 = CARTESIAN_POINT ( 'NONE',  ( 109.2294471768124424, -10.42840437825952549, -12.68791898119246042 ) ) ;
#36321 = CARTESIAN_POINT ( 'NONE',  ( 119.1496481442453046, -6.222761293078241884, -8.102969835052219238 ) ) ;
#36322 = EDGE_CURVE ( 'NONE', #27364, #18078, #32369, .T. ) ;
#36323 = CARTESIAN_POINT ( 'NONE',  ( 111.1770983795247787, -8.402594152722688392, -16.93181055722141792 ) ) ;
#36324 = CARTESIAN_POINT ( 'NONE',  ( 115.9693640045247776, 0.1403307496149616695, -15.46607636864997204 ) ) ;
#36325 = CARTESIAN_POINT ( 'NONE',  ( 113.4202548109119846, 0.1319031606808879209, -14.10382304977623669 ) ) ;
#36326 = DIRECTION ( 'NONE',  ( 0.000000000000000000, -0.3713878862591642460, 0.9284778069183722282 ) ) ;
#36327 = CARTESIAN_POINT ( 'NONE',  ( 68.95535311261431843, -26.02754444259658584, -5.893215200338315363 ) ) ;
#36328 = CARTESIAN_POINT ( 'NONE',  ( 113.0231681442453180, -10.15424416112533912, -14.75197769757731336 ) ) ;
#36329 = CARTESIAN_POINT ( 'NONE',  ( 119.4332814775786318, -0.4660016031367893996, -10.09054647747474043 ) ) ;
#36330 = ORIENTED_EDGE ( 'NONE', *, *, #13189, .T. ) ;
#36331 = CARTESIAN_POINT ( 'NONE',  ( 118.6391081442452986, -5.574606645277164318, -18.38911715685844683 ) ) ;
#36332 = CARTESIAN_POINT ( 'NONE',  ( 114.6115148109119986, -3.383040157471821630, -19.15922257007629170 ) ) ;
#36333 = CARTESIAN_POINT ( 'NONE',  ( 123.0637881442452937, -0.4660016031367893996, -10.09054647747474043 ) ) ;
#36334 = CARTESIAN_POINT ( 'NONE',  ( 121.5321681442453183, -0.1624402480850797581, -16.17319339645315424 ) ) ;
#36335 = EDGE_LOOP ( 'NONE', ( #45026, #39948, #21305, #14875, #18977, #7522 ) ) ;
#36336 = CARTESIAN_POINT ( 'NONE',  ( 125.1059481442452750, -1.833838273342660141, -17.42832698103878286 ) ) ;
#36337 = CARTESIAN_POINT ( 'NONE',  ( 118.8092881442453290, -9.988377603198976828, -10.36322818467138340 ) ) ;
#36338 = CARTESIAN_POINT ( 'NONE',  ( 112.5693548109119888, 0.4262465694468514643, -12.03445270309931736 ) ) ;
#36339 = CARTESIAN_POINT ( 'NONE',  ( 122.2128881442453263, -1.834011780172310813, -8.268836392978581529 ) ) ;
#36340 = CARTESIAN_POINT ( 'NONE',  ( 105.8986608795248401, -8.938348069036489818, -9.318865927141430916 ) ) ;
#36341 = CARTESIAN_POINT ( 'NONE',  ( 77.05532149770296257, 0.06670422450934243574, -18.64321520033831803 ) ) ;
#36342 = CARTESIAN_POINT ( 'NONE',  ( 135.7012255816029551, -0.6896191363000495622, -17.70303589939592825 ) ) ;
#36343 = CARTESIAN_POINT ( 'NONE',  ( 113.4690515045247992, -6.936859964151250502, -18.39754474579286025 ) ) ;
#36344 = AXIS2_PLACEMENT_3D ( 'NONE', #13586, #11056, #25190 ) ;
#36345 = CARTESIAN_POINT ( 'NONE',  ( 70.19189222814998175, -58.73420832284057269, -33.46539274499136241 ) ) ;
#36346 = AXIS2_PLACEMENT_3D ( 'NONE', #5529, #25840, #36539 ) ;
#36347 = CARTESIAN_POINT ( 'NONE',  ( 136.2632467228252438, -10.25174699308209547, -11.13433988238026728 ) ) ;
#36348 = CARTESIAN_POINT ( 'NONE',  ( 116.5402214775786405, -9.565557343593413364, -10.61323700422348004 ) ) ;
#36349 = CARTESIAN_POINT ( 'NONE',  ( 112.2289948109119848, -7.643976991954077427, -18.09477374809248928 ) ) ;
#36350 = CARTESIAN_POINT ( 'NONE',  ( 65.37189491326753910, -13.54774410707433141, -14.64331257007126297 ) ) ;
#36351 = VERTEX_POINT ( 'NONE', #8946 ) ;
#36352 = CARTESIAN_POINT ( 'NONE',  ( 116.5944421295247793, -9.868328341294093420, -13.39321520033831447 ) ) ;
#36353 = CARTESIAN_POINT ( 'NONE',  ( 109.5796765045248122, -2.791137627527939813, -8.388885654883777576 ) ) ;
#36354 = CARTESIAN_POINT ( 'NONE',  ( 117.0507614775786465, 0.1319031606808879209, -14.10382304977623669 ) ) ;
#36355 = CARTESIAN_POINT ( 'NONE',  ( 115.1430393777725385, -1.267766418764730840, -16.93314635290706605 ) ) ;
#36356 = CARTESIAN_POINT ( 'NONE',  ( 107.2294421295247844, -9.051693226400931991, -21.89321520033831447 ) ) ;
#36357 = CARTESIAN_POINT ( 'NONE',  ( -1.894019060673375332, -6.852671617155902339, -18.74982798469211787 ) ) ;
#36359 = CARTESIAN_POINT ( 'NONE',  ( 121.4754414775786131, -8.166667518702819706, -8.995218007635861213 ) ) ;
#36358 = CARTESIAN_POINT ( 'NONE',  ( 64.78880510502027334, -15.59149258467484422, -11.31956754614451199 ) ) ;
#36360 = CARTESIAN_POINT ( 'NONE',  ( 123.0637881442452937, -8.899110576539710493, -16.42337572283490132 ) ) ;
#36361 = ORIENTED_EDGE ( 'NONE', *, *, #26999, .T. ) ;
#36362 = DIRECTION ( 'NONE',  ( 0.000000000000000000, -0.4669533266896288559, -0.8842819633428518067 ) ) ;
#36363 = DIRECTION ( 'NONE',  ( 0.000000000000000000, 0.000000000000000000, 1.000000000000000000 ) ) ;
#36364 = CARTESIAN_POINT ( 'NONE',  ( 107.9128015045248219, -6.936859964151250502, -18.39754474579286025 ) ) ;
#36365 = CARTESIAN_POINT ( 'NONE',  ( 122.2128881442453263, -7.643976991954077427, -18.09477374809248928 ) ) ;
#36366 = B_SPLINE_CURVE_WITH_KNOTS ( 'NONE', 3,
 ( #30402, #43861, #40441, #19679, #26760, #19916, #33339, #2573, #2344, #5538, #39979, #9202, #1667, #19456, #5320, #40669, #36768, #30177, #32891, #22650, #36989, #33801, #23112, #12634, #8742, #44095, #44324, #25849 ),
 .UNSPECIFIED., .F., .F.,
 ( 4, 2, 2, 2, 1, 1, 2, 2, 2, 2, 1, 1, 2, 2, 2, 4 ),
 ( 0.000000000000000000, 0.1249999999999990563, 0.1874999999999982514, 0.2187499999999976685, 0.2343749999999973077, 0.2421874999999971412, 0.2460937499999970579, 0.2499999999999969746, 0.3749999999999961697, 0.4374999999999955036, 0.4687499999999955036, 0.4843749999999956146, 0.4921874999999955591, 0.4999999999999955036, 0.7499999999999976685, 1.000000000000000000 ),
 .UNSPECIFIED. ) ;
#36367 = CARTESIAN_POINT ( 'NONE',  ( 122.5532481442453019, 0.4262465694468514643, -12.03445270309931736 ) ) ;
#36368 = CARTESIAN_POINT ( 'NONE',  ( 115.4056881442453459, -2.084020599724406786, -8.691656652584148546 ) ) ;
#36369 = CARTESIAN_POINT ( 'NONE',  ( 125.0480389746926022, 1.230434822596612188, -17.81742975626465153 ) ) ;
#36370 = CARTESIAN_POINT ( 'NONE',  ( 107.3571765045248299, -7.250697342233347165, -19.15521520033831138 ) ) ;
#36371 = CARTESIAN_POINT ( 'NONE',  ( 124.0281414775786146, -7.643976991954077427, -18.09477374809248928 ) ) ;
#36372 = CARTESIAN_POINT ( 'NONE',  ( 122.8936081442453059, -9.565557343593413364, -10.61323700422348004 ) ) ;
#36373 = CARTESIAN_POINT ( 'NONE',  ( 87.80477198183443477, -25.99489077589524300, -13.39321520033831625 ) ) ;
#36374 = CARTESIAN_POINT ( 'NONE',  ( 78.69189222814998175, -64.41823023953079996, -19.25521411788948711 ) ) ;
#36375 = CARTESIAN_POINT ( 'NONE',  ( 113.8163171295247764, -10.62599879583958540, -13.39321520033831447 ) ) ;
#36376 = CARTESIAN_POINT ( 'NONE',  ( -13.67812064622776802, -4.634518106585512776, -18.88472069773969153 ) ) ;
#36377 = CARTESIAN_POINT ( 'NONE',  ( 87.62389663665700823, -12.03403077406018440, -18.64321520033831803 ) ) ;
#36378 = CARTESIAN_POINT ( 'NONE',  ( 122.2128881442453263, -1.834011780172310813, -8.268836392978581529 ) ) ;
#36379 = CARTESIAN_POINT ( 'NONE',  ( 119.0361948109119652, -7.893985811506177619, -18.51759400769804742 ) ) ;
#36380 = CARTESIAN_POINT ( 'NONE',  ( 106.3153796295248412, -4.863998795839590272, -19.15521520033831493 ) ) ;
#36381 = CARTESIAN_POINT ( 'NONE',  ( 114.9518748109119883, -1.834011780172310813, -8.268836392978581529 ) ) ;
#36382 = DIRECTION ( 'NONE',  ( -8.728168432587710164E-16, -1.000000000000000000, 0.000000000000000000 ) ) ;
#36383 = VERTEX_POINT ( 'NONE', #43834 ) ;
#36384 = CARTESIAN_POINT ( 'NONE',  ( 116.0861162244890892, -0.02276961308034231024, -12.14321520033833934 ) ) ;
#36385 = CARTESIAN_POINT ( 'NONE',  ( 120.3976348109119812, -1.834011780172310813, -8.268836392978581529 ) ) ;
#36386 = AXIS2_PLACEMENT_3D ( 'NONE', #12059, #32562, #39867 ) ;
#36387 = CARTESIAN_POINT ( 'NONE',  ( 125.0492214775786266, -3.505236298600246325, -18.68346056562440793 ) ) ;
#36388 = DIRECTION ( 'NONE',  ( 0.000000000000000000, 0.000000000000000000, 1.000000000000000000 ) ) ;
#36389 = CARTESIAN_POINT ( 'NONE',  ( 112.7962614775786676, -6.222761293078241884, -8.102969835052219238 ) ) ;
#36390 = CARTESIAN_POINT ( 'NONE',  ( 112.0020881442453344, -9.565557343593413364, -10.61323700422348004 ) ) ;
#36391 = CARTESIAN_POINT ( 'NONE',  ( 108.0517077545248696, -7.250697342233347165, -7.631215200338321125 ) ) ;
#36392 = VECTOR ( 'NONE', #9770, 1000.000000000000000 ) ;
#36393 = CARTESIAN_POINT ( 'NONE',  ( 119.8870948109119752, -0.8288870151387760510, -10.36305467784173118 ) ) ;
#36394 = CARTESIAN_POINT ( 'NONE',  ( 70.19189222814998175, -100.0979043305785581, -53.24182196210380624 ) ) ;
#36395 = DIRECTION ( 'NONE',  ( 1.000000000000000000, 0.000000000000000000, -0.000000000000000000 ) ) ;
#36396 = ORIENTED_EDGE ( 'NONE', *, *, #18655, .F. ) ;
#36397 = AXIS2_PLACEMENT_3D ( 'NONE', #17913, #28405, #14269 ) ;
#36398 = FACE_OUTER_BOUND ( 'NONE', #38847, .T. ) ;
#36399 = CARTESIAN_POINT ( 'NONE',  ( 123.5743281442453139, -7.893985811506177619, -18.51759400769804742 ) ) ;
#36400 = PLANE ( 'NONE',  #39315 ) ;
#36401 = CARTESIAN_POINT ( 'NONE',  ( -13.48327269170832565, -4.890975110956025773, -7.580226695745068355 ) ) ;
#36402 = CARTESIAN_POINT ( 'NONE',  ( 115.1614878519202847, 0.2518737723193609224, -12.14321520033831625 ) ) ;
#36403 = CARTESIAN_POINT ( 'NONE',  ( 119.2631014775786298, -9.565557343593413364, -10.61323700422348004 ) ) ;
#36404 = CARTESIAN_POINT ( 'NONE',  ( 61.69189222814998175, -49.76310523276723785, -7.393215200338315363 ) ) ;
#36405 = CARTESIAN_POINT ( 'NONE',  ( 124.5063586819718324, -9.678300144053231691, -12.04321394670371603 ) ) ;
#36406 = CARTESIAN_POINT ( 'NONE',  ( 122.3830681442452857, -1.833838273342659697, -17.42832698103878286 ) ) ;
#36407 = EDGE_CURVE ( 'NONE', #8204, #32644, #33071, .T. ) ;
#36408 = MANIFOLD_SOLID_BREP ( 'NONE', #42527 ) ;
#36409 = CARTESIAN_POINT ( 'NONE',  ( 121.9272896737536911, -8.611453504372539314, -17.77011218421760574 ) ) ;
#36410 = CARTESIAN_POINT ( 'NONE',  ( 124.0281414775786146, -7.643976991954077427, -18.09477374809248928 ) ) ;
#36411 = CARTESIAN_POINT ( 'NONE',  ( 119.7434548109119703, -4.863998795839242995, -13.39321520033831447 ) ) ;
#36413 = B_SPLINE_CURVE_WITH_KNOTS ( 'NONE', 3,
 ( #13902, #3189, #3414, #41725, #42392, #24390, #38494, #27811, #7058, #21635 ),
 .UNSPECIFIED., .F., .F.,
 ( 4, 3, 3, 4 ),
 ( 1.939479807224430197E-18, 0.0002476486808869839996, 0.0004952973797228669853, 0.0009539399846111490172 ),
 .UNSPECIFIED. ) ;
#36412 = CARTESIAN_POINT ( 'NONE',  ( 123.0070614775786169, 0.9020085738987339008, -11.91225656197089222 ) ) ;
#36414 = CARTESIAN_POINT ( 'NONE',  ( 118.6391081442452986, -5.574606645277164318, -18.38911715685844683 ) ) ;
#36415 = ADVANCED_FACE ( 'NONE', ( #34227 ), #33536, .F. ) ;
#36416 = CARTESIAN_POINT ( 'NONE',  ( 124.8223148109119762, -10.15424416112533912, -14.75197769757731336 ) ) ;
#36417 = CARTESIAN_POINT ( 'NONE',  ( 122.9503348109119827, 0.5811942927096110934, -14.16772938898807510 ) ) ;
#36418 = CARTESIAN_POINT ( 'NONE',  ( 115.4624148109119943, -5.638512984488999180, -18.83840828888717311 ) ) ;
#36419 = CARTESIAN_POINT ( 'NONE',  ( 115.4831921295247952, -9.868328341294093420, -13.39321520033831447 ) ) ;
#36420 = CARTESIAN_POINT ( 'NONE',  ( 113.4202548109119846, -10.30919188438809542, -12.61870101168854852 ) ) ;
#36421 = CARTESIAN_POINT ( 'NONE',  ( 125.8433948109119456, -7.643976991954077427, -18.09477374809248928 ) ) ;
#36422 = ORIENTED_EDGE ( 'NONE', *, *, #22620, .F. ) ;
#36423 = CARTESIAN_POINT ( 'NONE',  ( 119.4900081442453086, -1.834011780172310813, -8.268836392978581529 ) ) ;
#36424 = CARTESIAN_POINT ( 'NONE',  ( 115.2748327545248657, -2.477300249445798297, -19.15521520033831138 ) ) ;
#36425 = CARTESIAN_POINT ( 'NONE',  ( 109.6491296295247793, -4.863998795839590272, -8.388885654883775800 ) ) ;
#36426 = CARTESIAN_POINT ( 'NONE',  ( 87.41631446019775353, -25.99489077589524300, -13.39321520033831625 ) ) ;
#36427 = CARTESIAN_POINT ( 'NONE',  ( 114.1009748109119784, -5.574606645277164318, -18.38911715685844683 ) ) ;
#36428 = CIRCLE ( 'NONE', #28445, 4.499999999999996447 ) ;
#36429 = CARTESIAN_POINT ( 'NONE',  ( 120.6463454359119822, -11.07370829466463569, -12.81314460846529002 ) ) ;
#36430 = CARTESIAN_POINT ( 'NONE',  ( 116.4555358795247884, -8.402594152722688392, -9.854619843455216355 ) ) ;
#36431 = ORIENTED_EDGE ( 'NONE', *, *, #25758, .F. ) ;
#36432 = VECTOR ( 'NONE', #31364, 1000.000000000000227 ) ;
#36433 = CARTESIAN_POINT ( 'NONE',  ( 124.6521348109119884, -7.894159318335828068, -9.358103419637847864 ) ) ;
#36434 = CARTESIAN_POINT ( 'NONE',  ( 122.3132204359119868, 1.345710702986147034, -13.97328579221134426 ) ) ;
#36435 = CARTESIAN_POINT ( 'NONE',  ( 123.1466579359119891, -5.444069387712269226, -19.60292469916370450 ) ) ;
#36436 = CARTESIAN_POINT ( 'NONE',  ( 93.44708369096697709, -29.69178914684045623, -14.92061247508468647 ) ) ;
#36437 = CARTESIAN_POINT ( 'NONE',  ( 108.1906140045248463, 0.1403307496149616695, -15.46607636864997204 ) ) ;
#36438 = EDGE_CURVE ( 'NONE', #11921, #10287, #32402, .T. ) ;
#36439 = VERTEX_POINT ( 'NONE', #33772 ) ;
#36440 = CARTESIAN_POINT ( 'NONE',  ( 114.8384214775786489, 0.9020085738987339008, -11.91225656197089222 ) ) ;
#36441 = CARTESIAN_POINT ( 'NONE',  ( 125.6164881442453094, 0.2603800115204892296, -16.42320221600525088 ) ) ;
#36442 = CARTESIAN_POINT ( 'NONE',  ( 125.6732148109119862, -9.859900752359378018, -12.68260735090039759 ) ) ;
#36443 = CARTESIAN_POINT ( 'NONE',  ( 115.0653281442453277, -3.505236298600246325, -18.68346056562440793 ) ) ;
#36444 = CARTESIAN_POINT ( 'NONE',  ( 128.2184548109119930, -9.609004340414083245, -9.721032963308941177 ) ) ;
#36445 = CARTESIAN_POINT ( 'NONE',  ( 119.7434548109119703, -11.17722486020181627, -8.479644537342501565 ) ) ;
#36446 = EDGE_CURVE ( 'NONE', #24723, #2587, #34577, .T. ) ;
#36447 = CARTESIAN_POINT ( 'NONE',  ( 115.8595014775786609, -1.834011780172310813, -8.268836392978581529 ) ) ;
#36448 = EDGE_CURVE ( 'NONE', #20559, #7488, #27180, .T. ) ;
#36449 = CARTESIAN_POINT ( 'NONE',  ( 113.5385046295247804, -4.863998795839590272, -18.39754474579285315 ) ) ;
#36450 = AXIS2_PLACEMENT_3D ( 'NONE', #37688, #20149, #31065 ) ;
#36451 = CARTESIAN_POINT ( 'NONE',  ( 124.3685014775786328, -10.63000616557722466, -14.87417383870573495 ) ) ;
#36452 = CARTESIAN_POINT ( 'NONE',  ( 90.99708770779186295, -26.75858941326842810, -11.54476601486570964 ) ) ;
#36453 = ORIENTED_EDGE ( 'NONE', *, *, #33171, .T. ) ;
#36454 = CARTESIAN_POINT ( 'NONE',  ( 115.7460481442453357, 0.9020085738987339008, -11.91225656197089222 ) ) ;
#36455 = CARTESIAN_POINT ( 'NONE',  ( 112.0020881442453344, -9.565557343593413364, -10.61323700422348004 ) ) ;
#36456 = EDGE_CURVE ( 'NONE', #38956, #11695, #27632, .T. ) ;
#36457 = PLANE ( 'NONE',  #43875 ) ;
#36458 = CARTESIAN_POINT ( 'NONE',  ( 126.1270281442452870, 0.1319031606808879209, -14.10382304977623669 ) ) ;
#36459 = EDGE_LOOP ( 'NONE', ( #41302, #8317, #41652, #489, #18248, #8264 ) ) ;
#36460 = CARTESIAN_POINT ( 'NONE',  ( 117.6180281442453150, -0.4660016031367893996, -10.09054647747474043 ) ) ;
#36461 = CARTESIAN_POINT ( 'NONE',  ( 59.62174278132244609, -14.86814543204979344, -8.593215200338315540 ) ) ;
#36462 = LINE ( 'NONE', #5232, #10228 ) ;
#36463 = AXIS2_PLACEMENT_3D ( 'NONE', #12772, #5236, #32815 ) ;
#36464 = EDGE_CURVE ( 'NONE', #26462, #4322, #16406, .T. ) ;
#36465 = CARTESIAN_POINT ( 'NONE',  ( 69.69189222814998175, -41.76310523276723785, -19.39321520033831447 ) ) ;
#36466 = ADVANCED_FACE ( 'NONE', ( #37658 ), #9859, .F. ) ;
#36467 = EDGE_CURVE ( 'NONE', #166, #10084, #23991, .T. ) ;
#36468 = CARTESIAN_POINT ( 'NONE',  ( 135.5886503745646792, -2.475940008444037943, -7.888983817636334273 ) ) ;
#36469 = CARTESIAN_POINT ( 'NONE',  ( 113.9307948109119764, -10.15424416112533912, -14.75197769757731336 ) ) ;
#36470 = DIRECTION ( 'NONE',  ( 0.000000000000000000, 0.000000000000000000, 1.000000000000000000 ) ) ;
#36471 = CARTESIAN_POINT ( 'NONE',  ( 125.1602731999475537, -1.814607927093800255, -20.13360068303625283 ) ) ;
#36472 = CARTESIAN_POINT ( 'NONE',  ( 111.8886348109120092, -6.222761293078241884, -8.102969835052219238 ) ) ;
#36473 = CARTESIAN_POINT ( 'NONE',  ( 126.0703014775786102, -0.1624402480850797581, -16.17319339645315424 ) ) ;
#36474 = CARTESIAN_POINT ( 'NONE',  ( 116.6823128682102748, -8.240270276191195009, -17.20524534304492192 ) ) ;
#36475 = CARTESIAN_POINT ( 'NONE',  ( 122.3263414775786373, -3.505236298600246325, -18.68346056562440793 ) ) ;
#36476 = CARTESIAN_POINT ( 'NONE',  ( 65.04064389207671582, -15.49774878834461056, -16.33482031564782488 ) ) ;
#36477 = CARTESIAN_POINT ( 'NONE',  ( 123.1205148109119563, -1.834011780172310813, -8.268836392978581529 ) ) ;
#36478 = CARTESIAN_POINT ( 'NONE',  ( 122.0427081442452817, 0.5811942927096110934, -14.16772938898807510 ) ) ;
#36479 = ORIENTED_EDGE ( 'NONE', *, *, #23681, .T. ) ;
#36480 = CARTESIAN_POINT ( 'NONE',  ( 114.4099712410415748, 0.7607806665037644134, -12.14321520033829316 ) ) ;
#36481 = CARTESIAN_POINT ( 'NONE',  ( 109.9269421295247753, 0.8980012041604618078, -13.39321520033831447 ) ) ;
#36482 = CARTESIAN_POINT ( 'NONE',  ( 111.5243640045248412, 0.1403307496149616695, -15.46607636864997204 ) ) ;
#36483 = CARTESIAN_POINT ( 'NONE',  ( 109.9963952545248134, -9.868328341294098749, -15.46607636864997204 ) ) ;
#36484 = CIRCLE ( 'NONE', #16859, 1.610000000000000986 ) ;
#36485 = CARTESIAN_POINT ( 'NONE',  ( 125.1626748109119802, -0.1624402480845399399, -16.17319339645223053 ) ) ;
#36486 = CARTESIAN_POINT ( 'NONE',  ( 116.4267681442453153, -3.383040157471821630, -19.15922257007629170 ) ) ;
#36487 = ORIENTED_EDGE ( 'NONE', *, *, #26957, .T. ) ;
#36488 = LINE ( 'NONE', #41457, #8815 ) ;
#36489 = FACE_OUTER_BOUND ( 'NONE', #25311, .T. ) ;
#36490 = CARTESIAN_POINT ( 'NONE',  ( 116.0864081442453113, -0.1624402480850797581, -16.17319339645315424 ) ) ;
#36491 = CARTESIAN_POINT ( 'NONE',  ( 122.8959708535611242, -2.239543233855044946, -18.13706010537467606 ) ) ;
#36492 = CARTESIAN_POINT ( 'NONE',  ( 118.5823814775786360, -1.834011780172310813, -8.268836392978581529 ) ) ;
#36493 = CARTESIAN_POINT ( 'NONE',  ( 111.5243640045248412, -10.62599879583958717, -11.00651665394454604 ) ) ;
#36494 = CARTESIAN_POINT ( 'NONE',  ( 119.2263198309151164, -2.215723800389698184, -18.16877924232191788 ) ) ;
#36495 = ORIENTED_EDGE ( 'NONE', *, *, #13684, .F. ) ;
#36496 = CARTESIAN_POINT ( 'NONE',  ( 122.4767535264548854, -8.247323210606174015, -17.08054893949881858 ) ) ;
#36497 = VECTOR ( 'NONE', #27310, 1000.000000000000227 ) ;
#36498 = CARTESIAN_POINT ( 'NONE',  ( 120.2274548109119934, -9.859900752359374465, -12.68260735090039404 ) ) ;
#36499 = CARTESIAN_POINT ( 'NONE',  ( 114.9518748109119883, -1.834011780172310813, -8.268836392978581529 ) ) ;
#36500 = CARTESIAN_POINT ( 'NONE',  ( 117.1642148109119859, -9.261995988541697145, -16.69588392320189030 ) ) ;
#36501 = CARTESIAN_POINT ( 'NONE',  ( 59.24641515291911986, -13.72835195454734247, -18.19321520033831519 ) ) ;
#36502 = CARTESIAN_POINT ( 'NONE',  ( 121.8725281442453223, -6.222761293078241884, -8.102969835052219238 ) ) ;
#36503 = CARTESIAN_POINT ( 'NONE',  ( 120.2274548109119934, -9.859900752359378018, -12.68260735090039759 ) ) ;
#36504 = ORIENTED_EDGE ( 'NONE', *, *, #26777, .T. ) ;
#36505 = CARTESIAN_POINT ( 'NONE',  ( 120.4379860609119675, -6.564341423271550902, -7.887810678476487425 ) ) ;
#36506 = CARTESIAN_POINT ( 'NONE',  ( 111.7184548109119788, -9.261995988541697145, -16.69588392320189030 ) ) ;
#36507 = CARTESIAN_POINT ( 'NONE',  ( 116.6536748109119941, -10.15424416112533912, -14.75197769757731336 ) ) ;
#36508 = ORIENTED_EDGE ( 'NONE', *, *, #11402, .T. ) ;
#36509 = DIRECTION ( 'NONE',  ( -1.000000000000000000, 0.000000000000000000, 0.000000000000000000 ) ) ;
#36510 = CARTESIAN_POINT ( 'NONE',  ( 115.7460481442453357, 0.9020085738987339008, -11.91225656197089222 ) ) ;
#36511 = CARTESIAN_POINT ( 'NONE',  ( 115.6220983795247861, -0.7896495226426338832, -9.318865927141430916 ) ) ;
#36512 = CARTESIAN_POINT ( 'NONE',  ( 114.0442481442453300, -7.643976991954077427, -18.09477374809248928 ) ) ;
#36513 = ADVANCED_FACE ( 'NONE', ( #13940 ), #37880, .F. ) ;
#36514 = VERTEX_POINT ( 'NONE', #16468 ) ;
#36515 = VERTEX_POINT ( 'NONE', #23768 ) ;
#36516 = AXIS2_PLACEMENT_3D ( 'NONE', #44480, #34634, #3420 ) ;
#36517 = CARTESIAN_POINT ( 'NONE',  ( 121.4187148109119789, -3.505236298600246325, -18.68346056562440793 ) ) ;
#36518 = CARTESIAN_POINT ( 'NONE',  ( 122.7801548109119665, -6.222761293078241884, -8.102969835052219238 ) ) ;
#36519 = DIRECTION ( 'NONE',  ( 0.000000000000000000, 0.000000000000000000, 1.000000000000000000 ) ) ;
#36520 = VERTEX_POINT ( 'NONE', #30372 ) ;
#36521 = CARTESIAN_POINT ( 'NONE',  ( 112.1691149257650579, -8.910908836065232208, -16.40337021355369629 ) ) ;
#36522 = CARTESIAN_POINT ( 'NONE',  ( 62.73714355202354653, -64.74057374251856345, -45.90754283741456732 ) ) ;
#36523 = CARTESIAN_POINT ( 'NONE',  ( 108.1906140045248463, -10.62599879583958717, -11.00651665394454604 ) ) ;
#36524 = CARTESIAN_POINT ( 'NONE',  ( 116.1431348109119881, -10.30919188438810075, -12.61870101168855918 ) ) ;
#36526 = CARTESIAN_POINT ( 'NONE',  ( 115.8595014775786609, -7.643976991954077427, -18.09477374809248928 ) ) ;
#36525 = CARTESIAN_POINT ( 'NONE',  ( 116.1431348109119881, -10.30919188438810075, -12.61870101168855918 ) ) ;
#36527 = ADVANCED_FACE ( 'NONE', ( #6197, #34003 ), #34443, .T. ) ;
#36528 = CARTESIAN_POINT ( 'NONE',  ( 120.8514481442452961, -2.084020599724406786, -8.691656652584148546 ) ) ;
#36529 = DIRECTION ( 'NONE',  ( 0.9609149988134843001, -0.1028163501681632064, 0.2570431154366505933 ) ) ;
#36530 = EDGE_LOOP ( 'NONE', ( #14394, #34914, #6116, #13177 ) ) ;
#36531 = CARTESIAN_POINT ( 'NONE',  ( 119.4332814775786318, -8.899110576539710493, -16.42337572283490132 ) ) ;
#36532 = CARTESIAN_POINT ( 'NONE',  ( 128.2184548109119930, -4.863998795839242995, -13.39321520033831447 ) ) ;
#36533 = CARTESIAN_POINT ( 'NONE',  ( 112.2883483795247770, -0.7896495226426338832, -9.318865927141430916 ) ) ;
#36534 = CARTESIAN_POINT ( 'NONE',  ( 80.41643495664496299, -3.865424785743087899, -16.39321520033831447 ) ) ;
#36535 = CARTESIAN_POINT ( 'NONE',  ( 112.1494421295248003, 0.8980012041604618078, -13.39321520033831447 ) ) ;
#36536 = CARTESIAN_POINT ( 'NONE',  ( 118.6391081442452986, -4.089484607189486809, -7.948022111789456723 ) ) ;
#36537 = ORIENTED_EDGE ( 'NONE', *, *, #17908, .F. ) ;
#36538 = CARTESIAN_POINT ( 'NONE',  ( 122.4965214775786251, -10.30919188438810075, -12.61870101168855918 ) ) ;
#36539 = DIRECTION ( 'NONE',  ( 0.9609149988134837450, -0.1028163501681639419, 0.2570431154366518145 ) ) ;
#36540 = CARTESIAN_POINT ( 'NONE',  ( 107.2877233795247776, -8.938348069036489818, -17.46756447353520159 ) ) ;
#36541 = CARTESIAN_POINT ( 'NONE',  ( 118.6391081442452986, -4.089484607189486809, -7.948022111789456723 ) ) ;
#36542 = CARTESIAN_POINT ( 'NONE',  ( 117.9016614775786280, -9.988377603198976828, -10.36322818467138340 ) ) ;
#36543 = LINE ( 'NONE', #22871, #6086 ) ;
#36544 = CYLINDRICAL_SURFACE ( 'NONE', #36613, 8.000000000000000000 ) ;
#36545 = ORIENTED_EDGE ( 'NONE', *, *, #20500, .F. ) ;
#36546 = FACE_OUTER_BOUND ( 'NONE', #12258, .T. ) ;
#36547 = CARTESIAN_POINT ( 'NONE',  ( 109.2295002756012963, -10.42642047080344270, -13.52344292549696014 ) ) ;
#36548 = CARTESIAN_POINT ( 'NONE',  ( 120.8514481442452961, -2.084020599724406786, -8.691656652584148546 ) ) ;
#36549 = CARTESIAN_POINT ( 'NONE',  ( 110.4131140045248287, 0.1403307496149616695, -15.46607636864997204 ) ) ;
#36550 = CARTESIAN_POINT ( 'NONE',  ( 114.4413952545248350, -9.868328341294098749, -15.46607636864997204 ) ) ;
#36551 = CARTESIAN_POINT ( 'NONE',  ( 116.7671281442453335, -7.643976991954077427, -18.09477374809248928 ) ) ;
#36552 = DIRECTION ( 'NONE',  ( 0.000000000000000000, 0.000000000000000000, 1.000000000000000000 ) ) ;
#36553 = CARTESIAN_POINT ( 'NONE',  ( 69.87170781386352303, -25.28162009068048732, -5.721420406450495655 ) ) ;
#36554 = CARTESIAN_POINT ( 'NONE',  ( 112.6260814775786514, -0.8288870151387760510, -10.36305467784173118 ) ) ;
#36555 = CARTESIAN_POINT ( 'NONE',  ( 118.6391081442452986, -4.089484607189486809, -7.948022111789456723 ) ) ;
#36556 = ORIENTED_EDGE ( 'NONE', *, *, #24435, .F. ) ;
#36557 = CARTESIAN_POINT ( 'NONE',  ( 119.0929214775786278, -4.153390946401325223, -8.397313243818185668 ) ) ;
#36558 = VECTOR ( 'NONE', #26960, 1000.000000000000000 ) ;
#36559 = CARTESIAN_POINT ( 'NONE',  ( 114.6682414775786469, -1.561330072975668060, -17.79121239304076596 ) ) ;
#36560 = CARTESIAN_POINT ( 'NONE',  ( 120.7379948109119709, -10.63000616557722466, -14.87417383870573495 ) ) ;
#36561 = CARTESIAN_POINT ( 'NONE',  ( 123.3474214775786209, -0.1624402480850797581, -16.17319339645315424 ) ) ;
#36562 = VERTEX_POINT ( 'NONE', #6432 ) ;
#36563 = CARTESIAN_POINT ( 'NONE',  ( 116.1954459692789641, -1.179503403430490538, -17.05068175419388865 ) ) ;
#36564 = EDGE_CURVE ( 'NONE', #18777, #35294, #12763, .T. ) ;
#36565 = CARTESIAN_POINT ( 'NONE',  ( 119.2631014775786298, 0.2603800115204892296, -16.42320221600525088 ) ) ;
#36566 = CARTESIAN_POINT ( 'NONE',  ( 112.3991748109119868, -1.833838273342658809, -17.42832698103878286 ) ) ;
#36567 = CARTESIAN_POINT ( 'NONE',  ( 124.9357681442453014, -1.834011780172310813, -8.268836392978581529 ) ) ;
#36568 = CARTESIAN_POINT ( 'NONE',  ( 106.5237390045248418, 0.8980012041604421569, -15.77991374673208469 ) ) ;
#36569 = CARTESIAN_POINT ( 'NONE',  ( 121.0630641859119976, -8.321307733199551748, -9.223433127585318303 ) ) ;
#36570 = CARTESIAN_POINT ( 'NONE',  ( 68.07789357685331311, -71.37500728601287392, -39.55955678403736897 ) ) ;
#36571 = CARTESIAN_POINT ( 'NONE',  ( 109.0935046295247872, -4.863998795839590272, -18.39754474579285315 ) ) ;
#36572 = AXIS2_PLACEMENT_3D ( 'NONE', #17478, #39965, #1651 ) ;
#36573 = ADVANCED_FACE ( 'NONE', ( #30819 ), #18253, .T. ) ;
#36574 = DIRECTION ( 'NONE',  ( 0.000000000000000000, 0.000000000000000000, -1.000000000000000000 ) ) ;
#36575 = CARTESIAN_POINT ( 'NONE',  ( 135.8497638153382070, -10.33978686199914598, -11.03243195220415451 ) ) ;
#36576 = CARTESIAN_POINT ( 'NONE',  ( 119.8870948109119752, -0.8288870151387760510, -10.36305467784173118 ) ) ;
#36577 = CARTESIAN_POINT ( 'NONE',  ( 125.9001214775786224, -4.089484607189486809, -7.948022111789456723 ) ) ;
#36578 = CARTESIAN_POINT ( 'NONE',  ( 64.33685879144834985, -13.01308064423183986, -15.68040082802806978 ) ) ;
#36579 = EDGE_LOOP ( 'NONE', ( #9958, #41224, #6484 ) ) ;
#36580 = CARTESIAN_POINT ( 'NONE',  ( 112.1237736387913770, -8.918551276432252095, -16.31957112036458568 ) ) ;
#36581 = CARTESIAN_POINT ( 'NONE',  ( 112.3578015045248861, -6.936859964151250502, -18.39754474579286025 ) ) ;
#36582 = CARTESIAN_POINT ( 'NONE',  ( 117.6180281442453150, -8.899110576539710493, -16.42337572283490132 ) ) ;
#36583 = DIRECTION ( 'NONE',  ( 1.000000000000000000, 0.000000000000000000, -0.000000000000000000 ) ) ;
#36584 = AXIS2_PLACEMENT_3D ( 'NONE', #43770, #44229, #12536 ) ;
#36585 = CARTESIAN_POINT ( 'NONE',  ( 67.31358133957452594, -0.1451868489720468947, -10.39321520033831625 ) ) ;
#36586 = CARTESIAN_POINT ( 'NONE',  ( -2.478595920918978290, -7.028301761946200266, -19.25792888057430829 ) ) ;
#36588 = CARTESIAN_POINT ( 'NONE',  ( 124.6521348109119884, -1.561330072975668948, -17.79121239304076951 ) ) ;
#36587 = CARTESIAN_POINT ( 'NONE',  ( 95.62170725701133733, -26.53666860750450951, -14.17427805189290346 ) ) ;
#36589 = CARTESIAN_POINT ( 'NONE',  ( 124.0848681442452772, -5.574606645277164318, -18.38911715685844683 ) ) ;
#36590 = ORIENTED_EDGE ( 'NONE', *, *, #14241, .T. ) ;
#36591 = FACE_OUTER_BOUND ( 'NONE', #4502, .T. ) ;
#36592 = CARTESIAN_POINT ( 'NONE',  ( 125.3895814775786448, -7.893985811506177619, -18.51759400769804742 ) ) ;
#36593 = CARTESIAN_POINT ( 'NONE',  ( 109.5102233795247884, -1.325403438956436419, -9.854619843455211026 ) ) ;
#36594 = CARTESIAN_POINT ( 'NONE',  ( 120.3976348109119812, -7.643976991954077427, -18.09477374809248928 ) ) ;
#36595 = CARTESIAN_POINT ( 'NONE',  ( 119.1496481442453046, -6.222761293078241884, -8.102969835052219238 ) ) ;
#36596 = CARTESIAN_POINT ( 'NONE',  ( 119.2255797424434149, -0.9924539043446216624, -17.29976612834909133 ) ) ;
#36597 = CARTESIAN_POINT ( 'NONE',  ( 110.2047546295247855, -4.863998795839590272, -7.631215200338315796 ) ) ;
#36598 = LINE ( 'NONE', #44147, #4037 ) ;
#36599 = CARTESIAN_POINT ( 'NONE',  ( 9.052690036452151645, -4.182915634381243919, -8.893215200338314474 ) ) ;
#36600 = FACE_OUTER_BOUND ( 'NONE', #2005, .T. ) ;
#36601 = EDGE_CURVE ( 'NONE', #21089, #31466, #39220, .T. ) ;
#36602 = CARTESIAN_POINT ( 'NONE',  ( 112.5661608795247872, -8.938348069036489818, -9.318865927141430916 ) ) ;
#36603 = DIRECTION ( 'NONE',  ( 0.000000000000000000, -0.3818493186865936084, 0.9242245927363024194 ) ) ;
#36604 = CARTESIAN_POINT ( 'NONE',  ( 116.5249890045247980, 0.8980012041604421569, -15.77991374673208469 ) ) ;
#36605 = CARTESIAN_POINT ( 'NONE',  ( 121.3619881442452879, -4.089484607189486809, -7.948022111789456723 ) ) ;
#36606 = CARTESIAN_POINT ( 'NONE',  ( 122.5532481442453019, -10.63000616557722466, -14.87417383870573495 ) ) ;
#36607 = CARTESIAN_POINT ( 'NONE',  ( 105.8292077545248446, -7.250697342233347165, -7.631215200338321125 ) ) ;
#36608 = CARTESIAN_POINT ( 'NONE',  ( 117.9016614775786280, -9.988377603198976828, -10.36322818467138340 ) ) ;
#36609 = CARTESIAN_POINT ( 'NONE',  ( 124.6894688159050872, -8.253847584685239269, -17.09290432062678278 ) ) ;
#36610 = VERTEX_POINT ( 'NONE', #28525 ) ;
#36611 = CARTESIAN_POINT ( 'NONE',  ( 90.04708369096697140, -25.51891511063604767, -13.19656280121471958 ) ) ;
#36612 = CARTESIAN_POINT ( 'NONE',  ( 124.3685014775786328, -10.63000616557722466, -14.87417383870573495 ) ) ;
#36613 = AXIS2_PLACEMENT_3D ( 'NONE', #5318, #8297, #8973 ) ;
#36614 = CARTESIAN_POINT ( 'NONE',  ( 121.4754414775786131, -8.166667518702819706, -8.995218007635861213 ) ) ;
#36615 = CARTESIAN_POINT ( 'NONE',  ( 125.9001214775786224, -5.574606645277164318, -18.38911715685844683 ) ) ;
#36616 = CARTESIAN_POINT ( 'NONE',  ( 114.7816948109119863, -9.859900752359374465, -12.68260735090039404 ) ) ;
#36617 = CARTESIAN_POINT ( 'NONE',  ( 124.6521348109119884, -1.561330072975668948, -17.79121239304076951 ) ) ;
#36618 = CARTESIAN_POINT ( 'NONE',  ( 107.0793640045248196, -10.62599879583958717, -11.00651665394454604 ) ) ;
#36619 = AXIS2_PLACEMENT_3D ( 'NONE', #12259, #40059, #22725 ) ;
#36620 = CARTESIAN_POINT ( 'NONE',  ( 118.4122014775786340, -9.859900752359374465, -12.68260735090039404 ) ) ;
#36621 = CARTESIAN_POINT ( 'NONE',  ( 116.7836398906078017, -3.487082921028213711, -18.39717223183647477 ) ) ;
#36622 = CARTESIAN_POINT ( 'NONE',  ( 92.04708369096698561, -25.99489077589524300, -13.39321520033831625 ) ) ;
#36623 = ORIENTED_EDGE ( 'NONE', *, *, #28663, .F. ) ;
#36624 = CARTESIAN_POINT ( 'NONE',  ( 90.20794100481921873, -11.57440209418094668, -8.143215200338314474 ) ) ;
#36625 = CARTESIAN_POINT ( 'NONE',  ( 121.4187148109119789, -6.344957434206665248, -7.627207830600338134 ) ) ;
#36626 = CARTESIAN_POINT ( 'NONE',  ( 113.6774108795247997, -1.325403438956436419, -16.93181055722138595 ) ) ;
#36627 = CARTESIAN_POINT ( 'NONE',  ( 67.30914723170953096, -54.88665770272660183, -36.05198880062562949 ) ) ;
#36628 = DIRECTION ( 'NONE',  ( 0.000000000000000000, 0.000000000000000000, -1.000000000000000000 ) ) ;
#36629 = EDGE_CURVE ( 'NONE', #11127, #26421, #43613, .T. ) ;
#36630 = CARTESIAN_POINT ( 'NONE',  ( 118.9794681442453026, -0.8288870151387760510, -10.36305467784173118 ) ) ;
#36631 = CARTESIAN_POINT ( 'NONE',  ( 68.14538754644013352, -1.022943911447667720, -16.39321520033830737 ) ) ;
#36632 = CARTESIAN_POINT ( 'NONE',  ( 121.9470836909669913, -25.99489077589524300, -13.39321520033831447 ) ) ;
#36633 = CARTESIAN_POINT ( 'NONE',  ( 122.7234281442452755, -4.153390946401325223, -8.397313243818185668 ) ) ;
#36634 = CARTESIAN_POINT ( 'NONE',  ( 123.6854187682627781, -1.040089454026960292, -17.23633227186633476 ) ) ;
#36635 =( GEOMETRIC_REPRESENTATION_CONTEXT ( 3 ) GLOBAL_UNCERTAINTY_ASSIGNED_CONTEXT ( ( #28224 ) ) GLOBAL_UNIT_ASSIGNED_CONTEXT ( ( #35773, #42860, #8423 ) ) REPRESENTATION_CONTEXT ( 'NONE', 'WORKASPACE' ) );
#36636 = CARTESIAN_POINT ( 'NONE',  ( 125.4584548109119737, -5.999156839134895947, -18.26265215102791473 ) ) ;
#36637 = AXIS2_PLACEMENT_3D ( 'NONE', #22317, #14575, #36212 ) ;
#36638 = CARTESIAN_POINT ( 'NONE',  ( 125.3447737754104736, -11.69827971232593455, -15.21530341384118401 ) ) ;
#36639 = CARTESIAN_POINT ( 'NONE',  ( 121.1350814775786233, 0.5811942927096110934, -14.16772938898807510 ) ) ;
#36640 = CARTESIAN_POINT ( 'NONE',  ( 115.8595014775786609, -7.643976991954077427, -18.09477374809248928 ) ) ;
#36641 = CARTESIAN_POINT ( 'NONE',  ( 121.5321681442453183, -0.1624402480850797581, -16.17319339645315424 ) ) ;
#36642 = ORIENTED_EDGE ( 'NONE', *, *, #34210, .T. ) ;
#36643 = CARTESIAN_POINT ( 'NONE',  ( 123.3474214775786209, -9.988377603198976828, -10.36322818467138340 ) ) ;
#36644 = CARTESIAN_POINT ( 'NONE',  ( 114.3846081442453197, -10.63000616557722466, -14.87417383870573495 ) ) ;
#36645 = CARTESIAN_POINT ( 'NONE',  ( 113.2606921295247702, -9.868328341294093420, -13.39321520033831447 ) ) ;
#36646 = CARTESIAN_POINT ( 'NONE',  ( 112.5126281442453120, 0.1319031606808879209, -14.10382304977623669 ) ) ;
#36647 = CARTESIAN_POINT ( 'NONE',  ( 124.3117748109119844, 0.1319031606808879209, -14.10382304977623669 ) ) ;
#36648 = CARTESIAN_POINT ( 'NONE',  ( 124.4819548109119722, -7.893985811506177619, -18.51759400769804742 ) ) ;
#36649 = CARTESIAN_POINT ( 'NONE',  ( 114.3719421295247827, 0.8980012041604618078, -13.39321520033831447 ) ) ;
#36650 = CARTESIAN_POINT ( 'NONE',  ( 109.5102233795247884, -1.325403438956436419, -9.854619843455211026 ) ) ;
#36651 = CARTESIAN_POINT ( 'NONE',  ( 83.83554121260367253, -25.99489077589524300, -13.39321520033831625 ) ) ;
#36652 = VECTOR ( 'NONE', #6363, 1000.000000000000000 ) ;
#36653 = DIRECTION ( 'NONE',  ( 0.000000000000000000, -0.3818493186865936084, 0.9242245927363024194 ) ) ;
#36654 = CARTESIAN_POINT ( 'NONE',  ( 112.6356140045247827, 0.1403307496149616695, -15.46607636864997204 ) ) ;
#36655 = EDGE_LOOP ( 'NONE', ( #24182, #12386, #10721, #17555 ) ) ;
#36656 = CARTESIAN_POINT ( 'NONE',  ( 125.7866681442452688, -8.899110576539710493, -16.42337572283490132 ) ) ;
#36657 = CARTESIAN_POINT ( 'NONE',  ( 123.2855641859119942, -0.8832429491016019485, -18.19431474523657855 ) ) ;
#36658 = CARTESIAN_POINT ( 'NONE',  ( 121.9659548109119811, -7.554583864224885481, -18.48844787311982785 ) ) ;
#36659 = CARTESIAN_POINT ( 'NONE',  ( 94.20708369096698220, -26.21217205256509075, -14.21600912764254687 ) ) ;
#36660 = CARTESIAN_POINT ( 'NONE',  ( 106.3153796295248412, -4.863998795839590272, -8.388885654883775800 ) ) ;
#36661 = ORIENTED_EDGE ( 'NONE', *, *, #33534, .T. ) ;
#36662 = CARTESIAN_POINT ( 'NONE',  ( 118.3554748109119998, 0.2603800115204892296, -16.42320221600525088 ) ) ;
#36663 = CARTESIAN_POINT ( 'NONE',  ( 123.8012348109119642, -9.565557343593413364, -10.61323700422348004 ) ) ;
#36664 = CARTESIAN_POINT ( 'NONE',  ( 116.1998614775786507, 0.4262465694468514643, -12.03445270309931736 ) ) ;
#36665 = FILL_AREA_STYLE_COLOUR ( '', #43089 ) ;
#36666 = CARTESIAN_POINT ( 'NONE',  ( 86.34560043013698305, -9.320000780048239619, -9.893215200338316251 ) ) ;
#36667 = SHAPE_REPRESENTATION ( 'MAT-055', ( #40983, #19122, #24253, #24947, #16966, #15478, #44624, #25703 ), #10411 ) ;
#36668 = LINE ( 'NONE', #22769, #34650 ) ;
#36669 = CARTESIAN_POINT ( 'NONE',  ( 115.8027748109119841, -0.4660016031367893996, -10.09054647747474043 ) ) ;
#36670 = CARTESIAN_POINT ( 'NONE',  ( 112.5661608795247872, -1.325403438956436419, -16.93181055722141792 ) ) ;
#36671 = CARTESIAN_POINT ( 'NONE',  ( 123.5176014775786228, -9.261995988541697145, -16.69588392320189030 ) ) ;
#36672 = FILL_AREA_STYLE ('',( #37357 ) ) ;
#36673 = VERTEX_POINT ( 'NONE', #32147 ) ;
#36674 = CARTESIAN_POINT ( 'NONE',  ( 113.3068014775786594, -8.166667518702817929, -8.995218007635859436 ) ) ;
#36675 = CARTESIAN_POINT ( 'NONE',  ( 113.8173414775786512, -9.565557343593413364, -10.61323700422348004 ) ) ;
#36676 = DIRECTION ( 'NONE',  ( 0.000000000000000000, 0.000000000000000000, -1.000000000000000000 ) ) ;
#36677 = CARTESIAN_POINT ( 'NONE',  ( 126.0135748109119902, -1.833838273342660141, -17.42832698103878286 ) ) ;
#36678 = ORIENTED_EDGE ( 'NONE', *, *, #20834, .T. ) ;
#36679 = CARTESIAN_POINT ( 'NONE',  ( 122.7801548109119665, -3.383040157471821630, -19.15922257007629170 ) ) ;
#36680 = PLANE ( 'NONE',  #42753 ) ;
#36681 = CARTESIAN_POINT ( 'NONE',  ( 120.2023751563572347, -9.242038528452065194, -16.16155152458310695 ) ) ;
#36682 = DIRECTION ( 'NONE',  ( 1.000000000000000000, 0.000000000000000000, 0.000000000000000000 ) ) ;
#36683 = CARTESIAN_POINT ( 'NONE',  ( 123.2184548109119788, -3.410847707154505137, -16.57729307524250828 ) ) ;
#36684 = CARTESIAN_POINT ( 'NONE',  ( 115.2922348109119781, 0.4262465694468514643, -12.03445270309931736 ) ) ;
#36685 = EDGE_CURVE ( 'NONE', #40611, #41698, #33828, .T. ) ;
#36686 = LINE ( 'NONE', #26452, #35718 ) ;
#36687 = CARTESIAN_POINT ( 'NONE',  ( 125.3194757386390847, -2.314088454569425135, -20.05232376479858658 ) ) ;
#36688 = CARTESIAN_POINT ( 'NONE',  ( 111.8319081442453182, -4.153390946401321671, -8.397313243818183892 ) ) ;
#36689 = CARTESIAN_POINT ( 'NONE',  ( 113.3068014775786594, -8.166667518702817929, -8.995218007635859436 ) ) ;
#36690 = CARTESIAN_POINT ( 'NONE',  ( 123.2161110609119703, -6.340755971794695078, -8.611740276972781771 ) ) ;
#36691 = CARTESIAN_POINT ( 'NONE',  ( 125.9001214775786224, -5.574606645277164318, -18.38911715685844683 ) ) ;
#36692 = CARTESIAN_POINT ( 'NONE',  ( 115.8595014775786609, -7.643976991954077427, -18.09477374809248928 ) ) ;
#36693 = CARTESIAN_POINT ( 'NONE',  ( 122.1561614775786353, -0.4660016031367893996, -10.09054647747474043 ) ) ;
#36694 = CIRCLE ( 'NONE', #33812, 11.00000000000000000 ) ;
#36695 = CARTESIAN_POINT ( 'NONE',  ( 120.6812681442452941, -10.30919188438810075, -12.61870101168855918 ) ) ;
#36696 = VERTEX_POINT ( 'NONE', #11419 ) ;
#36697 = CARTESIAN_POINT ( 'NONE',  ( 126.5254139959020847, -8.556035843926350637, -16.98867727300566699 ) ) ;
#36698 = EDGE_CURVE ( 'NONE', #37016, #33070, #5856, .T. ) ;
#36699 = CARTESIAN_POINT ( 'NONE',  ( 110.6909265045248247, -7.250697342233347165, -19.15521520033831138 ) ) ;
#36700 = CARTESIAN_POINT ( 'NONE',  ( 108.2600671295247992, 0.1403307496149613920, -13.39321520033831447 ) ) ;
#36701 = CARTESIAN_POINT ( 'NONE',  ( 110.4131140045248287, 0.1403307496149616695, -15.46607636864997204 ) ) ;
#36702 = CARTESIAN_POINT ( 'NONE',  ( 125.4463081442453500, -4.153390946402302220, -8.397313243818043560 ) ) ;
#36703 = CARTESIAN_POINT ( 'NONE',  ( 113.5904348109119866, -7.893985811506177619, -18.51759400769804742 ) ) ;
#36704 = ORIENTED_EDGE ( 'NONE', *, *, #32690, .T. ) ;
#36705 = CARTESIAN_POINT ( 'NONE',  ( 126.2404814775786264, -9.261995988541697145, -16.69588392320189030 ) ) ;
#36706 = CARTESIAN_POINT ( 'NONE',  ( 124.5966688623432219, -9.713577380183913590, -14.62808432448665563 ) ) ;
#36707 = DIRECTION ( 'NONE',  ( 1.000000000000000000, 0.000000000000000000, -0.000000000000000000 ) ) ;
#36708 = CARTESIAN_POINT ( 'NONE',  ( 114.0442481442453300, -7.643976991954077427, -18.09477374809248928 ) ) ;
#36709 = CARTESIAN_POINT ( 'NONE',  ( 119.2631014775786298, 0.2603800115204892296, -16.42320221600525088 ) ) ;
#36710 = CARTESIAN_POINT ( 'NONE',  ( 108.4684265045247997, -7.250697342233347165, -19.15521520033831138 ) ) ;
#36711 = DIRECTION ( 'NONE',  ( -0.000000000000000000, -0.9284778069183721172, -0.3713878862591650232 ) ) ;
#36712 = EDGE_LOOP ( 'NONE', ( #30943, #22938, #42052, #5154, #11249 ) ) ;
#36713 = DIRECTION ( 'NONE',  ( 0.000000000000000000, 0.000000000000000000, -1.000000000000000000 ) ) ;
#36714 = CARTESIAN_POINT ( 'NONE',  ( 121.7023481442452919, -0.8288870151387760510, -10.36305467784173118 ) ) ;
#36715 = CARTESIAN_POINT ( 'NONE',  ( 119.3198281442452924, 0.5811942927096110934, -14.16772938898807510 ) ) ;
#36716 = CARTESIAN_POINT ( 'NONE',  ( 113.9307948109119764, -10.15424416112533912, -14.75197769757731336 ) ) ;
#36717 = CARTESIAN_POINT ( 'NONE',  ( 115.2922348109119781, -10.63000616557722466, -14.87417383870573495 ) ) ;
#36718 = ADVANCED_FACE ( 'NONE', ( #21894 ), #25327, .T. ) ;
#36719 = CARTESIAN_POINT ( 'NONE',  ( 136.0073873814629337, -7.187683303096414456, -18.83671677009607848 ) ) ;
#36720 = CARTESIAN_POINT ( 'NONE',  ( 122.2128881442453263, -7.643976991954077427, -18.09477374809248928 ) ) ;
#36721 = CARTESIAN_POINT ( 'NONE',  ( 120.6245414775786458, -0.1624402480850797581, -16.17319339645315424 ) ) ;
#36722 = ORIENTED_EDGE ( 'NONE', *, *, #39569, .F. ) ;
#36723 = EDGE_CURVE ( 'NONE', #35430, #37642, #33102, .T. ) ;
#36724 = EDGE_CURVE ( 'NONE', #33768, #27673, #4557, .T. ) ;
#36725 = CONICAL_SURFACE ( 'NONE', #1068, 2.445500000000004448, 0.9599310885968757034 ) ;
#36726 = CARTESIAN_POINT ( 'NONE',  ( 94.20708369096698220, -25.26022072204669655, -13.82270432939535709 ) ) ;
#36727 = CARTESIAN_POINT ( 'NONE',  ( 111.7751814775786556, -7.893985811506177619, -18.51759400769804742 ) ) ;
#36728 = CARTESIAN_POINT ( 'NONE',  ( 123.1205148109119563, -7.643976991954077427, -18.09477374809248928 ) ) ;
#36729 = ORIENTED_EDGE ( 'NONE', *, *, #40798, .T. ) ;
#36730 = CARTESIAN_POINT ( 'NONE',  ( 120.7852516859119731, -0.6942167230862511529, -9.935906262978006609 ) ) ;
#36731 = CARTESIAN_POINT ( 'NONE',  ( 117.3911214775786505, -1.561330072975668504, -17.79121239304076951 ) ) ;
#36732 = CIRCLE ( 'NONE', #25099, 2.999999999999999556 ) ;
#36733 = CARTESIAN_POINT ( 'NONE',  ( 114.4413952545248350, 0.8980012041604421569, -11.00651665394454071 ) ) ;
#36734 = CARTESIAN_POINT ( 'NONE',  ( 117.7882081442453170, -3.505236298600246325, -18.68346056562440793 ) ) ;
#36735 = ORIENTED_EDGE ( 'NONE', *, *, #23687, .T. ) ;
#36736 = VERTEX_POINT ( 'NONE', #12091 ) ;
#36737 = CARTESIAN_POINT ( 'NONE',  ( 121.7023481442452919, -0.8288870151387760510, -10.36305467784173118 ) ) ;
#36738 = CARTESIAN_POINT ( 'NONE',  ( 121.7590748109119687, -2.084020599724406786, -8.691656652584148546 ) ) ;
#36739 = SURFACE_STYLE_FILL_AREA ( #12601 ) ;
#36740 = CARTESIAN_POINT ( 'NONE',  ( 31.16856251326850824, -20.50830283073288385, -18.19321520033831519 ) ) ;
#36741 = CARTESIAN_POINT ( 'NONE',  ( 61.80825783966907494, -65.83929257108415811, -43.67008539085770025 ) ) ;
#36742 = CARTESIAN_POINT ( 'NONE',  ( 117.9016614775786280, -9.988377603198976828, -10.36322818467138340 ) ) ;
#36743 = DIRECTION ( 'NONE',  ( -0.000000000000000000, -0.9284778069183718952, -0.3713878862591649677 ) ) ;
#36744 = CARTESIAN_POINT ( 'NONE',  ( 116.3133148109119759, -7.893985811506177619, -18.51759400769804742 ) ) ;
#36746 = CARTESIAN_POINT ( 'NONE',  ( 116.6536748109119941, -10.15424416112533912, -14.75197769757731336 ) ) ;
#36745 = CARTESIAN_POINT ( 'NONE',  ( 116.5402214775786405, 0.2603800115204892296, -16.42320221600525088 ) ) ;
#36747 = CARTESIAN_POINT ( 'NONE',  ( 119.5467348109119712, -5.574606645277164318, -18.38911715685844683 ) ) ;
#36748 = DIRECTION ( 'NONE',  ( -0.000000000000000000, -0.9284778069183721172, -0.3713878862591650232 ) ) ;
#36749 = ORIENTED_EDGE ( 'NONE', *, *, #33337, .T. ) ;
#36750 = CARTESIAN_POINT ( 'NONE',  ( 122.0994348109119443, -10.15424416112533912, -14.75197769757731336 ) ) ;
#36751 = ADVANCED_FACE ( 'NONE', ( #8442 ), #28776, .T. ) ;
#36752 = CARTESIAN_POINT ( 'NONE',  ( 113.8979809388149533, -2.287189184988692059, -18.07361239780447448 ) ) ;
#36753 = AXIS2_PLACEMENT_3D ( 'NONE', #24374, #18195, #7930 ) ;
#36754 = CARTESIAN_POINT ( 'NONE',  ( 112.6356140045247827, -10.62599879583958717, -11.00651665394454604 ) ) ;
#36755 = CARTESIAN_POINT ( 'NONE',  ( 112.7050671295247923, 0.1403307496149613920, -13.39321520033831447 ) ) ;
#36756 = CARTESIAN_POINT ( 'NONE',  ( 113.2606921295247702, 0.8980012041604618078, -13.39321520033831447 ) ) ;
#36757 = CARTESIAN_POINT ( 'NONE',  ( 118.9227414775786400, -10.63000616557722466, -14.87417383870573495 ) ) ;
#36758 = ORIENTED_EDGE ( 'NONE', *, *, #23941, .T. ) ;
#36759 = CARTESIAN_POINT ( 'NONE',  ( 121.9859814775786333, 0.2603800115204892296, -16.42320221600525088 ) ) ;
#36760 = LINE ( 'NONE', #18779, #9427 ) ;
#36761 = CARTESIAN_POINT ( 'NONE',  ( 107.1488171295247867, -10.62599879583958540, -13.39321520033831447 ) ) ;
#36762 = CARTESIAN_POINT ( 'NONE',  ( 120.7947214775786193, -9.261995988541697145, -16.69588392320189030 ) ) ;
#36763 = CARTESIAN_POINT ( 'NONE',  ( 116.2565881442452991, -9.261995988541697145, -16.69588392320189030 ) ) ;
#36765 = CIRCLE ( 'NONE', #4718, 2.999999999999999556 ) ;
#36764 = DIRECTION ( 'NONE',  ( -0.8636456077245080465, 0.5040994586965603652, 0.000000000000000000 ) ) ;
#36766 = CARTESIAN_POINT ( 'NONE',  ( 114.2354127111058659, -1.267766418764742165, -16.93314635290707315 ) ) ;
#36767 = ORIENTED_EDGE ( 'NONE', *, *, #32690, .F. ) ;
#36768 = CARTESIAN_POINT ( 'NONE',  ( -2.175944109879409449, -6.937465585941038348, -7.722225285168071274 ) ) ;
#36769 = CARTESIAN_POINT ( 'NONE',  ( 109.2294844673402423, -10.43718104171506944, -13.11406945123205858 ) ) ;
#36770 = CARTESIAN_POINT ( 'NONE',  ( 121.4754414775786131, -1.833838273342659697, -17.42832698103878286 ) ) ;
#36771 = CARTESIAN_POINT ( 'NONE',  ( 113.3301452545248083, -9.868328341294098749, -15.46607636864997204 ) ) ;
#36772 = CARTESIAN_POINT ( 'NONE',  ( 113.1217858795247935, -8.402594152722688392, -9.854619843455216355 ) ) ;
#36773 = CARTESIAN_POINT ( 'NONE',  ( 119.6034614775786196, -3.505236298600246325, -18.68346056562440793 ) ) ;
#36774 = FACE_OUTER_BOUND ( 'NONE', #19635, .T. ) ;
#36775 = CARTESIAN_POINT ( 'NONE',  ( 71.24792571258848284, -26.61500810931513428, -5.214987668974215396 ) ) ;
#36776 = CARTESIAN_POINT ( 'NONE',  ( 113.2500748109119968, -3.505236298600246325, -18.68346056562440793 ) ) ;
#36777 = CARTESIAN_POINT ( 'NONE',  ( 122.6667014775786413, -7.893985811506177619, -18.51759400769804742 ) ) ;
#36778 = ORIENTED_EDGE ( 'NONE', *, *, #3317, .T. ) ;
#36779 = EDGE_CURVE ( 'NONE', #32851, #29903, #22221, .T. ) ;
#36780 = CARTESIAN_POINT ( 'NONE',  ( 120.4543614775786295, -5.574606645277164318, -18.38911715685844683 ) ) ;
#36781 = CARTESIAN_POINT ( 'NONE',  ( 115.1787814775786387, -9.988377603198976828, -10.36322818467138340 ) ) ;
#36782 = CARTESIAN_POINT ( 'NONE',  ( 121.4754414775786131, -8.166667518702819706, -8.995218007635861213 ) ) ;
#36783 = CARTESIAN_POINT ( 'NONE',  ( 123.6310548109119765, -4.153390946401325223, -8.397313243818185668 ) ) ;
#36784 = EDGE_LOOP ( 'NONE', ( #10845, #14062, #26367, #13994, #33446 ) ) ;
#36785 = EDGE_CURVE ( 'NONE', #37027, #21347, #8392, .T. ) ;
#36786 = CARTESIAN_POINT ( 'NONE',  ( 123.5176014775786228, -0.8288870151387760510, -10.36305467784173118 ) ) ;
#36787 = VECTOR ( 'NONE', #25939, 1000.000000000000000 ) ;
#36788 = CARTESIAN_POINT ( 'NONE',  ( 124.8223148109119762, 0.9020085738987339008, -11.91225656197089222 ) ) ;
#36789 = CARTESIAN_POINT ( 'NONE',  ( 125.0048763211383829, -8.133222562175093984, -6.560216017044333547 ) ) ;
#36790 = CARTESIAN_POINT ( 'NONE',  ( 111.3780948109119890, -5.574606645277164318, -18.38911715685844683 ) ) ;
#36791 = B_SPLINE_CURVE_WITH_KNOTS ( 'NONE', 3,
 ( #27020, #10146, #41614, #2835 ),
 .UNSPECIFIED., .F., .F.,
 ( 4, 4 ),
 ( 0.005938763149045529939, 0.008179074650722518991 ),
 .UNSPECIFIED. ) ;
#36792 = CARTESIAN_POINT ( 'NONE',  ( 105.6903015045248253, -2.477300249445798297, -7.631215200338321125 ) ) ;
#36793 = CARTESIAN_POINT ( 'NONE',  ( 120.7852516859119731, -0.6942167230862511529, -9.935906262978006609 ) ) ;
#36794 = CARTESIAN_POINT ( 'NONE',  ( 127.7862423803841381, -3.345148870660049845, -14.16624594358310141 ) ) ;
#36795 = CARTESIAN_POINT ( 'NONE',  ( 108.6073327545248048, -6.936859964151250502, -8.388885654883777576 ) ) ;
#36796 = CARTESIAN_POINT ( 'NONE',  ( 73.07463722459043254, -62.93137825908255678, -37.48083319807903280 ) ) ;
#36797 = CARTESIAN_POINT ( 'NONE',  ( 117.2985964273310060, -2.236191541394345172, -18.14152338500401029 ) ) ;
#36798 = CARTESIAN_POINT ( 'NONE',  ( 120.4543614775786295, -5.574606645277164318, -18.38911715685844683 ) ) ;
#36799 = CARTESIAN_POINT ( 'NONE',  ( 123.7445081442452874, -1.561330072975668948, -17.79121239304076951 ) ) ;
#36800 = CARTESIAN_POINT ( 'NONE',  ( 126.5177454662631220, -6.230080189768934851, -18.35871718775414152 ) ) ;
#36801 = VERTEX_POINT ( 'NONE', #26668 ) ;
#36802 = CARTESIAN_POINT ( 'NONE',  ( 116.2471765045247594, -2.791137627527939813, -8.388885654883777576 ) ) ;
#36803 = CARTESIAN_POINT ( 'NONE',  ( 107.7044421295247929, -9.868328341294093420, -13.39321520033831447 ) ) ;
#36804 = CARTESIAN_POINT ( 'NONE',  ( 117.2776681442452968, -4.153390946401321671, -8.397313243818183892 ) ) ;
#36805 = CARTESIAN_POINT ( 'NONE',  ( 93.24708369096698846, -28.02818487991510921, -14.23328370144882093 ) ) ;
#36806 = CARTESIAN_POINT ( 'NONE',  ( 67.17917282099325860, -0.1070896992261115427, -10.39321520033831447 ) ) ;
#36807 = CARTESIAN_POINT ( 'NONE',  ( 124.1800355643466673, -1.244021962887375432, -16.96476564598603431 ) ) ;
#36809 = CARTESIAN_POINT ( 'NONE',  ( 123.0070614775786169, 0.9020085738987339008, -11.91225656197089222 ) ) ;
#36808 = DIRECTION ( 'NONE',  ( 0.5735764363510499342, 0.3127926500124801890, -0.7570804645221008711 ) ) ;
#36810 = CARTESIAN_POINT ( 'NONE',  ( 122.3263414775786373, -3.505236298600246325, -18.68346056562440793 ) ) ;
#36811 = ORIENTED_EDGE ( 'NONE', *, *, #36180, .F. ) ;
#36812 = DIRECTION ( 'NONE',  ( 0.9908103287288505534, -0.1352586133457945317, 0.000000000000000000 ) ) ;
#36813 = CARTESIAN_POINT ( 'NONE',  ( 124.9924948109119924, -4.089484607189486809, -7.948022111789456723 ) ) ;
#36814 = CARTESIAN_POINT ( 'NONE',  ( 110.2742077545248094, -2.791137627527939813, -18.39754474579286025 ) ) ;
#36815 = EDGE_CURVE ( 'NONE', #27848, #11611, #12273, .T. ) ;
#36816 = CARTESIAN_POINT ( 'NONE',  ( 121.9859814775786333, -9.565557343593413364, -10.61323700422348004 ) ) ;
#36817 = CARTESIAN_POINT ( 'NONE',  ( 119.3765548109119834, -10.15424416112533912, -14.75197769757731336 ) ) ;
#36818 = CARTESIAN_POINT ( 'NONE',  ( 74.69189222814998175, -41.76310523276723785, -20.39321520033831447 ) ) ;
#36819 = CARTESIAN_POINT ( 'NONE',  ( 115.2748327545248657, -6.936859964151250502, -8.388885654883777576 ) ) ;
#36820 = DIRECTION ( 'NONE',  ( 0.000000000000000000, -0.3818493186865927203, 0.9242245927363029745 ) ) ;
#36821 = CARTESIAN_POINT ( 'NONE',  ( 73.07463722459043254, -58.28898922449070596, -35.62389376678321184 ) ) ;
#36822 = DIRECTION ( 'NONE',  ( -2.439015257082815255E-15, 1.000000000000000000, 0.000000000000000000 ) ) ;
#36823 = CARTESIAN_POINT ( 'NONE',  ( 111.1076452545248259, 0.8980012041604421569, -11.00651665394454071 ) ) ;
#36824 = CARTESIAN_POINT ( 'NONE',  ( -13.50689678881128231, -4.859881301483246041, -18.09470388050485568 ) ) ;
#36825 = CARTESIAN_POINT ( 'NONE',  ( 116.1082702545247827, -10.62599879583958717, -15.77991374673208469 ) ) ;
#36826 = CARTESIAN_POINT ( 'NONE',  ( 119.9438214775786378, -7.893985811506177619, -18.51759400769804742 ) ) ;
#36827 = CARTESIAN_POINT ( 'NONE',  ( 121.0216281442452981, -1.561330072975668948, -17.79121239304076951 ) ) ;
#36828 = CARTESIAN_POINT ( 'NONE',  ( 108.1906140045248463, -10.62599879583958717, -11.00651665394454604 ) ) ;
#36829 = CARTESIAN_POINT ( 'NONE',  ( 116.8805814775786445, -6.344957434206662583, -7.627207830600332805 ) ) ;
#36830 = CARTESIAN_POINT ( 'NONE',  ( 113.4769814775786330, -10.63000616557722466, -14.87417383870573495 ) ) ;
#36831 = ORIENTED_EDGE ( 'NONE', *, *, #10025, .F. ) ;
#36832 = CARTESIAN_POINT ( 'NONE',  ( 116.1351496632429416, -0.3638222789105182153, -10.82232390540186984 ) ) ;
#36833 = CIRCLE ( 'NONE', #27390, 2.000000000000000444 ) ;
#36834 = CARTESIAN_POINT ( 'NONE',  ( 121.6456214775786293, -10.63000616557722466, -14.87417383870573495 ) ) ;
#36835 = CARTESIAN_POINT ( 'NONE',  ( 121.8158014775786171, -5.638512984488999180, -18.83840828888717311 ) ) ;
#36836 = EDGE_CURVE ( 'NONE', #17122, #25324, #8810, .T. ) ;
#36837 = CARTESIAN_POINT ( 'NONE',  ( 111.9453614775786434, -1.561330072975668060, -17.79121239304076596 ) ) ;
#36838 = CONTEXT_DEPENDENT_SHAPE_REPRESENTATION ( #27967, #32139 ) ;
#36839 = CARTESIAN_POINT ( 'NONE',  ( 111.6617281442453304, 0.4262465694468514643, -12.03445270309931736 ) ) ;
#36840 = CARTESIAN_POINT ( 'NONE',  ( 115.7460481442453357, -10.15424416112533912, -14.75197769757731336 ) ) ;
#36841 = CARTESIAN_POINT ( 'NONE',  ( 124.5954081442453116, -3.383040157471821630, -19.15922257007629170 ) ) ;
#36842 = CARTESIAN_POINT ( 'NONE',  ( 109.5102233795247884, -8.938348069036489818, -17.46756447353520159 ) ) ;
#36843 = CARTESIAN_POINT ( 'NONE',  ( 119.6034614775786196, -3.505236298600246325, -18.68346056562440793 ) ) ;
#36844 = CARTESIAN_POINT ( 'NONE',  ( 110.5520202545248196, -10.62599879583953388, -15.77991374673210601 ) ) ;
#36845 = VECTOR ( 'NONE', #23334, 1000.000000000000000 ) ;
#36846 = DIRECTION ( 'NONE',  ( 1.000000000000000000, 0.000000000000000000, 0.000000000000000000 ) ) ;
#36847 = VERTEX_POINT ( 'NONE', #29862 ) ;
#36848 = DIRECTION ( 'NONE',  ( -8.728168432587710164E-16, -1.000000000000000000, 0.000000000000000000 ) ) ;
#36849 = CARTESIAN_POINT ( 'NONE',  ( 124.1415948109119540, -6.344957434206665248, -7.627207830600338134 ) ) ;
#36850 = VECTOR ( 'NONE', #37607, 1000.000000000000000 ) ;
#36851 = DIRECTION ( 'NONE',  ( 0.000000000000000000, 0.9284778069183720062, 0.3713878862591650232 ) ) ;
#36852 = CARTESIAN_POINT ( 'NONE',  ( 124.6574308310811858, 2.898587707825708293, -12.35876450466414056 ) ) ;
#36853 = CARTESIAN_POINT ( 'NONE',  ( 67.05222635936684128, -0.08653180621725030386, -16.39321520033831092 ) ) ;
#36854 = CARTESIAN_POINT ( 'NONE',  ( 88.35093386163799778, -25.99489077589524300, -13.39321520033831447 ) ) ;
#36855 = CARTESIAN_POINT ( 'NONE',  ( 124.9357681442453014, -7.643976991954077427, -18.09477374809248928 ) ) ;
#36856 = DIRECTION ( 'NONE',  ( 0.9609149988134843001, -0.1028163501681632064, 0.2570431154366505933 ) ) ;
#36857 = CIRCLE ( 'NONE', #26660, 2.999999999999999556 ) ;
#36858 = DIRECTION ( 'NONE',  ( 0.000000000000000000, -0.3818493186865936084, 0.9242245927363024194 ) ) ;
#36859 = CARTESIAN_POINT ( 'NONE',  ( 125.3513934876002764, -11.54857932371512419, -15.65469058310272210 ) ) ;
#36860 = CARTESIAN_POINT ( 'NONE',  ( 125.6164881442453094, 0.2603800115204892296, -16.42320221600525088 ) ) ;
#36861 = CARTESIAN_POINT ( 'NONE',  ( 116.9373081442452929, -1.833838273342659253, -17.42832698103878286 ) ) ;
#36862 = CARTESIAN_POINT ( 'NONE',  ( 119.7434548109119561, -1.843432898259047992, -17.99896722079169464 ) ) ;
#36863 = EDGE_LOOP ( 'NONE', ( #43905, #11404, #34300, #11244, #16710, #23930, #32437 ) ) ;
#36864 = CARTESIAN_POINT ( 'NONE',  ( 124.8790414775786246, -0.4660016031367893996, -10.09054647747474043 ) ) ;
#36865 = CARTESIAN_POINT ( 'NONE',  ( 116.9940348109119839, -9.988377603198976828, -10.36322818467138340 ) ) ;
#36866 = CARTESIAN_POINT ( 'NONE',  ( 114.3719421295247827, -9.868328341294093420, -13.39321520033831447 ) ) ;
#36867 = CARTESIAN_POINT ( 'NONE',  ( 113.7038881442453402, -6.222761293078241884, -8.102969835052219238 ) ) ;
#36868 = CARTESIAN_POINT ( 'NONE',  ( 124.8790414775786246, -8.899110576539710493, -16.42337572283490132 ) ) ;
#36869 = CARTESIAN_POINT ( 'NONE',  ( 122.7801548109119665, -3.383040157471821630, -19.15922257007629170 ) ) ;
#36870 = CARTESIAN_POINT ( 'NONE',  ( 106.1764733795248219, -1.325403438956436419, -9.854619843455211026 ) ) ;
#36871 = CARTESIAN_POINT ( 'NONE',  ( 109.2324108795247923, -1.325403438956436419, -16.93181055722141792 ) ) ;
#36872 = DIRECTION ( 'NONE',  ( -0.1352586133458019424, -0.9908103287288495542, 0.000000000000000000 ) ) ;
#36873 = DIRECTION ( 'NONE',  ( 0.9609149988134837450, -0.1028163501681639419, 0.2570431154366518145 ) ) ;
#36874 = CARTESIAN_POINT ( 'NONE',  ( 117.5613014775786525, -10.15424416112533912, -14.75197769757731336 ) ) ;
#36875 = DIRECTION ( 'NONE',  ( 0.000000000000000000, 0.000000000000000000, -1.000000000000000000 ) ) ;
#36876 = CIRCLE ( 'NONE', #39069, 2.000000000000000444 ) ;
#36877 = CARTESIAN_POINT ( 'NONE',  ( 113.9552233795247815, -1.325403438956436419, -9.854619843455211026 ) ) ;
#36878 = ORIENTED_EDGE ( 'NONE', *, *, #41778, .T. ) ;
#36879 = CARTESIAN_POINT ( 'NONE',  ( 124.3117748109119844, 0.1319031606808879209, -14.10382304977623669 ) ) ;
#36880 = CARTESIAN_POINT ( 'NONE',  ( 120.5768923109119868, -0.4387604401700512802, -15.73000352943951619 ) ) ;
#36881 = CARTESIAN_POINT ( 'NONE',  ( 122.4521266859119635, -0.06289925094097943703, -9.412459353600674206 ) ) ;
#36882 = ORIENTED_EDGE ( 'NONE', *, *, #40516, .F. ) ;
#36883 = CARTESIAN_POINT ( 'NONE',  ( 88.22708560785949317, -3.622631779710408395, -18.64321520033831803 ) ) ;
#36884 = CARTESIAN_POINT ( 'NONE',  ( 105.0652233795248378, -1.325403438956436419, -9.854619843455211026 ) ) ;
#36885 = VECTOR ( 'NONE', #43569, 1000.000000000000114 ) ;
#36886 = ORIENTED_EDGE ( 'NONE', *, *, #17508, .T. ) ;
#36887 = CARTESIAN_POINT ( 'NONE',  ( 118.2420214775786320, -3.383040157471821630, -19.15922257007629170 ) ) ;
#36888 = CARTESIAN_POINT ( 'NONE',  ( 125.3328548109119964, -0.8288870151387760510, -10.36305467784173118 ) ) ;
#36889 = EDGE_CURVE ( 'NONE', #31933, #30574, #31649, .T. ) ;
#36890 = CARTESIAN_POINT ( 'NONE',  ( 113.2500748109119968, -3.505236298600246325, -18.68346056562440793 ) ) ;
#36891 = FACE_OUTER_BOUND ( 'NONE', #3705, .T. ) ;
#36892 = CARTESIAN_POINT ( 'NONE',  ( 71.36400868967236022, -24.42718413923373788, -4.893215200338314474 ) ) ;
#36893 = CARTESIAN_POINT ( 'NONE',  ( 116.2565881442452991, -9.261995988541697145, -16.69588392320189030 ) ) ;
#36894 = CIRCLE ( 'NONE', #17963, 2.999999999999999556 ) ;
#36895 = CARTESIAN_POINT ( 'NONE',  ( 111.8021765045248372, -2.791137627527939813, -8.388885654883777576 ) ) ;
#36896 = CARTESIAN_POINT ( 'NONE',  ( 125.9568481442452850, -6.344957434206665248, -7.627207830600338134 ) ) ;
#36897 = FACE_OUTER_BOUND ( 'NONE', #40166, .T. ) ;
#36898 = ORIENTED_EDGE ( 'NONE', *, *, #20016, .F. ) ;
#36899 = CARTESIAN_POINT ( 'NONE',  ( 115.2355081442453155, -10.30919188438810075, -12.61870101168855918 ) ) ;
#36900 = CARTESIAN_POINT ( 'NONE',  ( 114.1009748109119784, -5.574606645277164318, -18.38911715685844683 ) ) ;
#36901 = CARTESIAN_POINT ( 'NONE',  ( 126.3539348109119800, -4.153390946401325223, -8.397313243818185668 ) ) ;
#36902 = ORIENTED_EDGE ( 'NONE', *, *, #43987, .F. ) ;
#36903 = CARTESIAN_POINT ( 'NONE',  ( 121.7023481442452777, -9.261995988541697145, -16.69588392320189030 ) ) ;
#36905 = DIRECTION ( 'NONE',  ( 0.000000000000000000, -0.3818493186865927203, 0.9242245927363029745 ) ) ;
#36904 = AXIS2_PLACEMENT_3D ( 'NONE', #42262, #7592, #11027 ) ;
#36906 = DIRECTION ( 'NONE',  ( 1.000000000000000000, 0.000000000000000000, 0.000000000000000000 ) ) ;
#36907 = CARTESIAN_POINT ( 'NONE',  ( 135.8497638153212108, -2.503215547705048394, -7.917427134178404380 ) ) ;
#36908 = CARTESIAN_POINT ( 'NONE',  ( 113.3068014775786594, -1.833838273342658809, -17.42832698103878286 ) ) ;
#36909 = VECTOR ( 'NONE', #23654, 1000.000000000000000 ) ;
#36910 = FACE_OUTER_BOUND ( 'NONE', #27256, .T. ) ;
#36911 = CARTESIAN_POINT ( 'NONE',  ( 125.0488419420234010, -3.685100071787774212, -20.83256261096772732 ) ) ;
#36912 = CARTESIAN_POINT ( 'NONE',  ( 116.9940348109119839, -0.1624402480850797581, -16.17319339645315424 ) ) ;
#36913 = CARTESIAN_POINT ( 'NONE',  ( 126.2404814775786264, -0.8288870151387760510, -10.36305467784173118 ) ) ;
#36914 = CARTESIAN_POINT ( 'NONE',  ( 124.1190016859119680, -0.6942167230862511529, -9.935906262978006609 ) ) ;
#36915 = CARTESIAN_POINT ( 'NONE',  ( 111.7751814775786556, -7.893985811506177619, -18.51759400769804742 ) ) ;
#36916 = CARTESIAN_POINT ( 'NONE',  ( 115.4624148109119943, -4.153390946401321671, -8.397313243818183892 ) ) ;
#36917 = CARTESIAN_POINT ( 'NONE',  ( 122.7234281442452755, -5.638512984488999180, -18.83840828888717311 ) ) ;
#36918 = AXIS2_PLACEMENT_3D ( 'NONE', #28414, #24331, #39117 ) ;
#36919 = CARTESIAN_POINT ( 'NONE',  ( 120.7379948109119709, -10.63000616557722466, -14.87417383870573495 ) ) ;
#36920 = ORIENTED_EDGE ( 'NONE', *, *, #7463, .F. ) ;
#36921 = CARTESIAN_POINT ( 'NONE',  ( 114.3846081442453197, -10.63000616557722466, -14.87417383870573495 ) ) ;
#36922 = CARTESIAN_POINT ( 'NONE',  ( 112.0799890045248475, 0.8980012041604421569, -15.77991374673208469 ) ) ;
#36923 = CARTESIAN_POINT ( 'NONE',  ( 111.2465515045248168, -6.936859964151250502, -18.39754474579286025 ) ) ;
#36924 = CARTESIAN_POINT ( 'NONE',  ( 108.6767858795247861, -8.402594152722688392, -9.854619843455216355 ) ) ;
#36925 = CARTESIAN_POINT ( 'NONE',  ( 109.2309317933750634, -8.902407557854933984, -9.282925415959930149 ) ) ;
#36926 = CARTESIAN_POINT ( 'NONE',  ( 118.1852948109119836, -5.638512984488999180, -18.83840828888717311 ) ) ;
#36927 = ORIENTED_EDGE ( 'NONE', *, *, #33064, .T. ) ;
#36928 = DIRECTION ( 'NONE',  ( 0.000000000000000000, 0.000000000000000000, -1.000000000000000000 ) ) ;
#36929 = CARTESIAN_POINT ( 'NONE',  ( 82.31000308962319423, -13.76004065658516673, -9.893215200338316251 ) ) ;
#36930 = CARTESIAN_POINT ( 'NONE',  ( 125.2761281442453196, -10.63000616557728506, -14.87417383870603160 ) ) ;
#36931 = CARTESIAN_POINT ( 'NONE',  ( 115.2355081442453155, 0.1319031606808879209, -14.10382304977623669 ) ) ;
#36932 =( BOUNDED_CURVE ( )  B_SPLINE_CURVE ( 2, ( #41082, #37639, #6413, #31679, #4313, #14816, #7967, #25528, #32576, #1120, #448, #25079, #28728 ),
 .UNSPECIFIED., .F., .F. ) 
 B_SPLINE_CURVE_WITH_KNOTS ( ( 3, 2, 2, 2, 2, 2, 3 ),
 ( 0.8296282416568590001, 0.8359375000000000000, 0.8437500000000000000, 0.8515625000000000000, 0.8593750000000000000, 0.8671875000000000000, 0.8750000000000000000 ),
 .UNSPECIFIED. ) 
 CURVE ( )  GEOMETRIC_REPRESENTATION_ITEM ( )  RATIONAL_B_SPLINE_CURVE ( ( 0.9763430640195970289, 0.9385262470928680267, 1.000000000000000000, 0.9238795325112869605, 1.000000000000000000, 0.9238795325112869605, 1.000000000000000000, 0.9238795325112869605, 1.000000000000000000, 0.9238795325112869605, 1.000000000000000000, 0.9238795325112869605, 1.000000000000000000 ) ) 
 REPRESENTATION_ITEM ( '' )  );
#36933 = CARTESIAN_POINT ( 'NONE',  ( 107.1488171295248861, 0.1403307496149613920, -13.39321520033831447 ) ) ;
#36934 = CARTESIAN_POINT ( 'NONE',  ( 120.7379948109119709, -10.63000616557722466, -14.87417383870573495 ) ) ;
#36935 = CARTESIAN_POINT ( 'NONE',  ( 115.2053796295247849, -4.863998795839590272, -8.388885654883775800 ) ) ;
#36936 = CARTESIAN_POINT ( 'NONE',  ( 67.30914723170953096, -56.95110010363538322, -36.87775856471080260 ) ) ;
#36937 = ORIENTED_EDGE ( 'NONE', *, *, #41745, .F. ) ;
#36938 = CARTESIAN_POINT ( 'NONE',  ( 61.76986277844709861, -39.32091226840162079, -6.340220811149025693 ) ) ;
#36939 = CARTESIAN_POINT ( 'NONE',  ( 120.9649014775786355, -6.222761293078241884, -8.102969835052219238 ) ) ;
#36940 = CARTESIAN_POINT ( 'NONE',  ( 119.8303681442453126, -10.63000616557722466, -14.87417383870573495 ) ) ;
#36941 = VECTOR ( 'NONE', #12215, 1000.000000000000000 ) ;
#36942 = CARTESIAN_POINT ( 'NONE',  ( 114.4413348109119823, -0.8288870151387760510, -10.36305467784173118 ) ) ;
#36943 = CARTESIAN_POINT ( 'NONE',  ( 116.3133148109119759, -7.893985811506177619, -18.51759400769804742 ) ) ;
#36944 = DIRECTION ( 'NONE',  ( -0.7071067811865480168, -0.5654279342906962658, -0.4246071727182139655 ) ) ;
#36945 = CARTESIAN_POINT ( 'NONE',  ( 121.9859814775786333, -9.565557343593413364, -10.61323700422348004 ) ) ;
#36946 = CARTESIAN_POINT ( 'NONE',  ( 119.7736414775786358, 0.1319031606808879209, -14.10382304977623669 ) ) ;
#36947 = VERTEX_POINT ( 'NONE', #43778 ) ;
#36948 = CARTESIAN_POINT ( 'NONE',  ( 113.7606148109119886, -1.561330072975668060, -17.79121239304076596 ) ) ;
#36949 = CARTESIAN_POINT ( 'NONE',  ( 119.6034614775786196, -3.505236298600246325, -18.68346056562440793 ) ) ;
#36950 = EDGE_LOOP ( 'NONE', ( #9219, #28158, #20877, #26237 ) ) ;
#36951 = CARTESIAN_POINT ( 'NONE',  ( 119.7434548109119703, -7.554583864224885481, -18.48844787311982785 ) ) ;
#36952 = CARTESIAN_POINT ( 'NONE',  ( 120.2274548109119934, 0.5811942927096110934, -14.16772938898807510 ) ) ;
#36953 = CARTESIAN_POINT ( 'NONE',  ( 114.5108483795247878, -0.7896495226426338832, -9.318865927141430916 ) ) ;
#36954 = CARTESIAN_POINT ( 'NONE',  ( 116.0296814775786345, -1.833838273342658809, -17.42832698103878286 ) ) ;
#36955 = VERTEX_POINT ( 'NONE', #12542 ) ;
#36956 = ORIENTED_EDGE ( 'NONE', *, *, #4563, .F. ) ;
#36957 = CARTESIAN_POINT ( 'NONE',  ( 124.9924948109119924, -5.574606645277164318, -18.38911715685844683 ) ) ;
#36958 = CARTESIAN_POINT ( 'NONE',  ( 121.0216281442452981, -7.894159318335828068, -9.358103419637847864 ) ) ;
#36959 = CARTESIAN_POINT ( 'NONE',  ( 86.34560043013698305, -9.320000780048239619, -9.893215200338316251 ) ) ;
#36960 = ORIENTED_EDGE ( 'NONE', *, *, #3633, .T. ) ;
#36961 = CARTESIAN_POINT ( 'NONE',  ( 116.9373081442452929, -8.166667518702817929, -8.995218007635861213 ) ) ;
#36962 = CARTESIAN_POINT ( 'NONE',  ( 107.2877233795247776, -8.938348069036489818, -17.46756447353520159 ) ) ;
#36963 = AXIS2_PLACEMENT_3D ( 'NONE', #26118, #16547, #36812 ) ;
#36964 = CARTESIAN_POINT ( 'NONE',  ( 116.0864081442453113, -9.988377603198976828, -10.36322818467138340 ) ) ;
#36966 = CARTESIAN_POINT ( 'NONE',  ( 115.0653281442453277, -3.505236298600246325, -18.68346056562440793 ) ) ;
#36965 = CARTESIAN_POINT ( 'NONE',  ( 115.5191414775786569, -3.383040157471821630, -19.15922257007629170 ) ) ;
#36967 = CARTESIAN_POINT ( 'NONE',  ( 123.8579614775786126, -9.859900752359378018, -12.68260735090039759 ) ) ;
#36968 = CARTESIAN_POINT ( 'NONE',  ( 113.9307948109119906, 0.9020085738987339008, -11.91225656197089222 ) ) ;
#36969 = EDGE_CURVE ( 'NONE', #42684, #529, #21325, .T. ) ;
#36970 = EDGE_CURVE ( 'NONE', #23478, #44558, #19148, .T. ) ;
#36971 = ORIENTED_EDGE ( 'NONE', *, *, #3140, .F. ) ;
#36972 = CARTESIAN_POINT ( 'NONE',  ( 124.1415948109119540, -3.505236298600246325, -18.68346056562440793 ) ) ;
#36973 = CARTESIAN_POINT ( 'NONE',  ( 122.3647822310133364, -1.244021962887374544, -16.96476564598603076 ) ) ;
#36974 = DIRECTION ( 'NONE',  ( 0.1352586133457950590, 0.9908103287288504424, 0.000000000000000000 ) ) ;
#36975 = CARTESIAN_POINT ( 'NONE',  ( 114.0246765045248196, -7.250697342233347165, -19.15521520033831138 ) ) ;
#36976 = CARTESIAN_POINT ( 'NONE',  ( 113.4690515045247992, -6.936859964151250502, -18.39754474579286025 ) ) ;
#36977 = CARTESIAN_POINT ( 'NONE',  ( 109.7185827545247889, -2.477300249445798297, -19.15521520033831138 ) ) ;
#36978 = CARTESIAN_POINT ( 'NONE',  ( 123.5176014775786228, -9.261995988541697145, -16.69588392320189030 ) ) ;
#36979 = ORIENTED_EDGE ( 'NONE', *, *, #25420, .F. ) ;
#36980 = CARTESIAN_POINT ( 'NONE',  ( 120.2274548109119934, 0.5811942927096110934, -14.16772938898807510 ) ) ;
#36981 = DIRECTION ( 'NONE',  ( 1.000000000000000000, 0.000000000000000000, 0.000000000000000000 ) ) ;
#36982 = CARTESIAN_POINT ( 'NONE',  ( 42.36021970110777346, -12.73296999994090761, -7.393215200338315363 ) ) ;
#36983 = CARTESIAN_POINT ( 'NONE',  ( 118.4122014775786340, 0.5811942927096110934, -14.16772938898807510 ) ) ;
#36984 = CARTESIAN_POINT ( 'NONE',  ( 122.2128881442453263, -1.834011780172310813, -8.268836392978581529 ) ) ;
#36985 = CARTESIAN_POINT ( 'NONE',  ( 123.6776560953690591, -6.001247023715324147, -18.26661038929047010 ) ) ;
#36986 = CARTESIAN_POINT ( 'NONE',  ( 120.7026895652850556, -6.239497348973052304, -18.71779138178827040 ) ) ;
#36987 = CARTESIAN_POINT ( 'NONE',  ( 120.2990798109119766, -7.200787124940443817, -17.81845355600750835 ) ) ;
#36988 = ORIENTED_EDGE ( 'NONE', *, *, #6923, .F. ) ;
#36989 = CARTESIAN_POINT ( 'NONE',  ( -2.071618846624489585, -6.906063984103743891, -7.819288697422720702 ) ) ;
#36990 = CARTESIAN_POINT ( 'NONE',  ( 114.5757164273310167, -2.236191541394345172, -18.14152338500401029 ) ) ;
#36991 = CARTESIAN_POINT ( 'NONE',  ( 123.6310548109119765, -4.153390946401325223, -8.397313243818185668 ) ) ;
#36992 = CARTESIAN_POINT ( 'NONE',  ( 116.2471765045247594, -7.250697342233347165, -19.15521520033831138 ) ) ;
#36993 = CARTESIAN_POINT ( 'NONE',  ( 111.8021765045248372, -2.791137627527939813, -8.388885654883777576 ) ) ;
#36994 = CARTESIAN_POINT ( 'NONE',  ( 117.3911214775786505, -7.894159318335828068, -9.358103419637847864 ) ) ;
#36995 = DIRECTION ( 'NONE',  ( 0.9609149988134837450, -0.1028163501681639419, 0.2570431154366518145 ) ) ;
#36996 = CARTESIAN_POINT ( 'NONE',  ( 68.97125867122092302, -25.93985065944693957, -5.893215200338315363 ) ) ;
#36997 = CARTESIAN_POINT ( 'NONE',  ( 111.3780948109119890, -5.574606645277164318, -18.38911715685844683 ) ) ;
#36998 = CARTESIAN_POINT ( 'NONE',  ( 122.8368814775786291, -1.561330072975668948, -17.79121239304076951 ) ) ;
#36999 = ORIENTED_EDGE ( 'NONE', *, *, #24038, .T. ) ;
#37000 = EDGE_CURVE ( 'NONE', #37411, #2634, #1800, .T. ) ;
#37001 = CARTESIAN_POINT ( 'NONE',  ( 123.1205148109119563, -7.643976991954077427, -18.09477374809248928 ) ) ;
#37002 = CARTESIAN_POINT ( 'NONE',  ( 115.6325948109119821, 0.2603800115204892296, -16.42320221600525088 ) ) ;
#37003 = CARTESIAN_POINT ( 'NONE',  ( 124.5954081442453116, -3.383040157471821630, -19.15922257007629170 ) ) ;
#37004 = CARTESIAN_POINT ( 'NONE',  ( 123.0637881442452937, -8.899110576539710493, -16.42337572283490132 ) ) ;
#37005 = VERTEX_POINT ( 'NONE', #25771 ) ;
#37006 = DIRECTION ( 'NONE',  ( -0.000000000000000000, -0.9284778069183718952, -0.3713878862591649677 ) ) ;
#37007 = EDGE_CURVE ( 'NONE', #4363, #32530, #16186, .T. ) ;
#37008 = EDGE_CURVE ( 'NONE', #7716, #16407, #27317, .T. ) ;
#37009 = CARTESIAN_POINT ( 'NONE',  ( 122.3263414775786373, -6.344957434206665248, -7.627207830600338134 ) ) ;
#37010 = CARTESIAN_POINT ( 'NONE',  ( 113.9875214775786532, -8.899110576539710493, -16.42337572283490132 ) ) ;
#37011 =( BOUNDED_CURVE ( )  B_SPLINE_CURVE ( 2, ( #17940, #38449, #38899, #32059, #30786, #25236, #42345, #35471, #4246, #25462, #8133 ),
 .UNSPECIFIED., .F., .T. ) 
 B_SPLINE_CURVE_WITH_KNOTS ( ( 3, 2, 2, 2, 2, 3 ),
 ( 0.04958152047947080032, 0.05000000000000000278, 0.06250000000000000000, 0.07499999999999999722, 0.08749999999999999445, 0.09595688439650540413 ),
 .UNSPECIFIED. ) 
 CURVE ( )  GEOMETRIC_REPRESENTATION_ITEM ( )  RATIONAL_B_SPLINE_CURVE ( ( 0.9950738546682840191, 0.9974516114610290085, 1.000000000000000000, 0.9238795325112869605, 1.000000000000000000, 0.9238795325112869605, 1.000000000000000000, 0.9238795325112869605, 1.000000000000000000, 0.9485006404992000206, 0.9666851417651740608 ) ) 
 REPRESENTATION_ITEM ( '' )  );
#37012 = CARTESIAN_POINT ( 'NONE',  ( 123.5176014775786228, -9.261995988541697145, -16.69588392320189030 ) ) ;
#37013 = CARTESIAN_POINT ( 'NONE',  ( 107.2182702545248105, -10.62599879583958717, -15.77991374673208469 ) ) ;
#37014 = B_SPLINE_CURVE_WITH_KNOTS ( 'NONE', 3,
 ( #31821, #31374, #10424, #32269, #1036, #42103, #34781, #38435, #145, #35226 ),
 .UNSPECIFIED., .F., .F.,
 ( 4, 3, 3, 4 ),
 ( 0.000000000000000000, 0.0001671877548681249956, 0.0003343755096277680285, 0.0006463528481650609656 ),
 .UNSPECIFIED. ) ;
#37015 = DIRECTION ( 'NONE',  ( 1.000000000000000000, 0.000000000000000000, -0.000000000000000000 ) ) ;
#37016 = VERTEX_POINT ( 'NONE', #8661 ) ;
#37017 = EDGE_CURVE ( 'NONE', #7972, #24335, #9843, .T. ) ;
#37018 = DIRECTION ( 'NONE',  ( 0.000000000000000000, 1.000000000000000000, 0.000000000000000000 ) ) ;
#37019 = CARTESIAN_POINT ( 'NONE',  ( 110.0658483795247804, -8.402594152722688392, -16.93181055722141792 ) ) ;
#37020 = CARTESIAN_POINT ( 'NONE',  ( 60.45894907855897316, -4.846173528048923096, -17.39321520033831447 ) ) ;
#37021 = EDGE_CURVE ( 'NONE', #44717, #42698, #26742, .T. ) ;
#37022 = CARTESIAN_POINT ( 'NONE',  ( 118.6391081442452986, -5.574606645277164318, -18.38911715685844683 ) ) ;
#37023 = CARTESIAN_POINT ( 'NONE',  ( 115.1220548109119761, -1.833838273342658809, -17.42832698103878286 ) ) ;
#37024 = CARTESIAN_POINT ( 'NONE',  ( 123.9584548109119737, -7.429215134363809092, -20.97079166887802160 ) ) ;
#37025 = ADVANCED_FACE ( 'NONE', ( #19827 ), #30762, .F. ) ;
#37026 = EDGE_CURVE ( 'NONE', #43860, #40595, #43317, .T. ) ;
#37027 = VERTEX_POINT ( 'NONE', #6375 ) ;
#37028 = CARTESIAN_POINT ( 'NONE',  ( 115.5566632127138575, -2.191907684172563986, -18.20049396185734025 ) ) ;
#37029 = CARTESIAN_POINT ( 'NONE',  ( 114.6115148109119986, -6.222761293078241884, -8.102969835052219238 ) ) ;
#37030 = FACE_OUTER_BOUND ( 'NONE', #31294, .T. ) ;
#37031 = CARTESIAN_POINT ( 'NONE',  ( 3.060777270043529619, -5.064559853354640317, -19.39321520033831447 ) ) ;
#37032 = CARTESIAN_POINT ( 'NONE',  ( -3.075987277002700804, -7.207016596002322473, -19.39321520033831447 ) ) ;
#37034 = CARTESIAN_POINT ( 'NONE',  ( 124.0281414775786146, -1.834011780172310813, -8.268836392978581529 ) ) ;
#37033 = CARTESIAN_POINT ( 'NONE',  ( 90.15753105894957287, -11.66076665495339881, -13.24321520033831412 ) ) ;
#37035 = CARTESIAN_POINT ( 'NONE',  ( 122.9503348109119827, -9.859900752359378018, -12.68260735090039759 ) ) ;
#37036 = ORIENTED_EDGE ( 'NONE', *, *, #39291, .T. ) ;
#37037 = CARTESIAN_POINT ( 'NONE',  ( 135.3184548109119874, -10.36826876090623450, -11.00511718064541178 ) ) ;
#37038 = CARTESIAN_POINT ( 'NONE',  ( 126.9733055311793066, 0.2194708681666166783, -15.14682149785671150 ) ) ;
#37039 = CARTESIAN_POINT ( 'NONE',  ( 109.9269421295247753, -9.868328341294093420, -13.39321520033831447 ) ) ;
#37040 = CARTESIAN_POINT ( 'NONE',  ( 124.9924948109119924, -5.574606645277164318, -18.38911715685844683 ) ) ;
#37041 = CARTESIAN_POINT ( 'NONE',  ( 118.4689281442453250, -10.15424416112533912, -14.75197769757731336 ) ) ;
#37042 = CARTESIAN_POINT ( 'NONE',  ( 125.0660727672603372, 1.224322542308768247, -17.79270567365541567 ) ) ;
#37043 = CARTESIAN_POINT ( 'NONE',  ( 112.7745202545247878, 0.1403307496149616695, -11.32035403202665336 ) ) ;
#37044 = FACE_OUTER_BOUND ( 'NONE', #6924, .T. ) ;
#37045 = CARTESIAN_POINT ( 'NONE',  ( 70.36267391504962632, -5.685877709920933221, -7.393215200338315363 ) ) ;
#37046 = CARTESIAN_POINT ( 'NONE',  ( 114.3846081442453197, 0.4262465694468514643, -12.03445270309931736 ) ) ;
#37047 = CARTESIAN_POINT ( 'NONE',  ( 109.9269421295247753, 0.8980012041604618078, -13.39321520033831447 ) ) ;
#37048 = CARTESIAN_POINT ( 'NONE',  ( -13.73291115513471716, -3.820450301670890614, -18.35493171628743170 ) ) ;
#37049 = CARTESIAN_POINT ( 'NONE',  ( 115.1359265045248605, -7.250697342233347165, -19.15521520033831138 ) ) ;
#37050 = CARTESIAN_POINT ( 'NONE',  ( 122.2696148109119889, -4.089484607189486809, -7.948022111789456723 ) ) ;
#37051 = CARTESIAN_POINT ( 'NONE',  ( 121.8725281442453223, -3.383040157471821630, -19.15922257007629170 ) ) ;
#37052 = CARTESIAN_POINT ( 'NONE',  ( 119.7285448082055836, -0.1020945015694968705, -15.74893487844867757 ) ) ;
#37053 = CARTESIAN_POINT ( 'NONE',  ( 115.5191414775786569, -3.383040157471821630, -19.15922257007629170 ) ) ;
#37054 = CARTESIAN_POINT ( 'NONE',  ( 113.9875214775786532, -0.4660016031367893996, -10.09054647747474043 ) ) ;
#37055 = VERTEX_POINT ( 'NONE', #30310 ) ;
#37056 = CARTESIAN_POINT ( 'NONE',  ( 113.1933481442453058, -5.574606645277164318, -18.38911715685844683 ) ) ;
#37057 = CARTESIAN_POINT ( 'NONE',  ( 112.5693548109119888, 0.4262465694468514643, -12.03445270309931736 ) ) ;
#37058 = CARTESIAN_POINT ( 'NONE',  ( 118.5823814775786360, -1.834011780172310813, -8.268836392978581529 ) ) ;
#37059 = CARTESIAN_POINT ( 'NONE',  ( 125.1059481442452750, -1.833838273342660141, -17.42832698103878286 ) ) ;
#37060 = CARTESIAN_POINT ( 'NONE',  ( 111.4915481442453142, -1.833838273342658365, -17.42832698103878286 ) ) ;
#37061 = ORIENTED_EDGE ( 'NONE', *, *, #40924, .F. ) ;
#37062 = CARTESIAN_POINT ( 'NONE',  ( 116.7104014775786425, -8.899110576539710493, -16.42337572283490132 ) ) ;
#37063 = CARTESIAN_POINT ( 'NONE',  ( 124.9357681442453014, -1.834011780172310813, -8.268836392978581529 ) ) ;
#37064 = CARTESIAN_POINT ( 'NONE',  ( 109.3018640045248304, -10.62599879583958717, -11.00651665394454604 ) ) ;
#37065 = CARTESIAN_POINT ( 'NONE',  ( 121.2485348109119769, -8.899110576539710493, -16.42337572283490132 ) ) ;
#37066 = CARTESIAN_POINT ( 'NONE',  ( 116.8240514920784818, -1.666881267585053283, -17.53180210756796598 ) ) ;
#37067 = CARTESIAN_POINT ( 'NONE',  ( 124.2951576481213607, -2.395992375830759524, -17.92872468182853396 ) ) ;
#37068 = ORIENTED_EDGE ( 'NONE', *, *, #35889, .T. ) ;
#37069 = VECTOR ( 'NONE', #17435, 1000.000000000000227 ) ;
#37070 = EDGE_CURVE ( 'NONE', #42191, #41162, #27121, .T. ) ;
#37071 = CARTESIAN_POINT ( 'NONE',  ( 122.4521266859119635, -9.033780868592240054, -16.85052413769862056 ) ) ;
#37072 = CARTESIAN_POINT ( 'NONE',  ( 124.7088614775786226, 0.2603800115204892296, -16.42320221600525088 ) ) ;
#37073 = DIRECTION ( 'NONE',  ( -0.000000000000000000, -0.9284778069183718952, -0.3713878862591649677 ) ) ;
#37074 = DIRECTION ( 'NONE',  ( -1.000000000000000000, 1.091021054073464066E-15, 0.000000000000000000 ) ) ;
#37075 = CARTESIAN_POINT ( 'NONE',  ( 122.7299391859119737, -8.844754642576873493, -8.592115655440052180 ) ) ;
#37076 = DIRECTION ( 'NONE',  ( 0.000000000000000000, -0.3818493186865927203, 0.9242245927363029745 ) ) ;
#37077 = CARTESIAN_POINT ( 'NONE',  ( 108.4684265045248424, -2.791137627527939813, -8.388885654883777576 ) ) ;
#37078 = DIRECTION ( 'NONE',  ( 1.000000000000000000, 0.000000000000000000, -0.000000000000000000 ) ) ;
#37079 = CARTESIAN_POINT ( 'NONE',  ( 137.0714388877963188, -6.662488778310335036, -18.49593449032493808 ) ) ;
#37080 = CARTESIAN_POINT ( 'NONE',  ( 9.052690036452151645, -4.182915634381243919, -19.39321520033831447 ) ) ;
#37081 = CARTESIAN_POINT ( 'NONE',  ( 125.8433948109119456, -1.834011780172310813, -8.268836392978581529 ) ) ;
#37082 = CARTESIAN_POINT ( 'NONE',  ( 118.6958348109119754, -3.505236298600246325, -18.68346056562440793 ) ) ;
#37083 = LINE ( 'NONE', #20008, #37896 ) ;
#37084 = ORIENTED_EDGE ( 'NONE', *, *, #39891, .F. ) ;
#37085 = CARTESIAN_POINT ( 'NONE',  ( 124.4252281442452812, -9.261995988541697145, -16.69588392320189030 ) ) ;
#37086 = ADVANCED_FACE ( 'NONE', ( #3173 ), #20731, .F. ) ;
#37087 = CARTESIAN_POINT ( 'NONE',  ( 116.1998614775786507, -10.63000616557722466, -14.87417383870573495 ) ) ;
#37088 = CARTESIAN_POINT ( 'NONE',  ( 116.3860827545247787, -6.936859964151250502, -8.388885654883777576 ) ) ;
#37089 = CARTESIAN_POINT ( 'NONE',  ( 112.6260814775786514, -0.8288870151387760510, -10.36305467784173118 ) ) ;
#37090 = CARTESIAN_POINT ( 'NONE',  ( 122.8936081442453059, -9.565557343593413364, -10.61323700422348004 ) ) ;
#37091 = CARTESIAN_POINT ( 'NONE',  ( 124.6521348109119884, -1.561330072975668948, -17.79121239304076951 ) ) ;
#37092 = CARTESIAN_POINT ( 'NONE',  ( 114.7192077545248594, -7.250697342233347165, -7.631215200338321125 ) ) ;
#37093 = CARTESIAN_POINT ( 'NONE',  ( 108.8851452545248151, -9.868328341294098749, -15.46607636864997204 ) ) ;
#37094 = CARTESIAN_POINT ( 'NONE',  ( 83.46578503091454593, -32.14527012763957714, -23.68292775665955574 ) ) ;
#37095 = CARTESIAN_POINT ( 'NONE',  ( 118.1285681442453068, -2.084020599724406786, -8.691656652584148546 ) ) ;
#37096 = CARTESIAN_POINT ( 'NONE',  ( 116.5402214775786405, -9.565557343593413364, -10.61323700422348004 ) ) ;
#37097 = AXIS2_PLACEMENT_3D ( 'NONE', #18035, #28303, #38 ) ;
#37098 = DIRECTION ( 'NONE',  ( 0.000000000000000000, 1.000000000000000000, 1.195183497228115774E-16 ) ) ;
#37099 = CARTESIAN_POINT ( 'NONE',  ( 111.8021765045248372, -2.791137627527939813, -8.388885654883777576 ) ) ;
#37100 = ORIENTED_EDGE ( 'NONE', *, *, #35889, .F. ) ;
#37101 = DIRECTION ( 'NONE',  ( 0.000000000000000000, -0.6004852223388321697, 0.7996358532186280677 ) ) ;
#37102 = CARTESIAN_POINT ( 'NONE',  ( 126.5808414775786446, -9.859900752359378018, -12.68260735090039759 ) ) ;
#37103 = CARTESIAN_POINT ( 'NONE',  ( 119.1878298109119783, -7.200787124940443817, -17.81845355600750835 ) ) ;
#37104 = CARTESIAN_POINT ( 'NONE',  ( 121.5492360609119800, -3.387241619883791355, -18.17469012370385073 ) ) ;
#37105 = B_SPLINE_CURVE_WITH_KNOTS ( 'NONE', 3,
 ( #32816, #43553, #40130, #8895, #36471, #23254, #19834, #33721, #22568, #22793, #43328, #40586, #12547, #22350, #36687, #2491, #40356, #5457, #36244, #1586, #9345, #12096, #12773, #9120, #5682, #19376, #2038, #33265, #29189, #43101, #26001, #5238, #5011, #15963, #29866, #43782, #23022, #36911, #12321, #18928, #19154, #15507, #11871, #15736, #25775, #39682, #19601, #26674, #37138 ),
 .UNSPECIFIED., .F., .F.,
 ( 4, 2, 2, 1, 2, 2, 2, 2, 1, 2, 2, 2, 2, 2, 2, 2, 1, 2, 2, 2, 2, 2, 2, 2, 2, 4 ),
 ( 0.000000000000000000, 0.06250000000003677614, 0.09375000000004964085, 0.1093750000000515560, 0.1171875000000521388, 0.1250000000000527078, 0.1875000000000492106, 0.2187500000000477396, 0.2343750000000468792, 0.2421875000000479616, 0.2500000000000490719, 0.3125000000000444089, 0.3437500000000421330, 0.3750000000000398015, 0.4375000000000360822, 0.4687500000000349720, 0.4843750000000360267, 0.4921875000000336398, 0.5000000000000311973, 0.6250000000000193179, 0.6875000000000134337, 0.7187500000000103251, 0.7500000000000073275, 0.8125000000000028866, 0.8749999999999984457, 1.000000000000000000 ),
 .UNSPECIFIED. ) ;
#37106 = ORIENTED_EDGE ( 'NONE', *, *, #32785, .F. ) ;
#37107 = CARTESIAN_POINT ( 'NONE',  ( 59.75121349346655109, -13.58877957849837692, -19.38162691376808411 ) ) ;
#37108 = CARTESIAN_POINT ( 'NONE',  ( 111.4886568738142074, -1.282328013897791052, -16.91375541185598053 ) ) ;
#37109 = ORIENTED_EDGE ( 'NONE', *, *, #13941, .T. ) ;
#37110 = CARTESIAN_POINT ( 'NONE',  ( 117.5613014775786525, 0.9020085738987339008, -11.91225656197089222 ) ) ;
#37111 = AXIS2_PLACEMENT_3D ( 'NONE', #31027, #38091, #17140 ) ;
#37112 = CARTESIAN_POINT ( 'NONE',  ( 124.8223148109119762, -10.15424416112533912, -14.75197769757731336 ) ) ;
#37113 = CARTESIAN_POINT ( 'NONE',  ( 114.1009748109119784, -5.574606645277164318, -18.38911715685844683 ) ) ;
#37114 = CIRCLE ( 'NONE', #32749, 2.999999999999999556 ) ;
#37115 = CARTESIAN_POINT ( 'NONE',  ( 67.30914723170953096, -51.38023326212514519, -34.64943124715581035 ) ) ;
#37116 = CARTESIAN_POINT ( 'NONE',  ( 121.5321681442453183, -9.988377603198976828, -10.36322818467138340 ) ) ;
#37117 = CARTESIAN_POINT ( 'NONE',  ( 112.9664414775786412, 0.5811942927096154232, -14.16772938898807155 ) ) ;
#37118 = CARTESIAN_POINT ( 'NONE',  ( 112.2883483795247770, -8.402594152722688392, -16.93181055722141792 ) ) ;
#37119 = CARTESIAN_POINT ( 'NONE',  ( 124.9357681442453014, -1.834011780172310813, -8.268836392978581529 ) ) ;
#37120 = CARTESIAN_POINT ( 'NONE',  ( 88.46631044337289040, -26.75858941326842810, -11.54476601486570964 ) ) ;
#37121 = ORIENTED_EDGE ( 'NONE', *, *, #6437, .T. ) ;
#37122 = CARTESIAN_POINT ( 'NONE',  ( 114.8951481442453115, -0.4660016031367893996, -10.09054647747474043 ) ) ;
#37123 = CARTESIAN_POINT ( 'NONE',  ( 114.2144281442453178, -1.833838273342658809, -17.42832698103878286 ) ) ;
#37124 = CARTESIAN_POINT ( 'NONE',  ( 126.6211808763464717, -4.842587725348250771, -18.59472652668980430 ) ) ;
#37125 = CARTESIAN_POINT ( 'NONE',  ( 113.5904348109119866, -7.893985811506177619, -18.51759400769804742 ) ) ;
#37126 = ORIENTED_EDGE ( 'NONE', *, *, #238, .F. ) ;
#37127 = CARTESIAN_POINT ( 'NONE',  ( 123.4608748109119745, -10.63000616557722466, -14.87417383870573495 ) ) ;
#37128 = CIRCLE ( 'NONE', #8731, 2.000000000000000444 ) ;
#37129 = CARTESIAN_POINT ( 'NONE',  ( 63.69189222814998175, -69.76310523276724496, -16.89321520033831447 ) ) ;
#37130 = CARTESIAN_POINT ( 'NONE',  ( 116.0113955643466852, -1.244021962887374544, -16.96476564598603076 ) ) ;
#37131 = CARTESIAN_POINT ( 'NONE',  ( 77.83157470812513168, -57.29119719338378047, -1.256939079640419843 ) ) ;
#37132 = CARTESIAN_POINT ( 'NONE',  ( 115.0086014775786509, -5.574606645277164318, -18.38911715685844683 ) ) ;
#37133 = CARTESIAN_POINT ( 'NONE',  ( 123.5140266804501152, -4.146825303465054624, -15.59726675418158948 ) ) ;
#37134 = CARTESIAN_POINT ( 'NONE',  ( 115.0653281442453277, -3.505236298600246325, -18.68346056562440793 ) ) ;
#37135 = DIRECTION ( 'NONE',  ( 1.000000000000000000, 0.000000000000000000, -0.000000000000000000 ) ) ;
#37136 = AXIS2_PLACEMENT_3D ( 'NONE', #29409, #43321, #29633 ) ;
#37137 = EDGE_CURVE ( 'NONE', #36279, #34725, #44797, .T. ) ;
#37138 = CARTESIAN_POINT ( 'NONE',  ( 123.9584548109119737, -3.874292970208447873, -21.33175929725637587 ) ) ;
#37139 = CARTESIAN_POINT ( 'NONE',  ( 115.9729548109119861, -3.505236298600246325, -18.68346056562440793 ) ) ;
#37140 = CARTESIAN_POINT ( 'NONE',  ( 117.1074881442453233, -10.63000616557722466, -14.87417383870573495 ) ) ;
#37141 = CARTESIAN_POINT ( 'NONE',  ( 124.2579079359120016, -4.360204210389833968, -8.000047426360245240 ) ) ;
#37142 = CARTESIAN_POINT ( 'NONE',  ( 125.7866681442452688, -8.899110576539710493, -16.42337572283490132 ) ) ;
#37143 = CARTESIAN_POINT ( 'NONE',  ( 115.1787814775786387, -0.1624402480850797581, -16.17319339645315424 ) ) ;
#37144 = CARTESIAN_POINT ( 'NONE',  ( 123.0637881442452937, -0.4660016031367893996, -10.09054647747474043 ) ) ;
#37145 = CARTESIAN_POINT ( 'NONE',  ( 123.2339681442453241, -6.344957434206665248, -7.627207830600338134 ) ) ;
#37146 = ORIENTED_EDGE ( 'NONE', *, *, #33755, .F. ) ;
#37147 = CARTESIAN_POINT ( 'NONE',  ( 113.6079577545248043, -7.250697342233347165, -7.631215200338321125 ) ) ;
#37148 = CARTESIAN_POINT ( 'NONE',  ( 27.78057335388972504, -13.48551096636548330, -17.89321520033831447 ) ) ;
#37149 = CARTESIAN_POINT ( 'NONE',  ( 87.44708369096655076, -22.59602017601539359, -8.393215200338321580 ) ) ;
#37150 = CARTESIAN_POINT ( 'NONE',  ( 64.34483944462449756, -36.50333010661785238, -5.615903718745205886 ) ) ;
#37151 = CARTESIAN_POINT ( 'NONE',  ( 120.5110881442453206, -6.344957434206665248, -7.627207830600338134 ) ) ;
#37152 = ORIENTED_EDGE ( 'NONE', *, *, #22385, .F. ) ;
#37153 = CARTESIAN_POINT ( 'NONE',  ( 61.76986277844709861, -39.32091226840162079, -7.393215200338315363 ) ) ;
#37154 = LINE ( 'NONE', #6618, #39440 ) ;
#37155 = CARTESIAN_POINT ( 'NONE',  ( 112.7395348109119766, -4.153390946401321671, -8.397313243818183892 ) ) ;
#37156 = CARTESIAN_POINT ( 'NONE',  ( 105.0652233795248378, -1.325403438956436419, -9.854619843455211026 ) ) ;
#37157 = CARTESIAN_POINT ( 'NONE',  ( 119.0361948109119652, -7.893985811506177619, -18.51759400769804742 ) ) ;
#37158 = CARTESIAN_POINT ( 'NONE',  ( 114.8581140045248361, 0.1403307496149616695, -15.46607636864997204 ) ) ;
#37159 = CARTESIAN_POINT ( 'NONE',  ( 119.2654641868944765, -2.239543233855044058, -18.13706010537467606 ) ) ;
#37160 = VERTEX_POINT ( 'NONE', #24157 ) ;
#37161 = CARTESIAN_POINT ( 'NONE',  ( 110.5290004229301815, 0.1075849324168598464, -14.64321520033829671 ) ) ;
#37162 = CARTESIAN_POINT ( 'NONE',  ( 123.3474214775786209, -0.1624402480850797581, -16.17319339645315424 ) ) ;
#37163 = CARTESIAN_POINT ( 'NONE',  ( 119.4332814775786318, -0.4660016031367893996, -10.09054647747474043 ) ) ;
#37164 = VECTOR ( 'NONE', #42123, 1000.000000000000000 ) ;
#37165 = EDGE_CURVE ( 'NONE', #13294, #14242, #10032, .T. ) ;
#37166 = CARTESIAN_POINT ( 'NONE',  ( 114.5547881442453217, -4.153390946401321671, -8.397313243818183892 ) ) ;
#37167 = CARTESIAN_POINT ( 'NONE',  ( 116.8238548109119819, -4.089484607189486809, -7.948022111789456723 ) ) ;
#37168 = CARTESIAN_POINT ( 'NONE',  ( 117.9382968734310992, -1.223627541775731631, -16.99192386690444323 ) ) ;
#37169 = CARTESIAN_POINT ( 'NONE',  ( 126.2184548109090940, -8.862178061931365036, -16.39564131203211517 ) ) ;
#37170 = CARTESIAN_POINT ( 'NONE',  ( 118.8092881442453290, -0.1624402480850797581, -16.17319339645315424 ) ) ;
#37171 = VERTEX_POINT ( 'NONE', #9340 ) ;
#37172 = CARTESIAN_POINT ( 'NONE',  ( 119.8870948109119752, -9.261995988541704250, -16.69588392320187964 ) ) ;
#37173 = VECTOR ( 'NONE', #23629, 1000.000000000000000 ) ;
#37174 = CARTESIAN_POINT ( 'NONE',  ( 114.9518748109119883, -1.834011780172310813, -8.268836392978581529 ) ) ;
#37175 = CARTESIAN_POINT ( 'NONE',  ( 120.9081748109119872, -4.153390946401325223, -8.397313243818185668 ) ) ;
#37176 = ORIENTED_EDGE ( 'NONE', *, *, #42558, .F. ) ;
#37177 = VECTOR ( 'NONE', #26673, 1000.000000000000000 ) ;
#37178 = CARTESIAN_POINT ( 'NONE',  ( 123.9800954359119771, 0.5291689781388270175, -13.89700978578772705 ) ) ;
#37179 = CARTESIAN_POINT ( 'NONE',  ( 117.1074881442453233, -10.63000616557722466, -14.87417383870573495 ) ) ;
#37180 = CARTESIAN_POINT ( 'NONE',  ( 113.0523327545247838, -2.477300249445798297, -19.15521520033831138 ) ) ;
#37181 = CARTESIAN_POINT ( 'NONE',  ( 115.8595014775786609, -7.643976991954077427, -18.09477374809248928 ) ) ;
#37182 = ORIENTED_EDGE ( 'NONE', *, *, #3077, .T. ) ;
#37183 = ORIENTED_EDGE ( 'NONE', *, *, #15266, .F. ) ;
#37184 = CARTESIAN_POINT ( 'NONE',  ( 125.3328548109119964, -0.8288870151387760510, -10.36305467784173118 ) ) ;
#37185 = CARTESIAN_POINT ( 'NONE',  ( 120.4543614775786295, -5.574606645277164318, -18.38911715685844683 ) ) ;
#37186 = CARTESIAN_POINT ( 'NONE',  ( -7.917624645353497748, -12.21642755857638818, -19.39321520033831447 ) ) ;
#37187 = EDGE_LOOP ( 'NONE', ( #22631, #5717, #22558, #13373 ) ) ;
#37188 = CARTESIAN_POINT ( 'NONE',  ( 117.6747548109119919, -1.834011780172310813, -8.268836392978581529 ) ) ;
#37189 = CARTESIAN_POINT ( 'NONE',  ( 106.3153796295248412, -4.863998795839590272, -19.15521520033831493 ) ) ;
#37190 = CONICAL_SURFACE ( 'NONE', #32830, 2.000000000000000444, 0.9599310885968830309 ) ;
#37191 = CARTESIAN_POINT ( 'NONE',  ( 121.3052614775786111, -1.834011780172310813, -8.268836392978581529 ) ) ;
#37193 = CARTESIAN_POINT ( 'NONE',  ( 120.1707281442453166, -9.565557343593413364, -10.61323700422348004 ) ) ;
#37192 = CARTESIAN_POINT ( 'NONE',  ( 115.1787814775786387, -9.988377603198976828, -10.36322818467138340 ) ) ;
#37194 =( BOUNDED_SURFACE ( )  B_SPLINE_SURFACE ( 1, 2, ( 
 ( #1107, #29379, #15025, #28935, #43291, #12061, #25962, #39868, #42843, #8633, #36430, #15243, #5198, #29151, #11603, #19117, #8183, #25514, #22092, #35979, #9085, #33908, #19795, #9768, #22987, #12287, #37335, #33679, #2909, #5427, #16839, #26185, #19344, #40093, #40551, #41014, #44205, #2455, #2679, #27092, #26637, #20026, #12735, #23679, #30058, #16153, #36877, #23450, #16610, #33231, #40777, #30279, #16377, #30732, #6106, #13191, #19567, #8853, #2224, #37569, #22754, #2004, #5873, #30503, #44424, #36654, #12966, #9311, #15930, #26862, #6338, #20254, #43971, #34140, #29828, #43744, #23220, #37099, #12513, #26411, #9534, #40321, #5647, #33445, #28217, #30957, #35244, #17719, #10662, #17943, #31175, #38452, #37790, #4021, #27547, #10884, #17285, #45096, #7013, #34361, #14298, #34582, #42124, #24567, #38019, #24782, #38232, #14076, #44655, #31617, #7223, #38673, #7440, #3143, #13418, #44881, #17492, #21136, #13637, #21361, #3365, #35011, #3793, #27322, #41238, #9998, #23907, #386, #10218, #6564, #20481, #31390, #6795, #17064, #41459, #24126, #20704, #13853, #27767, #41681, #24347, #10442, #20923, #34797, #3579, #160, #27994, #41899, #830, #14750, #32292, #11329, #18836, #42797, #8355, #14972, #39594, #15422, #1502, #1056, #4479 ),
 ( #28884, #31842, #35931, #36153, #22259, #35704, #4922, #32728, #4249, #21810, #18399, #29327, #43241, #11558, #8136, #5146, #18166, #25465, #39369, #22037, #32063, #28662, #42567, #4698, #25687, #12006, #25909, #611, #18618, #39814, #25239, #8581, #32509, #1284, #22481, #15195, #21587, #29100, #43011, #14522, #36375, #11780, #28435, #42348, #11106, #25008, #38902, #39138, #7673, #35475, #7903, #26359, #29551, #5377, #27039, #12458, #19063, #32947, #36602, #43916, #44150, #12915, #26584, #40956, #40722, #12685, #33622, #33172, #1949, #19516, #43682, #6045, #30000, #9480, #2167, #26811, #2625, #33856, #33393, #36823, #40034, #19294, #16327, #12233, #37510, #16095, #8799, #40497, #9258, #23168, #19968, #40266, #22704, #23392, #15875, #1724, #37047, #15646, #29772, #16558, #30453, #9033, #5818, #19738, #2398, #22930, #5592, #30228, #44373, #37278, #13135, #9711, #23623, #43467, #26129, #14246, #44601, #23857, #13806, #13364, #9943, #17668, #34312, #17012, #41632, #3527, #3085, #3307, #6961, #27717, #17231, #34958, #37742, #42072, #24513, #17445, #24727, #37967, #113, #27269, #10830, #30903, #31564, #24074, #6743, #10388, #41182, #21081, #41412, #3746, #31339, #44825, #333, #45045, #20868, #6283, #38398, #14026, #28162, #20204, #6513 ) ),
 .UNSPECIFIED., .F., .F., .T. ) 
 B_SPLINE_SURFACE_WITH_KNOTS ( ( 2, 2 ),
 ( 3, 2, 2, 2, 2, 2, 2, 2, 2, 2, 2, 2, 2, 2, 2, 2, 2, 2, 2, 2, 2, 2, 2, 2, 2, 2, 2, 2, 2, 2, 2, 2, 2, 2, 2, 2, 2, 2, 2, 2, 2, 2, 2, 2, 2, 2, 2, 2, 2, 2, 2, 2, 2, 2, 2, 2, 2, 2, 2, 2, 2, 2, 2, 2, 2, 2, 2, 2, 2, 2, 2, 2, 2, 2, 2, 2, 2, 2, 2, 2, 3 ),
 ( 0.000000000000000000, 1.000000000000000000 ),
 ( 0.000000000000000000, 0.01250000000000000069, 0.02500000000000000139, 0.03749999999999999861, 0.05000000000000000278, 0.06250000000000000000, 0.07499999999999999722, 0.08749999999999999445, 0.1000000000000000056, 0.1125000000000000028, 0.1250000000000000000, 0.1375000000000000111, 0.1499999999999999944, 0.1625000000000000056, 0.1749999999999999889, 0.1875000000000000000, 0.2000000000000000111, 0.2124999999999999944, 0.2250000000000000056, 0.2374999999999999889, 0.2500000000000000000, 0.2625000000000000111, 0.2750000000000000222, 0.2874999999999999778, 0.2999999999999999889, 0.3125000000000000000, 0.3250000000000000111, 0.3375000000000000222, 0.3499999999999999778, 0.3624999999999999889, 0.3750000000000000000, 0.3875000000000000111, 0.4000000000000000222, 0.4124999999999999778, 0.4249999999999999889, 0.4375000000000000000, 0.4500000000000000111, 0.4625000000000000222, 0.4749999999999999778, 0.4874999999999999889, 0.5000000000000000000, 0.5124999999999999556, 0.5250000000000000222, 0.5374999999999999778, 0.5500000000000000444, 0.5625000000000000000, 0.5749999999999999556, 0.5875000000000000222, 0.5999999999999999778, 0.6125000000000000444, 0.6250000000000000000, 0.6374999999999999556, 0.6500000000000000222, 0.6624999999999999778, 0.6750000000000000444, 0.6875000000000000000, 0.6999999999999999556, 0.7125000000000000222, 0.7249999999999999778, 0.7375000000000000444, 0.7500000000000000000, 0.7624999999999999556, 0.7750000000000000222, 0.7874999999999999778, 0.8000000000000000444, 0.8125000000000000000, 0.8249999999999999556, 0.8375000000000000222, 0.8499999999999999778, 0.8625000000000000444, 0.8750000000000000000, 0.8874999999999999556, 0.9000000000000000222, 0.9124999999999999778, 0.9250000000000000444, 0.9375000000000000000, 0.9499999999999999556, 0.9625000000000000222, 0.9749999999999999778, 0.9875000000000000444, 1.000000000000000000 ),
 .UNSPECIFIED. ) 
 GEOMETRIC_REPRESENTATION_ITEM ( )  RATIONAL_B_SPLINE_SURFACE ( (
 ( 1.000000000000000000, 0.9238795325112869605, 1.000000000000000000, 0.9238795325112869605, 1.000000000000000000, 0.9238795325112869605, 1.000000000000000000, 0.9238795325112869605, 1.000000000000000000, 0.9238795325112869605, 1.000000000000000000, 0.9238795325112869605, 1.000000000000000000, 0.9238795325112869605, 1.000000000000000000, 0.9238795325112869605, 1.000000000000000000, 0.9238795325112869605, 1.000000000000000000, 0.9238795325112869605, 1.000000000000000000, 0.9238795325112869605, 1.000000000000000000, 0.9238795325112869605, 1.000000000000000000, 0.9238795325112869605, 1.000000000000000000, 0.9238795325112869605, 1.000000000000000000, 0.9238795325112869605, 1.000000000000000000, 0.9238795325112869605, 1.000000000000000000, 0.9238795325112869605, 1.000000000000000000, 0.9238795325112869605, 1.000000000000000000, 0.9238795325112869605, 1.000000000000000000, 0.9238795325112869605, 1.000000000000000000, 0.9238795325112869605, 1.000000000000000000, 0.9238795325112869605, 1.000000000000000000, 0.9238795325112869605, 1.000000000000000000, 0.9238795325112869605, 1.000000000000000000, 0.9238795325112869605, 1.000000000000000000, 0.9238795325112869605, 1.000000000000000000, 0.9238795325112869605, 1.000000000000000000, 0.9238795325112869605, 1.000000000000000000, 0.9238795325112869605, 1.000000000000000000, 0.9238795325112869605, 1.000000000000000000, 0.9238795325112869605, 1.000000000000000000, 0.9238795325112869605, 1.000000000000000000, 0.9238795325112869605, 1.000000000000000000, 0.9238795325112869605, 1.000000000000000000, 0.9238795325112869605, 1.000000000000000000, 0.9238795325112869605, 1.000000000000000000, 0.9238795325112869605, 1.000000000000000000, 0.9238795325112869605, 1.000000000000000000, 0.9238795325112869605, 1.000000000000000000, 0.9238795325112869605, 1.000000000000000000, 0.9238795325112869605, 1.000000000000000000, 0.9238795325112869605, 1.000000000000000000, 0.9238795325112869605, 1.000000000000000000, 0.9238795325112869605, 1.000000000000000000, 0.9238795325112869605, 1.000000000000000000, 0.9238795325112869605, 1.000000000000000000, 0.9238795325112869605, 1.000000000000000000, 0.9238795325112869605, 1.000000000000000000, 0.9238795325112869605, 1.000000000000000000, 0.9238795325112869605, 1.000000000000000000, 0.9238795325112869605, 1.000000000000000000, 0.9238795325112869605, 1.000000000000000000, 0.9238795325112869605, 1.000000000000000000, 0.9238795325112869605, 1.000000000000000000, 0.9238795325112869605, 1.000000000000000000, 0.9238795325112869605, 1.000000000000000000, 0.9238795325112869605, 1.000000000000000000, 0.9238795325112869605, 1.000000000000000000, 0.9238795325112869605, 1.000000000000000000, 0.9238795325112869605, 1.000000000000000000, 0.9238795325112869605, 1.000000000000000000, 0.9238795325112869605, 1.000000000000000000, 0.9238795325112869605, 1.000000000000000000, 0.9238795325112869605, 1.000000000000000000, 0.9238795325112869605, 1.000000000000000000, 0.9238795325112869605, 1.000000000000000000, 0.9238795325112869605, 1.000000000000000000, 0.9238795325112869605, 1.000000000000000000, 0.9238795325112869605, 1.000000000000000000, 0.9238795325112869605, 1.000000000000000000, 0.9238795325112869605, 1.000000000000000000, 0.9238795325112869605, 1.000000000000000000, 0.9238795325112869605, 1.000000000000000000, 0.9238795325112869605, 1.000000000000000000, 0.9238795325112869605, 1.000000000000000000, 0.9238795325112869605, 1.000000000000000000, 0.9238795325112869605, 1.000000000000000000, 0.9238795325112869605, 1.000000000000000000, 0.9238795325112869605, 1.000000000000000000, 0.9238795325112869605, 1.000000000000000000),
 ( 1.000000000000000000, 0.9238795325112869605, 1.000000000000000000, 0.9238795325112869605, 1.000000000000000000, 0.9238795325112869605, 1.000000000000000000, 0.9238795325112869605, 1.000000000000000000, 0.9238795325112869605, 1.000000000000000000, 0.9238795325112869605, 1.000000000000000000, 0.9238795325112869605, 1.000000000000000000, 0.9238795325112869605, 1.000000000000000000, 0.9238795325112869605, 1.000000000000000000, 0.9238795325112869605, 1.000000000000000000, 0.9238795325112869605, 1.000000000000000000, 0.9238795325112869605, 1.000000000000000000, 0.9238795325112869605, 1.000000000000000000, 0.9238795325112869605, 1.000000000000000000, 0.9238795325112869605, 1.000000000000000000, 0.9238795325112869605, 1.000000000000000000, 0.9238795325112869605, 1.000000000000000000, 0.9238795325112869605, 1.000000000000000000, 0.9238795325112869605, 1.000000000000000000, 0.9238795325112869605, 1.000000000000000000, 0.9238795325112869605, 1.000000000000000000, 0.9238795325112869605, 1.000000000000000000, 0.9238795325112869605, 1.000000000000000000, 0.9238795325112869605, 1.000000000000000000, 0.9238795325112869605, 1.000000000000000000, 0.9238795325112869605, 1.000000000000000000, 0.9238795325112869605, 1.000000000000000000, 0.9238795325112869605, 1.000000000000000000, 0.9238795325112869605, 1.000000000000000000, 0.9238795325112869605, 1.000000000000000000, 0.9238795325112869605, 1.000000000000000000, 0.9238795325112869605, 1.000000000000000000, 0.9238795325112869605, 1.000000000000000000, 0.9238795325112869605, 1.000000000000000000, 0.9238795325112869605, 1.000000000000000000, 0.9238795325112869605, 1.000000000000000000, 0.9238795325112869605, 1.000000000000000000, 0.9238795325112869605, 1.000000000000000000, 0.9238795325112869605, 1.000000000000000000, 0.9238795325112869605, 1.000000000000000000, 0.9238795325112869605, 1.000000000000000000, 0.9238795325112869605, 1.000000000000000000, 0.9238795325112869605, 1.000000000000000000, 0.9238795325112869605, 1.000000000000000000, 0.9238795325112869605, 1.000000000000000000, 0.9238795325112869605, 1.000000000000000000, 0.9238795325112869605, 1.000000000000000000, 0.9238795325112869605, 1.000000000000000000, 0.9238795325112869605, 1.000000000000000000, 0.9238795325112869605, 1.000000000000000000, 0.9238795325112869605, 1.000000000000000000, 0.9238795325112869605, 1.000000000000000000, 0.9238795325112869605, 1.000000000000000000, 0.9238795325112869605, 1.000000000000000000, 0.9238795325112869605, 1.000000000000000000, 0.9238795325112869605, 1.000000000000000000, 0.9238795325112869605, 1.000000000000000000, 0.9238795325112869605, 1.000000000000000000, 0.9238795325112869605, 1.000000000000000000, 0.9238795325112869605, 1.000000000000000000, 0.9238795325112869605, 1.000000000000000000, 0.9238795325112869605, 1.000000000000000000, 0.9238795325112869605, 1.000000000000000000, 0.9238795325112869605, 1.000000000000000000, 0.9238795325112869605, 1.000000000000000000, 0.9238795325112869605, 1.000000000000000000, 0.9238795325112869605, 1.000000000000000000, 0.9238795325112869605, 1.000000000000000000, 0.9238795325112869605, 1.000000000000000000, 0.9238795325112869605, 1.000000000000000000, 0.9238795325112869605, 1.000000000000000000, 0.9238795325112869605, 1.000000000000000000, 0.9238795325112869605, 1.000000000000000000, 0.9238795325112869605, 1.000000000000000000, 0.9238795325112869605, 1.000000000000000000, 0.9238795325112869605, 1.000000000000000000, 0.9238795325112869605, 1.000000000000000000, 0.9238795325112869605, 1.000000000000000000, 0.9238795325112869605, 1.000000000000000000, 0.9238795325112869605, 1.000000000000000000) ) ) 
 REPRESENTATION_ITEM ( '' )  SURFACE ( )  );
#37195 = CARTESIAN_POINT ( 'NONE',  ( 123.6877814775786533, -6.222761293078241884, -8.102969835052219238 ) ) ;
#37196 = CARTESIAN_POINT ( 'NONE',  ( 63.74703025577719018, -40.95155355269160680, -19.39321520033831447 ) ) ;
#37197 = EDGE_LOOP ( 'NONE', ( #31865, #41686, #28117, #8733, #1218 ) ) ;
#37198 = CARTESIAN_POINT ( 'NONE',  ( 122.3263414775786373, -3.505236298600246325, -18.68346056562440793 ) ) ;
#37199 = CARTESIAN_POINT ( 'NONE',  ( 123.0637881442452937, -0.4660016031367911205, -10.09054647747473688 ) ) ;
#37200 = CARTESIAN_POINT ( 'NONE',  ( 59.44377208703740223, -12.82110557137145967, -17.39288367676203606 ) ) ;
#37201 = CARTESIAN_POINT ( 'NONE',  ( 111.7327233795247849, -8.938348069036489818, -17.46756447353520159 ) ) ;
#37202 = AXIS2_PLACEMENT_3D ( 'NONE', #4648, #15149, #15596 ) ;
#37203 = CARTESIAN_POINT ( 'NONE',  ( 114.3719421295247827, -9.868328341294093420, -13.39321520033831447 ) ) ;
#37204 = CARTESIAN_POINT ( 'NONE',  ( 113.6774108795247997, -8.938348069036489818, -9.318865927141430916 ) ) ;
#37205 = CARTESIAN_POINT ( 'NONE',  ( 122.1561614775786353, -0.4660016031367893996, -10.09054647747474043 ) ) ;
#37206 = CARTESIAN_POINT ( 'NONE',  ( 124.7088614775786226, -9.565557343593413364, -10.61323700422348004 ) ) ;
#37207 = ORIENTED_EDGE ( 'NONE', *, *, #1356, .T. ) ;
#37208 = AXIS2_PLACEMENT_3D ( 'NONE', #14604, #28524, #42429 ) ;
#37209 = CARTESIAN_POINT ( 'NONE',  ( 124.6521348109119884, -1.561330072975668948, -17.79121239304076951 ) ) ;
#37210 = CARTESIAN_POINT ( 'NONE',  ( 113.4202548109119846, 0.1319031606808879209, -14.10382304977623669 ) ) ;
#37211 = CARTESIAN_POINT ( 'NONE',  ( 105.7294421295247844, -9.051693226400931991, -21.39321520033831447 ) ) ;
#37212 = CARTESIAN_POINT ( 'NONE',  ( 119.4900081442453086, -1.834011780172310813, -8.268836392978581529 ) ) ;
#37213 = CARTESIAN_POINT ( 'NONE',  ( 119.8870948109119752, -9.261995988541697145, -16.69588392320189030 ) ) ;
#37214 = CARTESIAN_POINT ( 'NONE',  ( 64.63131511434168885, -2.693399871814762925, -18.62537188001541466 ) ) ;
#37215 = CARTESIAN_POINT ( 'NONE',  ( 123.9714148109119805, -8.899110576539710493, -16.42337572283490132 ) ) ;
#37216 = LINE ( 'NONE', #5755, #43890 ) ;
#37217 = CARTESIAN_POINT ( 'NONE',  ( 123.4244704359119709, -10.25716656981731489, -12.88942061488890545 ) ) ;
#37218 = ORIENTED_EDGE ( 'NONE', *, *, #7431, .T. ) ;
#37219 = CARTESIAN_POINT ( 'NONE',  ( 90.41915846579418314, -16.87387181286558757, -4.893215200338314474 ) ) ;
#37220 = DIRECTION ( 'NONE',  ( 0.000000000000000000, -0.3818493186865927203, 0.9242245927363029745 ) ) ;
#37221 = CARTESIAN_POINT ( 'NONE',  ( 124.8790414775786246, -8.899110576539710493, -16.42337572283490132 ) ) ;
#37222 = CARTESIAN_POINT ( 'NONE',  ( 108.3989733795247759, -1.325403438956436419, -9.854619843455211026 ) ) ;
#37223 = CARTESIAN_POINT ( 'NONE',  ( 111.0381921295247878, -9.868328341294093420, -13.39321520033831447 ) ) ;
#37224 = CARTESIAN_POINT ( 'NONE',  ( 118.3554748109119998, -9.565557343593413364, -10.61323700422348004 ) ) ;
#37225 = CARTESIAN_POINT ( 'NONE',  ( 69.23661232544138500, -26.06570555932018962, -5.871568482255425714 ) ) ;
#37226 = CARTESIAN_POINT ( 'NONE',  ( 117.2776681442452968, -4.153390946401325223, -8.397313243818185668 ) ) ;
#37227 = CARTESIAN_POINT ( 'NONE',  ( 122.6099748109119929, -9.261995988541697145, -16.69588392320189030 ) ) ;
#37228 = ORIENTED_EDGE ( 'NONE', *, *, #17337, .F. ) ;
#37229 = CARTESIAN_POINT ( 'NONE',  ( 123.6877814775786533, -6.222761293078241884, -8.102969835052219238 ) ) ;
#37230 = CARTESIAN_POINT ( 'NONE',  ( 117.2776681442452968, -5.638512984488999180, -18.83840828888717311 ) ) ;
#37231 = AXIS2_PLACEMENT_3D ( 'NONE', #29522, #12660, #12202 ) ;
#37232 = CARTESIAN_POINT ( 'NONE',  ( 124.8790414775786246, -0.4660016031367893996, -10.09054647747474043 ) ) ;
#37233 = CARTESIAN_POINT ( 'NONE',  ( 122.3263414775786373, -3.505236298600246325, -18.68346056562440793 ) ) ;
#37234 = ORIENTED_EDGE ( 'NONE', *, *, #21087, .T. ) ;
#37235 = DIRECTION ( 'NONE',  ( -1.000000000000000000, 0.000000000000000000, -0.000000000000000000 ) ) ;
#37236 = ADVANCED_FACE ( 'NONE', ( #44913 ), #17316, .T. ) ;
#37237 = CIRCLE ( 'NONE', #40159, 2.000000000000000444 ) ;
#37238 = CARTESIAN_POINT ( 'NONE',  ( 124.4252281442452812, -9.261995988541697145, -16.69588392320189030 ) ) ;
#37239 = CARTESIAN_POINT ( 'NONE',  ( 114.7249681442453237, -9.565557343593413364, -10.61323700422348004 ) ) ;
#37240 = B_SPLINE_CURVE_WITH_KNOTS ( 'NONE', 3,
 ( #1985, #18871, #29810, #26617, #40531, #6084, #16592, #17266, #20686, #37545, #40757, #30939, #44862, #37315, #24107, #34563, #2892, #45075, #27073, #6776, #41218, #9513, #16358, #3122, #26844, #2434, #37773, #6546, #20004, #33657, #40995, #13171, #33889, #23430, #30259, #13617, #30714, #20462, #3346, #31155, #37079, #34344, #13835, #27750, #16821, #23201 ),
 .UNSPECIFIED., .F., .F.,
 ( 4, 2, 2, 2, 2, 2, 2, 2, 2, 2, 2, 2, 2, 2, 2, 2, 2, 2, 2, 2, 2, 2, 4 ),
 ( 0.000000000000000000, 0.06249999999998258338, 0.09374999999996579125, 0.1249999999999489853, 0.1874999999999005518, 0.2187499999998762656, 0.2343749999998641920, 0.2499999999998521183, 0.3124999999998443467, 0.3437499999998468447, 0.3749999999998493982, 0.4374999999998543943, 0.4687499999998612776, 0.4999999999998682165, 0.6249999999998880895, 0.6874999999998981925, 0.7187499999999032996, 0.7499999999999082956, 0.8124999999999186207, 0.8437499999999280575, 0.8593749999999329425, 0.8749999999999378275, 1.000000000000000000 ),
 .UNSPECIFIED. ) ;
#37241 = CARTESIAN_POINT ( 'NONE',  ( 111.7751814775786556, -2.084020599724406786, -8.691656652584148546 ) ) ;
#37242 = CARTESIAN_POINT ( 'NONE',  ( 108.9545983795247821, -0.7896495226426338832, -9.318865927141430916 ) ) ;
#37243 = CARTESIAN_POINT ( 'NONE',  ( 123.0077516859119839, -0.6942167230862511529, -9.935906262978006609 ) ) ;
#37244 = ORIENTED_EDGE ( 'NONE', *, *, #38095, .F. ) ;
#37245 = FACE_OUTER_BOUND ( 'NONE', #42217, .T. ) ;
#37246 = CARTESIAN_POINT ( 'NONE',  ( 111.2465515045248168, -6.936859964151250502, -18.39754474579286025 ) ) ;
#37247 = DIRECTION ( 'NONE',  ( -1.000000000000000000, 0.000000000000000000, 0.000000000000000000 ) ) ;
#37248 = CARTESIAN_POINT ( 'NONE',  ( 121.1918081442452859, -10.15424416112533912, -14.75197769757731336 ) ) ;
#37249 = CARTESIAN_POINT ( 'NONE',  ( 115.4624148109119943, -4.153390946401321671, -8.397313243818183892 ) ) ;
#37250 = DIRECTION ( 'NONE',  ( -0.000000000000000000, -0.9284778069183721172, -0.3713878862591650232 ) ) ;
#37251 = ORIENTED_EDGE ( 'NONE', *, *, #26503, .T. ) ;
#37252 = FACE_OUTER_BOUND ( 'NONE', #42721, .T. ) ;
#37253 = CARTESIAN_POINT ( 'NONE',  ( 121.0783548109119749, -9.565557343593413364, -10.61323700422348004 ) ) ;
#37254 = CARTESIAN_POINT ( 'NONE',  ( 112.4559014775786778, -0.1624402480850797581, -16.17319339645315424 ) ) ;
#37255 = EDGE_CURVE ( 'NONE', #2056, #36383, #2714, .T. ) ;
#37257 = CIRCLE ( 'NONE', #29983, 2.999999999999999556 ) ;
#37256 = CARTESIAN_POINT ( 'NONE',  ( 66.84025912450881890, -0.06488636359980230750, -10.39321520033831625 ) ) ;
#37258 = CARTESIAN_POINT ( 'NONE',  ( 111.3319081442453182, -5.568102603702657305, -18.34339073538273013 ) ) ;
#37260 = CARTESIAN_POINT ( 'NONE',  ( 123.0637881442452937, -0.4660016031367893996, -10.09054647747474043 ) ) ;
#37259 = CARTESIAN_POINT ( 'NONE',  ( 70.32328378357757970, -26.37807398378523160, -5.615903685620933672 ) ) ;
#37261 = CARTESIAN_POINT ( 'NONE',  ( 112.5693548109119888, -10.63000616557722466, -14.87417383870573495 ) ) ;
#37262 =( REPRESENTATION_RELATIONSHIP ('NONE','NONE', #36667, #38750 ) REPRESENTATION_RELATIONSHIP_WITH_TRANSFORMATION ( #2870 )SHAPE_REPRESENTATION_RELATIONSHIP( ) );
#37263 = EDGE_LOOP ( 'NONE', ( #43225, #25377, #15125, #42641 ) ) ;
#37264 = CARTESIAN_POINT ( 'NONE',  ( 114.5104504682427802, 0.5115630086001619059, -14.64321520033831447 ) ) ;
#37265 = CARTESIAN_POINT ( 'NONE',  ( 126.6390922358748270, 0.1291732976736364169, -14.88311683621468795 ) ) ;
#37266 = B_SPLINE_CURVE_WITH_KNOTS ( 'NONE', 3,
 ( #35129, #28995, #32175, #8241, #10995, #36040, #11221, #31947, #18730, #25127 ),
 .UNSPECIFIED., .F., .F.,
 ( 4, 2, 2, 2, 4 ),
 ( 5.485677294651094893E-18, 0.0005882757591493389601, 0.001176551518298672282, 0.001764827277448005821, 0.002353103036597339361 ),
 .UNSPECIFIED. ) ;
#37267 = CARTESIAN_POINT ( 'NONE',  ( 107.2877233795247776, -1.325403438956436419, -9.854619843455211026 ) ) ;
#37268 = EDGE_CURVE ( 'NONE', #14703, #30187, #2798, .T. ) ;
#37269 = CARTESIAN_POINT ( 'NONE',  ( 126.1270281442452870, 0.1319031606808879209, -14.10382304977623669 ) ) ;
#37270 = CARTESIAN_POINT ( 'NONE',  ( 120.8514481442452961, -2.084020599724406786, -8.691656652584148546 ) ) ;
#37271 = EDGE_CURVE ( 'NONE', #43627, #12584, #14105, .T. ) ;
#37272 = DIRECTION ( 'NONE',  ( -0.2768435750659241079, -0.3568721902840695792, 0.8921882507333129819 ) ) ;
#37273 = CARTESIAN_POINT ( 'NONE',  ( 113.6079577545248043, -2.791137627527939813, -18.39754474579286025 ) ) ;
#37274 = CONICAL_SURFACE ( 'NONE', #44597, 2.445500000000004448, 0.9599310885968757034 ) ;
#37275 = CARTESIAN_POINT ( 'NONE',  ( 85.15861813568058380, -25.99489077589524300, -13.39321520033831625 ) ) ;
#37276 = CARTESIAN_POINT ( 'NONE',  ( 120.1601735609119856, -9.645473719204776586, -14.86997237629376656 ) ) ;
#37277 = CARTESIAN_POINT ( 'NONE',  ( 114.3278814775786429, 0.1319031606808879209, -14.10382304977623669 ) ) ;
#37278 = CARTESIAN_POINT ( 'NONE',  ( 109.0240515045248202, -2.477300249445798297, -7.631215200338321125 ) ) ;
#37279 = CARTESIAN_POINT ( 'NONE',  ( 117.5613014775786525, 0.9020085738987385637, -11.91225656197091887 ) ) ;
#37280 = CARTESIAN_POINT ( 'NONE',  ( 114.1635827545248389, -2.477300249445798297, -19.15521520033831138 ) ) ;
#37281 = CARTESIAN_POINT ( 'NONE',  ( 124.0281414775786146, -1.834011780172310813, -8.268836392978581529 ) ) ;
#37282 = CARTESIAN_POINT ( 'NONE',  ( 122.8368814775786291, -1.561330072975668948, -17.79121239304076951 ) ) ;
#37283 = CARTESIAN_POINT ( 'NONE',  ( 115.4451630180080883, 0.7607806665037644134, -14.64321520033834467 ) ) ;
#37284 = CARTESIAN_POINT ( 'NONE',  ( 115.9162281442453235, -4.089484607189486809, -7.948022111789456723 ) ) ;
#37285 = CARTESIAN_POINT ( 'NONE',  ( 113.8173414775786512, 0.2603800115204892296, -16.42320221600525088 ) ) ;
#37286 = EDGE_LOOP ( 'NONE', ( #27028, #38472, #28108, #2755, #39040, #7922, #13734, #2271, #21612, #36088 ) ) ;
#37287 = CARTESIAN_POINT ( 'NONE',  ( 113.5337081442453240, -0.8288870151387760510, -10.36305467784173118 ) ) ;
#37288 = CARTESIAN_POINT ( 'NONE',  ( 112.4559014775786778, -0.1624402480850797581, -16.17319339645315424 ) ) ;
#37289 = CARTESIAN_POINT ( 'NONE',  ( 118.9794681442453026, -9.261995988541697145, -16.69588392320189030 ) ) ;
#37290 = CARTESIAN_POINT ( 'NONE',  ( 115.1220548109119761, -8.166667518702817929, -8.995218007635861213 ) ) ;
#37291 = ITEM_DEFINED_TRANSFORMATION ( 'NONE', 'NONE', #19122,  #12375 ) ;
#37292 = CARTESIAN_POINT ( 'NONE',  ( 111.6050014775786536, 0.1319031606808879209, -14.10382304977623669 ) ) ;
#37293 = ORIENTED_EDGE ( 'NONE', *, *, #25630, .F. ) ;
#37294 = ADVANCED_FACE ( 'NONE', ( #17524 ), #30952, .T. ) ;
#37295 = CARTESIAN_POINT ( 'NONE',  ( 116.2565881442453133, -0.8288870151387760510, -10.36305467784173118 ) ) ;
#37296 = CARTESIAN_POINT ( 'NONE',  ( 115.7460481442453357, -10.15424416112533912, -14.75197769757731336 ) ) ;
#37297 = EDGE_CURVE ( 'NONE', #20751, #6914, #27843, .T. ) ;
#37298 = ADVANCED_FACE ( 'NONE', ( #7253 ), #18430, .T. ) ;
#37299 = VECTOR ( 'NONE', #44991, 1000.000000000000000 ) ;
#37300 = CARTESIAN_POINT ( 'NONE',  ( 109.5796765045248122, -7.250697342233347165, -19.15521520033831138 ) ) ;
#37301 = VECTOR ( 'NONE', #8961, 1000.000000000000227 ) ;
#37302 = CARTESIAN_POINT ( 'NONE',  ( 109.3018640045248304, 0.1403307496149616695, -15.46607636864997204 ) ) ;
#37303 = CARTESIAN_POINT ( 'NONE',  ( 123.6310548109119765, -4.153390946401325223, -8.397313243818185668 ) ) ;
#37304 = DIRECTION ( 'NONE',  ( 0.9609149988134837450, -0.1028163501681639419, 0.2570431154366518145 ) ) ;
#37305 = CARTESIAN_POINT ( 'NONE',  ( 116.4555358795247884, -0.7896495226426338832, -17.46756447353520159 ) ) ;
#37306 = ORIENTED_EDGE ( 'NONE', *, *, #9789, .F. ) ;
#37307 = CARTESIAN_POINT ( 'NONE',  ( 78.69189222814998175, -69.76310523276724496, -16.89321520033831447 ) ) ;
#37308 = CARTESIAN_POINT ( 'NONE',  ( 122.1561614775786353, -0.4660016031367893996, -10.09054647747474043 ) ) ;
#37309 = DIRECTION ( 'NONE',  ( 1.000000000000000000, 0.000000000000000000, -0.000000000000000000 ) ) ;
#37310 = CARTESIAN_POINT ( 'NONE',  ( 111.7751814775786556, -7.893985811506177619, -18.51759400769804742 ) ) ;
#37311 = CARTESIAN_POINT ( 'NONE',  ( 116.7696035360916227, 2.027398920889790457, -5.931029822836547005 ) ) ;
#37312 = CARTESIAN_POINT ( 'NONE',  ( 65.55689610126231059, -13.67296395165911704, -14.39321520033831625 ) ) ;
#37313 = CARTESIAN_POINT ( 'NONE',  ( 106.3153796295248412, -4.863998795839590272, -8.388885654883775800 ) ) ;
#37314 = DIRECTION ( 'NONE',  ( -0.000000000000000000, -0.9284778069183721172, -0.3713878862591650232 ) ) ;
#37315 = CARTESIAN_POINT ( 'NONE',  ( 136.5048557854543674, -4.261492763881302714, -19.10789423623526417 ) ) ;
#37316 = CARTESIAN_POINT ( 'NONE',  ( 115.7145311052981782, 0.4930828106259610433, -12.14321520033831625 ) ) ;
#37317 = CARTESIAN_POINT ( 'NONE',  ( 126.2404814775786264, -9.261995988541697145, -16.69588392320189030 ) ) ;
#37318 = CARTESIAN_POINT ( 'NONE',  ( 121.7590748109119687, -2.084020599724406786, -8.691656652584148546 ) ) ;
#37319 = CARTESIAN_POINT ( 'NONE',  ( 119.7434548109119561, -0.5813642816343631559, -16.73924225410030431 ) ) ;
#37320 = EDGE_LOOP ( 'NONE', ( #6207, #32212, #9402, #25247 ) ) ;
#37321 = CARTESIAN_POINT ( 'NONE',  ( 122.4397948109119767, -9.988377603198976828, -10.36322818467138340 ) ) ;
#37322 = CARTESIAN_POINT ( 'NONE',  ( 118.1852948109119836, -5.638512984488999180, -18.83840828888717311 ) ) ;
#37323 = DIRECTION ( 'NONE',  ( 1.387778780781445676E-17, -0.9284778069183720062, -0.3713878862591650232 ) ) ;
#37324 = CARTESIAN_POINT ( 'NONE',  ( 113.7606148109119886, -7.894159318335828068, -9.358103419637847864 ) ) ;
#37325 = CARTESIAN_POINT ( 'NONE',  ( 113.1933481442453058, -4.089484607189486809, -7.948022111789456723 ) ) ;
#37327 = CARTESIAN_POINT ( 'NONE',  ( 123.0637881442452937, -0.4660016031367893996, -10.09054647747474043 ) ) ;
#37326 = VECTOR ( 'NONE', #16907, 1000.000000000000000 ) ;
#37328 = CARTESIAN_POINT ( 'NONE',  ( 110.6909265045248247, -7.250697342233347165, -19.15521520033831138 ) ) ;
#37329 = ADVANCED_FACE ( 'NONE', ( #20952 ), #10473, .T. ) ;
#37330 = CARTESIAN_POINT ( 'NONE',  ( 61.76986277844709861, -39.32091226840162079, -21.89321520033831447 ) ) ;
#37331 = CARTESIAN_POINT ( 'NONE',  ( 124.8533330496100859, -12.49533689344159981, -14.47573569507178171 ) ) ;
#37332 = CARTESIAN_POINT ( 'NONE',  ( 116.5969481442453031, -9.859900752359374465, -12.68260735090039404 ) ) ;
#37333 = CARTESIAN_POINT ( 'NONE',  ( 116.7671281442453335, -7.643976991954077427, -18.09477374809248928 ) ) ;
#37334 = LINE ( 'NONE', #33678, #19700 ) ;
#37335 = CARTESIAN_POINT ( 'NONE',  ( 115.3442858795247759, -8.402594152722688392, -9.854619843455216355 ) ) ;
#37336 = ORIENTED_EDGE ( 'NONE', *, *, #8638, .F. ) ;
#37337 = LINE ( 'NONE', #27094, #36392 ) ;
#37338 = CARTESIAN_POINT ( 'NONE',  ( 114.2711548109119803, -9.988377603198976828, -10.36322818467138340 ) ) ;
#37339 = CARTESIAN_POINT ( 'NONE',  ( 79.39832680986421565, 5.045790854648893209, -6.299625027019903456 ) ) ;
#37340 = CARTESIAN_POINT ( 'NONE',  ( 119.3961891859119930, -1.406689858478933353, -17.56299727309130887 ) ) ;
#37341 = CARTESIAN_POINT ( 'NONE',  ( 121.7575954359119805, 0.5291689781388270175, -13.89700978578772705 ) ) ;
#37342 = VERTEX_POINT ( 'NONE', #14330 ) ;
#37343 = CARTESIAN_POINT ( 'NONE',  ( 123.4286749921664352, -2.732273803890511665, -14.98280307987510085 ) ) ;
#37344 = CARTESIAN_POINT ( 'NONE',  ( 73.07463722459043254, -60.35343162539949446, -36.44966353086839206 ) ) ;
#37345 = ORIENTED_EDGE ( 'NONE', *, *, #18214, .F. ) ;
#37346 = VECTOR ( 'NONE', #42764, 1000.000000000000114 ) ;
#37347 = CARTESIAN_POINT ( 'NONE',  ( 116.9940348109119839, -9.988377603198976828, -10.36322818467138340 ) ) ;
#37348 = CARTESIAN_POINT ( 'NONE',  ( 125.1626748109119802, -0.1624402480850797581, -16.17319339645315424 ) ) ;
#37349 = CARTESIAN_POINT ( 'NONE',  ( 117.6747548109119919, -7.643976991954077427, -18.09477374809248928 ) ) ;
#37350 = FILL_AREA_STYLE_COLOUR ( '', #18221 ) ;
#37351 = PLANE ( 'NONE',  #11140 ) ;
#37352 = CARTESIAN_POINT ( 'NONE',  ( 121.3052614775786111, -1.834011780172310813, -8.268836392978581529 ) ) ;
#37353 = CARTESIAN_POINT ( 'NONE',  ( 115.5191414775786569, -3.383040157471821630, -19.15922257007629170 ) ) ;
#37354 = EDGE_CURVE ( 'NONE', #12584, #39438, #44837, .T. ) ;
#37355 = CARTESIAN_POINT ( 'NONE',  ( 110.6909265045248247, -2.791137627527939813, -8.388885654883777576 ) ) ;
#37356 = CARTESIAN_POINT ( 'NONE',  ( 111.7184548109119788, -0.8288870151387760510, -10.36305467784173118 ) ) ;
#37357 = FILL_AREA_STYLE_COLOUR ( '', #32281 ) ;
#37358 = ORIENTED_EDGE ( 'NONE', *, *, #1650, .T. ) ;
#37359 = EDGE_CURVE ( 'NONE', #17793, #42758, #22697, .T. ) ;
#37360 = CARTESIAN_POINT ( 'NONE',  ( 118.0718414775786300, -9.261995988541697145, -16.69588392320189030 ) ) ;
#37361 = CARTESIAN_POINT ( 'NONE',  ( 113.7606148109119886, -7.894159318335828068, -9.358103419637847864 ) ) ;
#37362 = CARTESIAN_POINT ( 'NONE',  ( 126.3975136127248362, -5.074220342508069415, -18.47877043462501234 ) ) ;
#37363 = CARTESIAN_POINT ( 'NONE',  ( 112.7962614775786676, -3.383040157471821630, -19.15922257007629170 ) ) ;
#37364 = ORIENTED_EDGE ( 'NONE', *, *, #9273, .T. ) ;
#37365 = CIRCLE ( 'NONE', #14072, 5.000000000000000888 ) ;
#37366 = CARTESIAN_POINT ( 'NONE',  ( 122.0427081442452817, 0.5811942927096110934, -14.16772938898807510 ) ) ;
#37367 = DIRECTION ( 'NONE',  ( 0.000000000000000000, 0.3818493186865928868, -0.9242245927363029745 ) ) ;
#37368 = CARTESIAN_POINT ( 'NONE',  ( 113.0798948109119948, -8.899110576539710493, -16.42337572283490132 ) ) ;
#37369 = CARTESIAN_POINT ( 'NONE',  ( -7.923679509334008664, -5.078949698970065540, -19.39321520033831447 ) ) ;
#37370 = FACE_BOUND ( 'NONE', #16039, .T. ) ;
#37371 = CARTESIAN_POINT ( 'NONE',  ( 116.9940348109119839, -0.1624402480850797581, -16.17319339645315424 ) ) ;
#37372 = CARTESIAN_POINT ( 'NONE',  ( 137.3802547664384122, -3.523273223278070354, -8.431451416491041684 ) ) ;
#37373 = CARTESIAN_POINT ( 'NONE',  ( 117.9583881442453048, 0.1319031606808879209, -14.10382304977623669 ) ) ;
#37374 = FACE_OUTER_BOUND ( 'NONE', #8228, .T. ) ;
#37375 = AXIS2_PLACEMENT_3D ( 'NONE', #14318, #20502, #17084 ) ;
#37376 = DIRECTION ( 'NONE',  ( -1.000000000000000000, 0.000000000000000000, -0.000000000000000000 ) ) ;
#37377 = CARTESIAN_POINT ( 'NONE',  ( 116.7104014775786425, -8.899110576539710493, -16.42337572283490132 ) ) ;
#37378 = CARTESIAN_POINT ( 'NONE',  ( 117.3343948109119737, -3.383040157471821630, -19.15922257007629170 ) ) ;
#37379 = CARTESIAN_POINT ( 'NONE',  ( 123.4939235609119663, -9.645473719204776586, -14.86997237629376656 ) ) ;
#37380 = CARTESIAN_POINT ( 'NONE',  ( 112.7962614775786676, -3.383040157471821630, -19.15922257007629170 ) ) ;
#37381 = CARTESIAN_POINT ( 'NONE',  ( 116.1431348109119881, 0.1319031606808879209, -14.10382304977623669 ) ) ;
#37382 = CARTESIAN_POINT ( 'NONE',  ( 121.5888948109119809, -10.30919188438810075, -12.61870101168855918 ) ) ;
#37383 = CARTESIAN_POINT ( 'NONE',  ( 115.4056881442453459, -2.084020599724406786, -8.691656652584148546 ) ) ;
#37384 = ORIENTED_EDGE ( 'NONE', *, *, #19307, .F. ) ;
#37385 = CARTESIAN_POINT ( 'NONE',  ( 113.7606148109119886, -1.561330072975668060, -17.79121239304076596 ) ) ;
#37386 = CARTESIAN_POINT ( 'NONE',  ( 112.0105358795247810, -0.7896495226426338832, -17.46756447353520159 ) ) ;
#37387 = CARTESIAN_POINT ( 'NONE',  ( 89.40092984481313465, -25.38011337280982715, -14.88121679464376257 ) ) ;
#37388 = CARTESIAN_POINT ( 'NONE',  ( 84.10862215250544693, -25.38011337280982715, -14.88121679464376257 ) ) ;
#37389 = CARTESIAN_POINT ( 'NONE',  ( 127.9950210827190631, -4.139185286760726612, -15.60733003398113361 ) ) ;
#37390 = CARTESIAN_POINT ( 'NONE',  ( 120.0005481442453146, -5.638512984488999180, -18.83840828888717311 ) ) ;
#37391 = ORIENTED_EDGE ( 'NONE', *, *, #25429, .T. ) ;
#37392 = CARTESIAN_POINT ( 'NONE',  ( 126.0135748109119902, -8.166667518702819706, -8.995218007635861213 ) ) ;
#37393 = CARTESIAN_POINT ( 'NONE',  ( 125.0492214775786266, -6.344957434206642155, -7.627207830600332805 ) ) ;
#37394 = CARTESIAN_POINT ( 'NONE',  ( 115.9162281442453235, -5.574606645277164318, -18.38911715685844683 ) ) ;
#37395 = CARTESIAN_POINT ( 'NONE',  ( 124.3685014775786186, 0.4262465694468523525, -12.03445270309933690 ) ) ;
#37396 = ADVANCED_FACE ( 'NONE', ( #10692 ), #28244, .F. ) ;
#37397 = CARTESIAN_POINT ( 'NONE',  ( 124.6521348109119884, -1.561330072975668948, -17.79121239304076951 ) ) ;
#37398=STYLED_ITEM('',(#45190),#21657);
#37399 = CARTESIAN_POINT ( 'NONE',  ( 114.7192077545248594, -2.791137627527939813, -18.39754474579286025 ) ) ;
#37400 = CARTESIAN_POINT ( 'NONE',  ( 70.19189222814998175, -64.81574766768041229, -39.12908228425553858 ) ) ;
#37401 = VERTEX_POINT ( 'NONE', #35505 ) ;
#37402 = CARTESIAN_POINT ( 'NONE',  ( 112.5693548109119888, -10.63000616557722466, -14.87417383870573495 ) ) ;
#37403 = CARTESIAN_POINT ( 'NONE',  ( 123.1772414775786189, -5.574606645277164318, -18.38911715685844683 ) ) ;
#37404 = VECTOR ( 'NONE', #31725, 1000.000000000000000 ) ;
#37405 = CARTESIAN_POINT ( 'NONE',  ( 119.4900081442453086, -1.834011780172310813, -8.268836392978581529 ) ) ;
#37406 = CARTESIAN_POINT ( 'NONE',  ( 113.4769814775786330, 0.4262465694468514643, -12.03445270309931736 ) ) ;
#37407 = CARTESIAN_POINT ( 'NONE',  ( 116.3700414775786527, -5.638512984488999180, -18.83840828888717311 ) ) ;
#37408 = FACE_OUTER_BOUND ( 'NONE', #18974, .T. ) ;
#37409 = CARTESIAN_POINT ( 'NONE',  ( 127.0915067942438839, -1.262365849409121221, -9.320838424185609483 ) ) ;
#37410 = CARTESIAN_POINT ( 'NONE',  ( 118.4689281442453250, -10.15424416112533912, -14.75197769757731336 ) ) ;
#37411 = VERTEX_POINT ( 'NONE', #10912 ) ;
#37412 = CARTESIAN_POINT ( 'NONE',  ( 119.3765548109119550, 0.9020085738987385637, -11.91225656197091887 ) ) ;
#37413 = AXIS2_PLACEMENT_3D ( 'NONE', #29302, #15398, #19270 ) ;
#37414 = EDGE_CURVE ( 'NONE', #27673, #17596, #28088, .T. ) ;
#37415 = CARTESIAN_POINT ( 'NONE',  ( 115.0653281442453277, -6.344957434206662583, -7.627207830600332805 ) ) ;
#37416 = CARTESIAN_POINT ( 'NONE',  ( 122.3263414775786373, -3.505236298600246325, -18.68346056562440793 ) ) ;
#37417 = ORIENTED_EDGE ( 'NONE', *, *, #40060, .F. ) ;
#37418 = CARTESIAN_POINT ( 'NONE',  ( 121.2714235609119697, -9.645473719204776586, -14.86997237629376656 ) ) ;
#37419 = CARTESIAN_POINT ( 'NONE',  ( 137.4282737236158027, -0.5073614352806926631, -10.75960489339085768 ) ) ;
#37420 = CARTESIAN_POINT ( 'NONE',  ( 119.5467348109119712, -4.089484607189486809, -7.948022111789456723 ) ) ;
#37421 = CARTESIAN_POINT ( 'NONE',  ( 110.6909265045248247, -7.250697342233347165, -19.15521520033831138 ) ) ;
#37422 = CARTESIAN_POINT ( 'NONE',  ( 114.6682414775786469, -7.894159318335828068, -9.358103419637847864 ) ) ;
#37423 = VERTEX_POINT ( 'NONE', #35273 ) ;
#37424 = VERTEX_POINT ( 'NONE', #31872 ) ;
#37425 = CARTESIAN_POINT ( 'NONE',  ( 125.7299414775786346, -10.15424416112533912, -14.75197769757731336 ) ) ;
#37426 = CARTESIAN_POINT ( 'NONE',  ( 121.8725281442453223, -6.222761293078241884, -8.102969835052219238 ) ) ;
#37427 = CARTESIAN_POINT ( 'NONE',  ( 31.16856251326850824, -20.50830283073288385, -19.39321520033831447 ) ) ;
#37428 = CARTESIAN_POINT ( 'NONE',  ( 69.69189222814998175, -41.76310523276723785, -23.89321520033831803 ) ) ;
#37429 = CARTESIAN_POINT ( 'NONE',  ( 123.7445081442452874, -1.561330072975668948, -17.79121239304076951 ) ) ;
#37430 = CARTESIAN_POINT ( 'NONE',  ( 112.1721994132789320, -8.900630651041904429, -16.42135045828372597 ) ) ;
#37431 = CARTESIAN_POINT ( 'NONE',  ( 118.1852948109119836, -5.638512984488999180, -18.83840828888717311 ) ) ;
#37433 = CARTESIAN_POINT ( 'NONE',  ( 120.3409081442453044, -8.899110576539710493, -16.42337572283490132 ) ) ;
#37432 = CARTESIAN_POINT ( 'NONE',  ( 119.0361948109119652, -7.893985811506177619, -18.51759400769804742 ) ) ;
#37434 = DIRECTION ( 'NONE',  ( -0.000000000000000000, -0.9284778069183720062, -0.3713878862591650232 ) ) ;
#37435 = CARTESIAN_POINT ( 'NONE',  ( 112.0378865278262737, -1.036737761566193239, -17.24079555149560505 ) ) ;
#37436 = VERTEX_POINT ( 'NONE', #637 ) ;
#37437 = CARTESIAN_POINT ( 'NONE',  ( 122.8936081442453059, -9.565557343593413364, -10.61323700422348004 ) ) ;
#37438 = CARTESIAN_POINT ( 'NONE',  ( 116.5944421295247793, -4.863998795839590272, -13.39321520033831447 ) ) ;
#37439 = CARTESIAN_POINT ( 'NONE',  ( 121.1018636130535384, -8.422568683347405383, -17.41241596312870854 ) ) ;
#37440 = CARTESIAN_POINT ( 'NONE',  ( 109.1629577545248395, -7.250697342233347165, -7.631215200338321125 ) ) ;
#37441 = CARTESIAN_POINT ( 'NONE',  ( 111.5938171295247940, 0.1403307496149613920, -13.39321520033831447 ) ) ;
#37442 = CARTESIAN_POINT ( 'NONE',  ( 106.3848327545248651, -2.477300249445798297, -19.15521520033831138 ) ) ;
#37443 = CARTESIAN_POINT ( 'NONE',  ( 123.8579614775786126, 0.5811942927096110934, -14.16772938898807510 ) ) ;
#37444 = CARTESIAN_POINT ( 'NONE',  ( 124.0848681442452772, -5.574606645277164318, -18.38911715685844683 ) ) ;
#37445 = ORIENTED_EDGE ( 'NONE', *, *, #42473, .F. ) ;
#37446 = CARTESIAN_POINT ( 'NONE',  ( 124.5954081442453116, -3.383040157471821630, -19.15922257007629170 ) ) ;
#37447 = CARTESIAN_POINT ( 'NONE',  ( 113.4769814775786330, 0.4262465694468514643, -12.03445270309931736 ) ) ;
#37448 = CARTESIAN_POINT ( 'NONE',  ( 84.39081516114413262, -30.32262605124143562, -12.39321520033834645 ) ) ;
#37449 = CARTESIAN_POINT ( 'NONE',  ( 121.7023481442452777, -9.261995988541697145, -16.69588392320189030 ) ) ;
#37450 = CARTESIAN_POINT ( 'NONE',  ( 121.0216281442452981, -1.561330072975668948, -17.79121239304076951 ) ) ;
#37451 = CARTESIAN_POINT ( 'NONE',  ( 83.86216108596053687, -32.76310523276723785, -23.89321520033831803 ) ) ;
#37452 = CARTESIAN_POINT ( 'NONE',  ( 125.7866681442452688, -8.899110576539710493, -16.42337572283490132 ) ) ;
#37453 = CARTESIAN_POINT ( 'NONE',  ( 92.22433883960545131, -8.119819663282910938, -18.64321520033831803 ) ) ;
#37454 = DIRECTION ( 'NONE',  ( 0.9908103287288502203, -0.1352586133457981954, 0.000000000000000000 ) ) ;
#37455 = CIRCLE ( 'NONE', #27289, 0.4999999999999981681 ) ;
#37456 = VERTEX_POINT ( 'NONE', #14550 ) ;
#37457 = CARTESIAN_POINT ( 'NONE',  ( 124.6720798309150808, -2.215723800389698184, -18.16877924232191788 ) ) ;
#37458 = CARTESIAN_POINT ( 'NONE',  ( 114.5024048144346693, -2.280480477428486363, -18.08254604495228435 ) ) ;
#37459 = CARTESIAN_POINT ( 'NONE',  ( 123.9714148109119805, -8.899110576539710493, -16.42337572283490132 ) ) ;
#37460 = CARTESIAN_POINT ( 'NONE',  ( 107.9128015045248219, -6.936859964151250502, -18.39754474579286025 ) ) ;
#37461 = CARTESIAN_POINT ( 'NONE',  ( 110.3436608795247764, -1.325403438956436419, -16.93181055722141792 ) ) ;
#37462 = CARTESIAN_POINT ( 'NONE',  ( 119.0361948109119652, -2.084020599724406786, -8.691656652584148546 ) ) ;
#37463 = SHAPE_REPRESENTATION_RELATIONSHIP ( 'NONE' , 'NONE' ,  #26250, #34112 ) ;
#37464 = CARTESIAN_POINT ( 'NONE',  ( 117.7882081442453170, -3.505236298600246325, -18.68346056562440793 ) ) ;
#37465 = CARTESIAN_POINT ( 'NONE',  ( 123.4041481442452834, -10.30919188438810075, -12.61870101168855918 ) ) ;
#37466 = ORIENTED_EDGE ( 'NONE', *, *, #8387, .T. ) ;
#37467 = AXIS2_PLACEMENT_3D ( 'NONE', #35046, #31646, #3400 ) ;
#37468 = CARTESIAN_POINT ( 'NONE',  ( 123.0637881442452937, -8.899110576539710493, -16.42337572283490132 ) ) ;
#37469 = CARTESIAN_POINT ( 'NONE',  ( 119.8303681442453126, -10.63000616557722466, -14.87417383870573495 ) ) ;
#37470 = CARTESIAN_POINT ( 'NONE',  ( 124.9924948109119924, -4.089484607189486809, -7.948022111789456723 ) ) ;
#37471 = EDGE_CURVE ( 'NONE', #14403, #40384, #39302, .T. ) ;
#37472 = CARTESIAN_POINT ( 'NONE',  ( 122.8936081442453059, -9.565557343593413364, -10.61323700422348004 ) ) ;
#37473 = ORIENTED_EDGE ( 'NONE', *, *, #44180, .T. ) ;
#37474 = DIRECTION ( 'NONE',  ( -2.439015257082815255E-15, 1.000000000000000000, 0.000000000000000000 ) ) ;
#37475 = CARTESIAN_POINT ( 'NONE',  ( 124.3685014775786328, -10.63000616557722466, -14.87417383870573495 ) ) ;
#37476 = CARTESIAN_POINT ( 'NONE',  ( 116.3700414775786527, -4.153390946401321671, -8.397313243818183892 ) ) ;
#37477 = CARTESIAN_POINT ( 'NONE',  ( 123.4608748109119745, -10.63000616557722466, -14.87417383870573495 ) ) ;
#37478 =( BOUNDED_CURVE ( )  B_SPLINE_CURVE ( 2, ( #13401, #6319, #19775, #27303, #23889, #17046, #34123, #12946, #41442, #44406, #38649, #18379, #42547, #21566, #38434, #34989, #6994 ),
 .UNSPECIFIED., .F., .T. ) 
 B_SPLINE_CURVE_WITH_KNOTS ( ( 3, 2, 2, 2, 2, 2, 2, 2, 3 ),
 ( 0.7602707595410509445, 0.7812500000000000000, 0.8125000000000000000, 0.8437500000000000000, 0.8750000000000000000, 0.9062500000000000000, 0.9375000000000000000, 0.9687500000000000000, 0.9897292404589489445 ),
 .UNSPECIFIED. ) 
 CURVE ( )  GEOMETRIC_REPRESENTATION_ITEM ( )  RATIONAL_B_SPLINE_CURVE ( ( 0.9664089390052280626, 0.9488976130786129781, 1.000000000000000000, 0.9238795325112869605, 1.000000000000000000, 0.9238795325112869605, 1.000000000000000000, 0.9238795325112869605, 1.000000000000000000, 0.9238795325112869605, 1.000000000000000000, 0.9238795325112869605, 1.000000000000000000, 0.9238795325112869605, 1.000000000000000000, 0.9488976130786129781, 0.9664089390052290618 ) ) 
 REPRESENTATION_ITEM ( '' )  );
#37479 = FACE_OUTER_BOUND ( 'NONE', #31965, .T. ) ;
#37480 = CARTESIAN_POINT ( 'NONE',  ( 124.0495485609119584, -0.08252387247370887580, -11.91645802438286417 ) ) ;
#37481 = VERTEX_POINT ( 'NONE', #36404 ) ;
#37482 = CARTESIAN_POINT ( 'NONE',  ( 116.5564130180080866, 0.7607806665037644134, -14.64321520033833401 ) ) ;
#37483 = AXIS2_PLACEMENT_3D ( 'NONE', #41272, #10249, #13222 ) ;
#37484 = CARTESIAN_POINT ( 'NONE',  ( 108.7462390045248242, -9.868328341294098749, -11.32035403202665869 ) ) ;
#37485 = DIRECTION ( 'NONE',  ( -1.000000000000000000, 0.000000000000000000, -0.000000000000000000 ) ) ;
#37486 = CARTESIAN_POINT ( 'NONE',  ( 122.5532481442453019, 0.4262465694468514643, -12.03445270309931736 ) ) ;
#37487 = CARTESIAN_POINT ( 'NONE',  ( 113.2500748109119968, -3.505236298600246325, -18.68346056562440793 ) ) ;
#37488 = CARTESIAN_POINT ( 'NONE',  ( 125.3328548109119964, -0.8288870151387812690, -10.36305467784172407 ) ) ;
#37489 = ORIENTED_EDGE ( 'NONE', *, *, #27729, .F. ) ;
#37490 = DIRECTION ( 'NONE',  ( -0.000000000000000000, -0.9284778069183721172, -0.3713878862591650232 ) ) ;
#37491 = CARTESIAN_POINT ( 'NONE',  ( 120.6812681442452941, 0.1319031606808879209, -14.10382304977623669 ) ) ;
#37492 = AXIS2_PLACEMENT_3D ( 'NONE', #27071, #30937, #10198 ) ;
#37493 = CARTESIAN_POINT ( 'NONE',  ( 116.3631031537514815, 0.4930828106259610433, -14.64321520033831447 ) ) ;
#37494 = CARTESIAN_POINT ( 'NONE',  ( 112.7745202545247736, -10.62599879583958540, -15.77991374673208469 ) ) ;
#37495 = CYLINDRICAL_SURFACE ( 'NONE', #34758, 3.000000000000001776 ) ;
#37497 = CARTESIAN_POINT ( 'NONE',  ( 125.7866681442452688, -0.4660016031367893996, -10.09054647747474043 ) ) ;
#37496 = CARTESIAN_POINT ( 'NONE',  ( 68.68839935636916039, -25.95913848132418522, -5.893215200338315363 ) ) ;
#37498 = CARTESIAN_POINT ( 'NONE',  ( 125.7299414775786346, -10.15424416112533912, -14.75197769757731336 ) ) ;
#37499 = EDGE_LOOP ( 'NONE', ( #2641, #13498, #4267, #4296, #13754 ) ) ;
#37500 = CARTESIAN_POINT ( 'NONE',  ( 113.5904348109119866, -7.893985811506177619, -18.51759400769804742 ) ) ;
#37501 = DIRECTION ( 'NONE',  ( 0.3445294493088594256, 0.9387755102040817867, 0.000000000000000000 ) ) ;
#37502 = CARTESIAN_POINT ( 'NONE',  ( 106.0375671295248310, 0.1403307496149613920, -13.39321520033831447 ) ) ;
#37503 = CARTESIAN_POINT ( 'NONE',  ( 124.3117748109119844, 0.1319031606808879209, -14.10382304977623669 ) ) ;
#37504 = CARTESIAN_POINT ( 'NONE',  ( 121.5888948109119809, 0.1319031606808879209, -14.10382304977623669 ) ) ;
#37505 = DIRECTION ( 'NONE',  ( -0.9908103287288504424, 0.1352586133457950313, 0.000000000000000000 ) ) ;
#37506 = CARTESIAN_POINT ( 'NONE',  ( 115.6220983795247861, -8.402594152722688392, -16.93181055722141792 ) ) ;
#37507 = CARTESIAN_POINT ( 'NONE',  ( 70.19189222814998175, -100.0979043305785581, -53.24182196210380624 ) ) ;
#37508 = CARTESIAN_POINT ( 'NONE',  ( 126.2184548109105435, -0.8658195297460520301, -10.39078908864422246 ) ) ;
#37509 = CYLINDRICAL_SURFACE ( 'NONE', #9536, 1.999999999999998890 ) ;
#37510 = CARTESIAN_POINT ( 'NONE',  ( 110.7603796295247918, -4.863998795839590272, -19.15521520033831493 ) ) ;
#37511 = DIRECTION ( 'NONE',  ( 0.000000000000000000, 0.000000000000000000, -1.000000000000000000 ) ) ;
#37512 = CARTESIAN_POINT ( 'NONE',  ( 113.2606921295247702, 0.8980012041604618078, -13.39321520033831447 ) ) ;
#37513 = CARTESIAN_POINT ( 'NONE',  ( 124.1983214775786166, -8.166667518702819706, -8.995218007635861213 ) ) ;
#37514 = CARTESIAN_POINT ( 'NONE',  ( 122.9503348109119827, 0.5811942927096110934, -14.16772938898807510 ) ) ;
#37515 = CARTESIAN_POINT ( 'NONE',  ( 120.8160396737536928, -8.611453504372539314, -17.77011218421760574 ) ) ;
#37516 = CARTESIAN_POINT ( 'NONE',  ( 119.4332814775786318, -0.4660016031367893996, -10.09054647747474043 ) ) ;
#37517 = B_SPLINE_CURVE_WITH_KNOTS ( 'NONE', 3,
 ( #31378, #23666, #21123, #17271, #45081, #20468, #3127, #149, #27982, #24553, #34997, #30944, #17705, #31605, #4683, #25674, #39579, #24767, #817, #36139, #15409, #8122, #18387, #4008, #14509, #22243, #42333, #38890, #29313, #4466, #7659, #7891, #11545, #32275, #21797, #8342, #11094, #1487, #29085, #22023, #10872, #14736, #11316, #42997, #7427, #42554, #21348, #25226, #28648, #32715, #35232, #1270, #17930, #599, #28871, #25452 ),
 .UNSPECIFIED., .F., .F.,
 ( 4, 2, 2, 2, 2, 2, 2, 1, 2, 2, 2, 2, 2, 2, 2, 2, 2, 2, 2, 2, 2, 1, 2, 2, 2, 2, 2, 2, 4 ),
 ( 0.000000000000000000, 0.06250000000001540434, 0.09375000000001655620, 0.1093750000000236755, 0.1250000000000308087, 0.1875000000000596467, 0.2187500000000681954, 0.2343750000000779099, 0.2421875000000825451, 0.2500000000000871525, 0.3125000000001046940, 0.3437500000001088019, 0.3593750000001146860, 0.3750000000001205147, 0.5000000000001594280, 0.5625000000001791900, 0.5937500000001889600, 0.6093750000001936229, 0.6250000000001982858, 0.6875000000002169376, 0.7187500000002267075, 0.7343750000002317035, 0.7421875000002340350, 0.7500000000002362555, 0.8125000000001991740, 0.8437500000001806333, 0.8593750000001714184, 0.8750000000001620926, 1.000000000000000000 ),
 .UNSPECIFIED. ) ;
#37518 = CARTESIAN_POINT ( 'NONE',  ( 111.9453614775786434, -1.561330072975668060, -17.79121239304076596 ) ) ;
#37519 = VERTEX_POINT ( 'NONE', #12489 ) ;
#37520 = CARTESIAN_POINT ( 'NONE',  ( 114.6682414775786469, -7.894159318335828068, -9.358103419637847864 ) ) ;
#37521 = CARTESIAN_POINT ( 'NONE',  ( 124.6521348109119884, -1.561330072975668948, -17.79121239304076951 ) ) ;
#37522 = CARTESIAN_POINT ( 'NONE',  ( 122.9503348109119827, 0.5811942927096110934, -14.16772938898807510 ) ) ;
#37523 = CARTESIAN_POINT ( 'NONE',  ( 114.3846081442453197, -10.63000616557722466, -14.87417383870573495 ) ) ;
#37524 = ITEM_DEFINED_TRANSFORMATION ( 'NONE', 'NONE', #16966,  #12375 ) ;
#37525 = CARTESIAN_POINT ( 'NONE',  ( 114.3846081442453197, 0.4262465694468514643, -12.03445270309931736 ) ) ;
#37526 = ORIENTED_EDGE ( 'NONE', *, *, #43751, .T. ) ;
#37527 = CARTESIAN_POINT ( 'NONE',  ( 117.7314814775786260, -5.574606645277164318, -18.38911715685844683 ) ) ;
#37528 = CIRCLE ( 'NONE', #17871, 8.000000000000000000 ) ;
#37529 = CARTESIAN_POINT ( 'NONE',  ( 105.5513952545248060, 0.8980012041604421569, -11.00651665394454071 ) ) ;
#37530 = CARTESIAN_POINT ( 'NONE',  ( 108.8851452545248151, -9.868328341294098749, -15.46607636864997204 ) ) ;
#37531 = CARTESIAN_POINT ( 'NONE',  ( 122.4397948109119767, -0.1624402480850797581, -16.17319339645315424 ) ) ;
#37532 = DIRECTION ( 'NONE',  ( 0.000000000000000000, -0.9242245927363029745, -0.3818493186865927758 ) ) ;
#37533 = CARTESIAN_POINT ( 'NONE',  ( 114.0246765045248196, -7.250697342233347165, -19.15521520033831138 ) ) ;
#37534 = ORIENTED_EDGE ( 'NONE', *, *, #41046, .T. ) ;
#37535 = DIRECTION ( 'NONE',  ( -0.9659258262890689783, -0.2588190451025185190, 0.000000000000000000 ) ) ;
#37536 = EDGE_CURVE ( 'NONE', #8271, #11048, #18612, .T. ) ;
#37537 = CARTESIAN_POINT ( 'NONE',  ( 125.2194014775786286, -10.30919188438810075, -12.61870101168855918 ) ) ;
#37538 = DIRECTION ( 'NONE',  ( -0.000000000000000000, -0.9284778069183720062, -0.3713878862591650232 ) ) ;
#37539 = CARTESIAN_POINT ( 'NONE',  ( 70.89841814381148311, -68.89136543047671069, -37.69090763720760151 ) ) ;
#37540 = VECTOR ( 'NONE', #33853, 1000.000000000000114 ) ;
#37541 = CARTESIAN_POINT ( 'NONE',  ( 90.06246830635160450, -26.60966817898065884, -11.90521360603286816 ) ) ;
#37542 = CARTESIAN_POINT ( 'NONE',  ( 106.2459265045248173, -2.791137627527939813, -8.388885654883777576 ) ) ;
#37543 = CARTESIAN_POINT ( 'NONE',  ( 123.1153024678160932, -1.149058757900107697, -17.09122335155391781 ) ) ;
#37544 = CARTESIAN_POINT ( 'NONE',  ( 119.2063748109119814, -1.561330072975668504, -17.79121239304076951 ) ) ;
#37545 = CARTESIAN_POINT ( 'NONE',  ( 136.3130839835673100, -4.208110519389379967, -19.18091293523846019 ) ) ;
#37546 = AXIS2_PLACEMENT_3D ( 'NONE', #8446, #33485, #2263 ) ;
#37547 = CARTESIAN_POINT ( 'NONE',  ( 125.4584548109119737, -4.863998795839242995, -13.39321520033831447 ) ) ;
#37548 = CARTESIAN_POINT ( 'NONE',  ( 124.3999891859119913, -8.318316608003341273, -9.227040655997777563 ) ) ;
#37549 = B_SPLINE_CURVE_WITH_KNOTS ( 'NONE', 3,
 ( #7854, #25186, #11279, #21310, #18342, #39312, #35421, #3969, #32008, #31788, #560, #21533, #35652, #28378, #42291, #24956, #38852, #18115, #772, #14695, #39085, #21760, #4426, #32235, #6867, #37649, #44958, #17359, #23759, #24415, #10514, #44502, #10079, #6646, #20554, #2990, #16916, #13715, #7083, #27171, #34435 ),
 .UNSPECIFIED., .F., .F.,
 ( 4, 2, 1, 1, 1, 2, 2, 2, 1, 1, 1, 2, 2, 2, 2, 1, 1, 2, 2, 2, 2, 1, 2, 2, 4 ),
 ( 0.000000000000000000, 0.06249999999992449096, 0.09374999999988881116, 0.1093749999998711170, 0.1171874999998622630, 0.1210937499998595568, 0.1249999999998568645, 0.1874999999998673561, 0.2187499999998746836, 0.2343749999998763767, 0.2421874999998769873, 0.2460937499998774036, 0.2499999999998778200, 0.3749999999999229505, 0.4374999999999431011, 0.4687499999999530931, 0.4843749999999580891, 0.4921874999999604761, 0.4999999999999629186, 0.6249999999999770184, 0.6874999999999841238, 0.7187499999999891198, 0.7343749999999902300, 0.7499999999999912292, 1.000000000000000000 ),
 .UNSPECIFIED. ) ;
#37550 = CARTESIAN_POINT ( 'NONE',  ( 122.5532481442453019, 0.4262465694468514643, -12.03445270309931736 ) ) ;
#37551 = LINE ( 'NONE', #20241, #25534 ) ;
#37552 = EDGE_CURVE ( 'NONE', #33083, #17073, #25717, .T. ) ;
#37553 = ORIENTED_EDGE ( 'NONE', *, *, #38102, .T. ) ;
#37554 = CARTESIAN_POINT ( 'NONE',  ( 122.2131136130535367, -8.422568683347400054, -17.41241596312869788 ) ) ;
#37555 = CARTESIAN_POINT ( 'NONE',  ( 119.7736414775786358, -10.30919188438810075, -12.61870101168855918 ) ) ;
#37556 = FACE_OUTER_BOUND ( 'NONE', #44484, .T. ) ;
#37557 = CARTESIAN_POINT ( 'NONE',  ( 115.7460481442453357, -10.15424416112533912, -14.75197769757731336 ) ) ;
#37558 = EDGE_CURVE ( 'NONE', #854, #26347, #133, .T. ) ;
#37559 = EDGE_CURVE ( 'NONE', #33002, #16491, #29356, .T. ) ;
#37560 = CIRCLE ( 'NONE', #23753, 2.999999999999999556 ) ;
#37561 = CARTESIAN_POINT ( 'NONE',  ( 123.1772414775786189, -4.089484607189486809, -7.948022111789456723 ) ) ;
#37562 = CARTESIAN_POINT ( 'NONE',  ( 111.3160046295247838, -4.863998795839590272, -7.631215200338315796 ) ) ;
#37563 = CARTESIAN_POINT ( 'NONE',  ( 69.69189222814998175, -41.76310523276723785, -47.71602681600972318 ) ) ;
#37564 = CARTESIAN_POINT ( 'NONE',  ( 124.3454436379668380, -12.76346192841408467, -14.38917066012018431 ) ) ;
#37565 = CARTESIAN_POINT ( 'NONE',  ( 115.6325948109119821, -9.565557343593413364, -10.61323700422348004 ) ) ;
#37566 = CARTESIAN_POINT ( 'NONE',  ( 116.7104014775786425, -8.899110576539710493, -16.42337572283490132 ) ) ;
#37567 = CIRCLE ( 'NONE', #44878, 26.50000000000000000 ) ;
#37568 = CARTESIAN_POINT ( 'NONE',  ( 84.38170309240724976, -25.99489077589524300, -13.39321520033831447 ) ) ;
#37569 = CARTESIAN_POINT ( 'NONE',  ( 113.0523327545247838, -6.936859964151250502, -8.388885654883777576 ) ) ;
#37570 = EDGE_LOOP ( 'NONE', ( #25034, #11910, #39746, #41250 ) ) ;
#37571 = CARTESIAN_POINT ( 'NONE',  ( 109.2294422423184272, -0.4618089760604071059, -15.91181704383022932 ) ) ;
#37572 = CARTESIAN_POINT ( 'NONE',  ( 114.4413348109119823, -9.261995988541697145, -16.69588392320189030 ) ) ;
#37573 = CARTESIAN_POINT ( 'NONE',  ( 122.8568264975817499, -2.215723800389698184, -18.16877924232191788 ) ) ;
#37574 = CARTESIAN_POINT ( 'NONE',  ( 121.2714235609119697, -9.645473719204776586, -14.86997237629376656 ) ) ;
#37575 = CARTESIAN_POINT ( 'NONE',  ( 119.3267360609119692, -3.387241619883791355, -18.17469012370385073 ) ) ;
#37576 = EDGE_LOOP ( 'NONE', ( #44119, #21487, #11823, #9983, #37796 ) ) ;
#37577 = CARTESIAN_POINT ( 'NONE',  ( 70.19189222814998175, -50.19222220871606766, -33.27972307567368659 ) ) ;
#37578 = CARTESIAN_POINT ( 'NONE',  ( 84.77016061404391678, -25.38011337280982715, -14.88121679464376257 ) ) ;
#37579 = EDGE_LOOP ( 'NONE', ( #31241, #29174, #12611, #39754 ) ) ;
#37580 = CARTESIAN_POINT ( 'NONE',  ( 118.0718414775786300, -9.261995988541697145, -16.69588392320189030 ) ) ;
#37581 = CARTESIAN_POINT ( 'NONE',  ( 112.6260814775786514, -9.261995988541697145, -16.69588392320189030 ) ) ;
#37582 = CARTESIAN_POINT ( 'NONE',  ( 116.7104014775786425, -8.899110576539710493, -16.42337572283490132 ) ) ;
#37583 = AXIS2_PLACEMENT_3D ( 'NONE', #21480, #35365, #32180 ) ;
#37584 = DIRECTION ( 'NONE',  ( 0.5040994586965589219, 0.8636456077245088236, 0.000000000000000000 ) ) ;
#37585 = CARTESIAN_POINT ( 'NONE',  ( 122.8936081442453059, 0.2603800115204892296, -16.42320221600525088 ) ) ;
#37586 = CARTESIAN_POINT ( 'NONE',  ( 117.3911214775786505, -1.561330072975668504, -17.79121239304076951 ) ) ;
#37587 = ADVANCED_FACE ( 'NONE', ( #4731 ), #8386, .T. ) ;
#37588 = CIRCLE ( 'NONE', #12872, 2.999999999999999556 ) ;
#37589 = CARTESIAN_POINT ( 'NONE',  ( 106.9404577545248145, -2.791137627527939813, -18.39754474579286025 ) ) ;
#37590 = CARTESIAN_POINT ( 'NONE',  ( 114.4980614775786734, -2.084020599724406786, -8.691656652584148546 ) ) ;
#37591 = DIRECTION ( 'NONE',  ( 0.000000000000000000, -1.000000000000000000, 0.000000000000000000 ) ) ;
#37592 = ORIENTED_EDGE ( 'NONE', *, *, #6114, .T. ) ;
#37593 = CARTESIAN_POINT ( 'NONE',  ( 119.1496481442453046, -3.383040157471821630, -19.15922257007629170 ) ) ;
#37594 = ADVANCED_FACE ( 'NONE', ( #15452 ), #36186, .F. ) ;
#37595 = CIRCLE ( 'NONE', #39052, 1.000000000000000888 ) ;
#37596 = DIRECTION ( 'NONE',  ( 0.9609149988134833009, -0.1028163501681649411, 0.2570431154366530913 ) ) ;
#37597 = EDGE_CURVE ( 'NONE', #1633, #6756, #13743, .T. ) ;
#37598 = CARTESIAN_POINT ( 'NONE',  ( 116.7671281442453335, -1.834011780172310813, -8.268836392978581529 ) ) ;
#37599 = ORIENTED_EDGE ( 'NONE', *, *, #34917, .T. ) ;
#37600 = CARTESIAN_POINT ( 'NONE',  ( 120.5110881442453206, -6.344957434206665248, -7.627207830600338134 ) ) ;
#37601 = DIRECTION ( 'NONE',  ( -1.000000000000000000, 0.000000000000000000, 0.000000000000000000 ) ) ;
#37602 = CARTESIAN_POINT ( 'NONE',  ( 112.5126281442453120, 0.1319031606808879209, -14.10382304977623669 ) ) ;
#37603 = CARTESIAN_POINT ( 'NONE',  ( 78.63502652544006821, -59.11697439676735399, 0.04365315361115504333 ) ) ;
#37604 = CARTESIAN_POINT ( 'NONE',  ( 114.6682414775786469, -7.894159318335828068, -9.358103419637847864 ) ) ;
#37605 = FACE_OUTER_BOUND ( 'NONE', #21504, .T. ) ;
#37606 = CARTESIAN_POINT ( 'NONE',  ( 119.0361948109119652, -2.084020599724406786, -8.691656652584148546 ) ) ;
#37607 = DIRECTION ( 'NONE',  ( -1.000000000000000000, 0.000000000000000000, 0.000000000000000000 ) ) ;
#37608 = CARTESIAN_POINT ( 'NONE',  ( 113.9875214775786532, -8.899110576539710493, -16.42337572283490132 ) ) ;
#37609 = CARTESIAN_POINT ( 'NONE',  ( 113.9875214775786532, -0.4660016031367893996, -10.09054647747474043 ) ) ;
#37610 = CARTESIAN_POINT ( 'NONE',  ( 119.8823610609119754, -3.163656168406935087, -18.89861972220014508 ) ) ;
#37611 = CARTESIAN_POINT ( 'NONE',  ( 112.3424481442453384, -6.344957434206662583, -7.627207830600332805 ) ) ;
#37612 = CARTESIAN_POINT ( 'NONE',  ( 116.7104014775786425, -8.899110576539710493, -16.42337572283490132 ) ) ;
#37613 = CARTESIAN_POINT ( 'NONE',  ( 113.3068014775786594, -1.833838273342658809, -17.42832698103878286 ) ) ;
#37614 = EDGE_CURVE ( 'NONE', #7363, #4044, #24783, .T. ) ;
#37615 = CARTESIAN_POINT ( 'NONE',  ( 118.1285681442453068, -2.084020599724406786, -8.691656652584148546 ) ) ;
#37616 = VERTEX_POINT ( 'NONE', #2200 ) ;
#37617 = DIRECTION ( 'NONE',  ( 0.000000000000000000, -0.9242245927363029745, -0.3818493186865927203 ) ) ;
#37618 = CARTESIAN_POINT ( 'NONE',  ( 109.6491296295247793, -4.863998795839590272, -19.15521520033831493 ) ) ;
#37619 = VECTOR ( 'NONE', #8168, 1000.000000000000227 ) ;
#37620 = CARTESIAN_POINT ( 'NONE',  ( 105.6208483795248299, -8.402594152722688392, -16.93181055722141792 ) ) ;
#37621 = CARTESIAN_POINT ( 'NONE',  ( 106.1764733795248219, -1.325403438956436419, -9.854619843455211026 ) ) ;
#37622 = CARTESIAN_POINT ( 'NONE',  ( 109.7880358795247986, -0.7896495226426338832, -17.46756447353518382 ) ) ;
#37623 = CARTESIAN_POINT ( 'NONE',  ( 118.5823814775786360, -1.834011780172310813, -8.268836392978581529 ) ) ;
#37624 = ORIENTED_EDGE ( 'NONE', *, *, #32712, .F. ) ;
#37625 = CARTESIAN_POINT ( 'NONE',  ( 125.9568481442452850, -6.344957434206665248, -7.627207830600338134 ) ) ;
#37626 = FACE_OUTER_BOUND ( 'NONE', #12337, .T. ) ;
#37627 = CARTESIAN_POINT ( 'NONE',  ( 116.2565881442453133, -0.8288870151387760510, -10.36305467784173118 ) ) ;
#37628 = DIRECTION ( 'NONE',  ( -0.9908103287288505534, 0.1352586133457950590, 0.000000000000000000 ) ) ;
#37629 = CONICAL_SURFACE ( 'NONE', #39805, 1.610000000000000986, 0.9599310885968765916 ) ;
#37630 = CARTESIAN_POINT ( 'NONE',  ( 124.3685014775786328, -10.63000616557722466, -14.87417383870573495 ) ) ;
#37631 = CARTESIAN_POINT ( 'NONE',  ( 107.3571765045248299, -7.250697342233347165, -19.15521520033831138 ) ) ;
#37632 = CARTESIAN_POINT ( 'NONE',  ( 89.16950374942143753, -10.33215483242199717, -14.02354088222794637 ) ) ;
#37633 = ORIENTED_EDGE ( 'NONE', *, *, #28346, .F. ) ;
#37634 = CARTESIAN_POINT ( 'NONE',  ( 111.8779471478583929, -3.807985514183284348, -19.09877912889400875 ) ) ;
#37635 = CARTESIAN_POINT ( 'NONE',  ( 122.9503348109119827, -9.859900752359378018, -12.68260735090039759 ) ) ;
#37636 = CARTESIAN_POINT ( 'NONE',  ( 121.3052614775786111, -1.834011780172310813, -8.268836392978581529 ) ) ;
#37637 = CARTESIAN_POINT ( 'NONE',  ( 114.2711548109119803, -0.1624402480850797581, -16.17319339645315424 ) ) ;
#37638 = CARTESIAN_POINT ( 'NONE',  ( 118.5256548109119876, -0.4660016031367893996, -10.09054647747474043 ) ) ;
#37639 = CARTESIAN_POINT ( 'NONE',  ( 123.3590514748722455, -0.1020945015695005759, -15.74893487844868112 ) ) ;
#37640 = CARTESIAN_POINT ( 'NONE',  ( 126.5041214912225627, -1.164387443341326378, -9.820872858089868984 ) ) ;
#37641 = CARTESIAN_POINT ( 'NONE',  ( 124.7655881442452852, -9.859900752359378018, -12.68260735090039759 ) ) ;
#37642 = VERTEX_POINT ( 'NONE', #10195 ) ;
#37643 = DIRECTION ( 'NONE',  ( 0.3445294493088594256, 0.9387755102040817867, 2.035644895278904423E-16 ) ) ;
#37644 = AXIS2_PLACEMENT_3D ( 'NONE', #27059, #40979, #37532 ) ;
#37645 = CARTESIAN_POINT ( 'NONE',  ( 117.8449348109119938, -8.166667518702817929, -8.995218007635861213 ) ) ;
#37646 = CARTESIAN_POINT ( 'NONE',  ( 121.6456214775786293, 0.4262465694468514643, -12.03445270309931736 ) ) ;
#37647 = ORIENTED_EDGE ( 'NONE', *, *, #44819, .T. ) ;
#37648 = CARTESIAN_POINT ( 'NONE',  ( 123.0077516859119839, -0.6942167230862511529, -9.935906262978006609 ) ) ;
#37649 = CARTESIAN_POINT ( 'NONE',  ( 63.02684575864485339, -12.60992855379462618, -10.24602201293989978 ) ) ;
#37650 = CARTESIAN_POINT ( 'NONE',  ( 116.9373081442452929, -8.166667518702817929, -8.995218007635861213 ) ) ;
#37651 = CARTESIAN_POINT ( 'NONE',  ( 110.4825671295247815, -10.62599879583958540, -13.39321520033831447 ) ) ;
#37652 = CARTESIAN_POINT ( 'NONE',  ( 115.9729548109119861, -3.505236298600246325, -18.68346056562440793 ) ) ;
#37653 = VECTOR ( 'NONE', #9422, 1000.000000000000000 ) ;
#37654 = ORIENTED_EDGE ( 'NONE', *, *, #1684, .F. ) ;
#37655 = ORIENTED_EDGE ( 'NONE', *, *, #44274, .T. ) ;
#37656 = CARTESIAN_POINT ( 'NONE',  ( 126.0703014775786102, -0.1624402480850797581, -16.17319339645315424 ) ) ;
#37657 = CARTESIAN_POINT ( 'NONE',  ( 70.89841814381148311, -71.67679885123182260, -38.80507129598510119 ) ) ;
#37658 = FACE_OUTER_BOUND ( 'NONE', #12419, .T. ) ;
#37659 = EDGE_CURVE ( 'NONE', #9906, #19817, #20457, .T. ) ;
#37660 = TOROIDAL_SURFACE ( 'NONE', #1261, 8.800000000000000711, 1.199999999999999956 ) ;
#37661 = ORIENTED_EDGE ( 'NONE', *, *, #11932, .T. ) ;
#37662 = CARTESIAN_POINT ( 'NONE',  ( 121.4754414775786131, -8.166667518702819706, -8.995218007635861213 ) ) ;
#37663 = DIRECTION ( 'NONE',  ( 0.000000000000000000, -0.6004852223388322807, 0.7996358532186280677 ) ) ;
#37664 = LINE ( 'NONE', #16703, #30260 ) ;
#37665 = CARTESIAN_POINT ( 'NONE',  ( 120.2841814775786276, 0.9020085738987339008, -11.91225656197089222 ) ) ;
#37667 = CARTESIAN_POINT ( 'NONE',  ( 119.1496481442453046, -6.222761293078241884, -8.102969835052219238 ) ) ;
#37666 = CARTESIAN_POINT ( 'NONE',  ( 120.6812681442452941, -10.30919188438810075, -12.61870101168855918 ) ) ;
#37668 = CARTESIAN_POINT ( 'NONE',  ( 124.5954081442453116, -6.222761293078241884, -8.102969835052219238 ) ) ;
#37669 = CARTESIAN_POINT ( 'NONE',  ( 113.3635281442453504, -9.988377603198976828, -10.36322818467138340 ) ) ;
#37670 = EDGE_LOOP ( 'NONE', ( #32243, #39989, #33349, #3480, #16920 ) ) ;
#37671 = CARTESIAN_POINT ( 'NONE',  ( 123.4041481442452834, 0.1319031606808879209, -14.10382304977623669 ) ) ;
#37672 = CARTESIAN_POINT ( 'NONE',  ( 125.3790414775786388, -0.8658195297466895202, -10.39078908864337514 ) ) ;
#37673 = CARTESIAN_POINT ( 'NONE',  ( 107.1488171295247867, -10.62599879583958540, -13.39321520033831447 ) ) ;
#37674 = CARTESIAN_POINT ( 'NONE',  ( 112.7745202545247878, 0.1403307496149616695, -11.32035403202665336 ) ) ;
#37675 = CARTESIAN_POINT ( 'NONE',  ( 108.5378796295247810, -4.863998795839590272, -19.15521520033831493 ) ) ;
#37676 = AXIS2_PLACEMENT_3D ( 'NONE', #6980, #14715, #32254 ) ;
#37677 = CARTESIAN_POINT ( 'NONE',  ( 124.0281414775786146, -1.834011780172310813, -8.268836392978581529 ) ) ;
#37678 = CARTESIAN_POINT ( 'NONE',  ( 123.4041481442452834, 0.1319031606808879209, -14.10382304977623669 ) ) ;
#37679 = ORIENTED_EDGE ( 'NONE', *, *, #11844, .F. ) ;
#37680 = CARTESIAN_POINT ( 'NONE',  ( 125.8433948109119456, -1.834011780172310813, -8.268836392978581529 ) ) ;
#37681 = FACE_OUTER_BOUND ( 'NONE', #28966, .T. ) ;
#37682 = DIRECTION ( 'NONE',  ( -0.000000000000000000, -0.9284778069183718952, -0.3713878862591649677 ) ) ;
#37683 = EDGE_CURVE ( 'NONE', #816, #29699, #21285, .T. ) ;
#37684 = CARTESIAN_POINT ( 'NONE',  ( 124.7088614775786226, 0.2603800115204892296, -16.42320221600525088 ) ) ;
#37685 = CARTESIAN_POINT ( 'NONE',  ( 120.6245414775786458, -9.988377603198976828, -10.36322818467138340 ) ) ;
#37686 = CARTESIAN_POINT ( 'NONE',  ( 119.8097329359119811, -4.360640073283683193, -8.004713379073654878 ) ) ;
#37687 = CARTESIAN_POINT ( 'NONE',  ( 113.1933481442453058, -4.089484607189486809, -7.948022111789456723 ) ) ;
#37688 = CARTESIAN_POINT ( 'NONE',  ( 31.33087284928348026, -19.31933043625826585, -8.593215200338315540 ) ) ;
#37689 = CARTESIAN_POINT ( 'NONE',  ( 107.3571765045248299, -7.250697342233347165, -19.15521520033831138 ) ) ;
#37690 = ORIENTED_EDGE ( 'NONE', *, *, #15719, .F. ) ;
#37691 = CARTESIAN_POINT ( 'NONE',  ( 124.8677593335883955, -2.334846009198413341, -18.01015021110790215 ) ) ;
#37692 = CARTESIAN_POINT ( 'NONE',  ( 112.7962614775786676, -6.222761293078241884, -8.102969835052219238 ) ) ;
#37693 = CARTESIAN_POINT ( 'NONE',  ( 125.5597614775786326, -7.894159318335828068, -9.358103419637847864 ) ) ;
#37694 = CARTESIAN_POINT ( 'NONE',  ( 109.3018640045248304, 0.1403307496149616695, -15.46607636864997204 ) ) ;
#37695 = CARTESIAN_POINT ( 'NONE',  ( 107.1488171295248861, 0.1403307496149613920, -13.39321520033831447 ) ) ;
#37696 = CARTESIAN_POINT ( 'NONE',  ( 122.8936081442453059, -9.565557343593413364, -10.61323700422348004 ) ) ;
#37697 = CARTESIAN_POINT ( 'NONE',  ( 68.68839935636917460, -25.95913848132418522, -5.893215200338315363 ) ) ;
#37698 = CARTESIAN_POINT ( 'NONE',  ( 115.2922348109119781, 0.4262465694468514643, -12.03445270309931736 ) ) ;
#37699 = CARTESIAN_POINT ( 'NONE',  ( 121.9292548109119849, -1.561330072975668948, -17.79121239304076951 ) ) ;
#37700 = VERTEX_POINT ( 'NONE', #20899 ) ;
#37701 = CIRCLE ( 'NONE', #27515, 1.610000000000000986 ) ;
#37702 = CARTESIAN_POINT ( 'NONE',  ( 121.7023481442452777, -0.8288870151387760510, -10.36305467784173118 ) ) ;
#37703 = CARTESIAN_POINT ( 'NONE',  ( 118.9227414775786400, -10.63000616557722466, -14.87417383870573495 ) ) ;
#37704 = CARTESIAN_POINT ( 'NONE',  ( 124.2550481442452792, -9.988377603198980381, -10.36322818467138518 ) ) ;
#37705 = CARTESIAN_POINT ( 'NONE',  ( 121.9470836909669913, -25.99489077589524300, -13.39321520033831447 ) ) ;
#37706 = VERTEX_POINT ( 'NONE', #360 ) ;
#37707 = CARTESIAN_POINT ( 'NONE',  ( 123.3482543740715442, -2.419733177069661512, -17.89711025544711376 ) ) ;
#37708 = CARTESIAN_POINT ( 'NONE',  ( 122.8368814775786291, -1.561330072975668948, -17.79121239304076951 ) ) ;
#37709 = CARTESIAN_POINT ( 'NONE',  ( 116.5402214775786405, -9.565557343593413364, -10.61323700422348004 ) ) ;
#37710 = AXIS2_PLACEMENT_3D ( 'NONE', #18096, #24281, #38167 ) ;
#37711 = CARTESIAN_POINT ( 'NONE',  ( 115.1220548109119761, -1.833838273342658809, -17.42832698103878286 ) ) ;
#37712 = CARTESIAN_POINT ( 'NONE',  ( 71.02242295334774269, -52.47502135561418157, -37.29764242556413478 ) ) ;
#37713 = CARTESIAN_POINT ( 'NONE',  ( 123.0772048109119652, -2.527210466738041728, -8.967976844669124148 ) ) ;
#37714 = ORIENTED_EDGE ( 'NONE', *, *, #29288, .T. ) ;
#37715 = FACE_OUTER_BOUND ( 'NONE', #16007, .T. ) ;
#37716 = CARTESIAN_POINT ( 'NONE',  ( 125.3566265649645715, 1.939509583157688954, -11.55384643022778945 ) ) ;
#37717 = CARTESIAN_POINT ( 'NONE',  ( 115.8999108795247821, -8.938348069036489818, -9.318865927141430916 ) ) ;
#37718 = CARTESIAN_POINT ( 'NONE',  ( 117.9024943740715656, -2.419733177069680607, -17.89711025544712442 ) ) ;
#37719 = CARTESIAN_POINT ( 'NONE',  ( 122.9503348109119827, -9.859900752359378018, -12.68260735090039759 ) ) ;
#37720 = CARTESIAN_POINT ( 'NONE',  ( 112.7395348109119766, -4.153390946401321671, -8.397313243818183892 ) ) ;
#37721 = CARTESIAN_POINT ( 'NONE',  ( 126.9276200068485991, -0.06140791722303787920, -11.02529072918189534 ) ) ;
#37722 = ORIENTED_EDGE ( 'NONE', *, *, #5477, .T. ) ;
#37723 = CARTESIAN_POINT ( 'NONE',  ( 77.77634386988368931, 3.254514819260763581, -12.14321520033831625 ) ) ;
#37724 = CARTESIAN_POINT ( 'NONE',  ( 113.1933481442453058, -5.574606645277164318, -18.38911715685844683 ) ) ;
#37725 = CARTESIAN_POINT ( 'NONE',  ( 112.6356140045247827, -10.62599879583958540, -11.00651665394455492 ) ) ;
#37726 = CARTESIAN_POINT ( 'NONE',  ( 111.8424481442453242, -6.210324830718715994, -8.151390318758327425 ) ) ;
#37728 = DIRECTION ( 'NONE',  ( -0.3445294493088594256, -0.9387755102040817867, 0.000000000000000000 ) ) ;
#37727 = DIRECTION ( 'NONE',  ( 0.000000000000000000, -0.3818493186865927203, 0.9242245927363029745 ) ) ;
#37729 = EDGE_CURVE ( 'NONE', #1801, #21278, #33890, .T. ) ;
#37730 = CARTESIAN_POINT ( 'NONE',  ( 124.8223148109119762, -10.15424416112533912, -14.75197769757731336 ) ) ;
#37731 = VERTEX_POINT ( 'NONE', #17916 ) ;
#37732 = CARTESIAN_POINT ( 'NONE',  ( 113.0798948109119948, -0.4660016031367893996, -10.09054647747474043 ) ) ;
#37733 = CARTESIAN_POINT ( 'NONE',  ( 127.0066334553003315, 0.2291786611533031814, -15.16966009980168906 ) ) ;
#37734 = CARTESIAN_POINT ( 'NONE',  ( 114.0941296295247867, -4.863998795839590272, -19.15521520033831493 ) ) ;
#37735 = CARTESIAN_POINT ( 'NONE',  ( 124.4819548109119722, -2.084020599724406786, -8.691656652584148546 ) ) ;
#37736 = CARTESIAN_POINT ( 'NONE',  ( 122.7234281442452755, -4.153390946401325223, -8.397313243818185668 ) ) ;
#37737 = CARTESIAN_POINT ( 'NONE',  ( 63.27883505452616930, -30.76310523276723785, -21.89321520033831447 ) ) ;
#37738 = CARTESIAN_POINT ( 'NONE',  ( 113.9552233795247815, -1.325403438956436419, -9.854619843455211026 ) ) ;
#37739 = DIRECTION ( 'NONE',  ( -0.2768435750659241079, -0.3568721902840686355, 0.8921882507333134260 ) ) ;
#37740 = CARTESIAN_POINT ( 'NONE',  ( 120.2055705993907679, -9.245649465415469948, -16.16453161350215240 ) ) ;
#37741 = CARTESIAN_POINT ( 'NONE',  ( 113.7038881442453402, -6.222761293078241884, -8.102969835052219238 ) ) ;
#37742 = CARTESIAN_POINT ( 'NONE',  ( 107.4266296295248821, -4.863998795839590272, -19.15521520033831493 ) ) ;
#37743 = VECTOR ( 'NONE', #40099, 1000.000000000000000 ) ;
#37744 = DIRECTION ( 'NONE',  ( 1.000000000000000000, 0.000000000000000000, -0.000000000000000000 ) ) ;
#37745 = CARTESIAN_POINT ( 'NONE',  ( 113.8857702545248003, -10.62599879583958717, -15.77991374673208469 ) ) ;
#37746 = CARTESIAN_POINT ( 'NONE',  ( 123.2339681442453241, -6.344957434206665248, -7.627207830600338134 ) ) ;
#37747 = CARTESIAN_POINT ( 'NONE',  ( 124.8790414775786246, -0.4660016031367893996, -10.09054647747474043 ) ) ;
#37748 = CARTESIAN_POINT ( 'NONE',  ( 114.9275671295247889, -10.62599879583958540, -13.39321520033831625 ) ) ;
#37749 = CARTESIAN_POINT ( 'NONE',  ( 120.0572748109119772, -3.383040157471821630, -19.15922257007629170 ) ) ;
#37750 = CARTESIAN_POINT ( 'NONE',  ( 111.7184548109119788, -9.261995988541697145, -16.69588392320189030 ) ) ;
#37751 = ORIENTED_EDGE ( 'NONE', *, *, #36723, .F. ) ;
#37752 = CARTESIAN_POINT ( 'NONE',  ( 113.3068014775786594, -1.833838273342658809, -17.42832698103878286 ) ) ;
#37753 = CARTESIAN_POINT ( 'NONE',  ( 125.3328548109119964, -9.261995988541697145, -16.69588392320189030 ) ) ;
#37754 = CARTESIAN_POINT ( 'NONE',  ( 123.5176014775786228, -9.261995988541697145, -16.69588392320189030 ) ) ;
#37755 = CARTESIAN_POINT ( 'NONE',  ( 114.8951481442453115, -0.4660016031367893996, -10.09054647747474043 ) ) ;
#37756 = CARTESIAN_POINT ( 'NONE',  ( 112.7395348109119766, -4.153390946401321671, -8.397313243818183892 ) ) ;
#37757 = VERTEX_POINT ( 'NONE', #7645 ) ;
#37758 = CARTESIAN_POINT ( 'NONE',  ( 118.6958348109119754, -3.505236298600246325, -18.68346056562440793 ) ) ;
#37759 =( BOUNDED_CURVE ( )  B_SPLINE_CURVE ( 2, ( #37942, #27692, #2600, #6489, #34503, #3504, #34064, #6716, #6020, #19943, #10364, #3282, #17421, #17204, #27243, #31097, #2830 ),
 .UNSPECIFIED., .F., .F. ) 
 B_SPLINE_CURVE_WITH_KNOTS ( ( 3, 2, 2, 2, 2, 2, 2, 2, 3 ),
 ( 0.004043115603494570193, 0.01250000000000000069, 0.02500000000000000139, 0.03750000000000000555, 0.05000000000000000278, 0.06250000000000000000, 0.07499999999999999722, 0.08749999999999999445, 0.09595688439650570944 ),
 .UNSPECIFIED. ) 
 CURVE ( )  GEOMETRIC_REPRESENTATION_ITEM ( )  RATIONAL_B_SPLINE_CURVE ( ( 0.9666851417651740608, 0.9485006404992000206, 1.000000000000000000, 0.9238795325112869605, 1.000000000000000000, 0.9238795325112869605, 1.000000000000000000, 0.9238795325112869605, 1.000000000000000000, 0.9238795325112869605, 1.000000000000000000, 0.9238795325112869605, 1.000000000000000000, 0.9238795325112869605, 1.000000000000000000, 0.9485006404991980222, 0.9666851417651760592 ) ) 
 REPRESENTATION_ITEM ( '' )  );
#37760 = CARTESIAN_POINT ( 'NONE',  ( 90.33554924625337890, -25.99489077589524300, -13.39321520033831447 ) ) ;
#37761 = CARTESIAN_POINT ( 'NONE',  ( 124.4252281442452812, -0.8288870151387760510, -10.36305467784173118 ) ) ;
#37762 = CARTESIAN_POINT ( 'NONE',  ( 42.57150613532612482, -13.18613447638990088, -14.39321520033831625 ) ) ;
#37763 = CARTESIAN_POINT ( 'NONE',  ( 112.6356140045247827, -10.62599879583958717, -11.00651665394454604 ) ) ;
#37764 = ORIENTED_EDGE ( 'NONE', *, *, #41240, .F. ) ;
#37765 = CARTESIAN_POINT ( 'NONE',  ( 61.14763380861215580, -2.318372254017448508, -8.893215200339504634 ) ) ;
#37766 = CARTESIAN_POINT ( 'NONE',  ( 125.3328548109119964, -9.261995988541697145, -16.69588392320189030 ) ) ;
#37767 = CARTESIAN_POINT ( 'NONE',  ( 79.79010115959992788, 5.106172230548961188, -6.893215200338315363 ) ) ;
#37768 = CARTESIAN_POINT ( 'NONE',  ( 116.5856851890968642, 2.159773802720716951, -6.182123076206457846 ) ) ;
#37769 = CARTESIAN_POINT ( 'NONE',  ( 121.6547847346423055, -8.435056900666539903, -17.43606523319152757 ) ) ;
#37770 = CARTESIAN_POINT ( 'NONE',  ( 105.2041296295248287, -4.863998795839590272, -8.388885654883775800 ) ) ;
#37771 = CARTESIAN_POINT ( 'NONE',  ( 115.2154168734311241, -1.223627541775731631, -16.99192386690444323 ) ) ;
#37772 = CARTESIAN_POINT ( 'NONE',  ( 116.5969481442453031, 0.5811942927096154232, -14.16772938898807155 ) ) ;
#37773 = CARTESIAN_POINT ( 'NONE',  ( 137.3803399967318910, -4.959070169535716666, -18.53201221635876905 ) ) ;
#37774 = CARTESIAN_POINT ( 'NONE',  ( 68.07789357685331311, -68.58957386525776201, -38.44539312525988350 ) ) ;
#37775 = CARTESIAN_POINT ( 'NONE',  ( 124.7088614775786226, 0.2603800115204892296, -16.42320221600525088 ) ) ;
#37776 = CARTESIAN_POINT ( 'NONE',  ( 119.4900081442453086, -7.643976991954077427, -18.09477374809248928 ) ) ;
#37777 = ORIENTED_EDGE ( 'NONE', *, *, #33649, .F. ) ;
#37778 = DIRECTION ( 'NONE',  ( 0.000000000000000000, -0.3818493186865927203, 0.9242245927363029745 ) ) ;
#37779 = CARTESIAN_POINT ( 'NONE',  ( 118.9227414775786400, -10.63000616557722466, -14.87417383870573495 ) ) ;
#37780 = FACE_OUTER_BOUND ( 'NONE', #7868, .T. ) ;
#37781 = CARTESIAN_POINT ( 'NONE',  ( 116.1998614775786507, 0.4262465694468514643, -12.03445270309931736 ) ) ;
#37782 = CARTESIAN_POINT ( 'NONE',  ( 111.7184548109119788, -0.8288870151387760510, -10.36305467784173118 ) ) ;
#37783 = CARTESIAN_POINT ( 'NONE',  ( 110.4825671295247815, -10.62599879583958540, -13.39321520033831447 ) ) ;
#37784 = CARTESIAN_POINT ( 'NONE',  ( 105.8986608795248401, -1.325403438956436419, -16.93181055722141792 ) ) ;
#37785 = CARTESIAN_POINT ( 'NONE',  ( 115.6220983795247861, -0.7896495226426338832, -9.318865927141430916 ) ) ;
#37786 = CARTESIAN_POINT ( 'NONE',  ( 118.0151148109119816, 0.4262465694468514643, -12.03445270309931736 ) ) ;
#37787 = CARTESIAN_POINT ( 'NONE',  ( 118.6391081442452986, -5.574606645277164318, -18.38911715685844683 ) ) ;
#37788 = LINE ( 'NONE', #13634, #21893 ) ;
#37789 = CARTESIAN_POINT ( 'NONE',  ( 119.8823610609119754, -3.163656168406935087, -18.89861972220014508 ) ) ;
#37790 = CARTESIAN_POINT ( 'NONE',  ( 110.7603796295247918, -4.863998795839590272, -8.388885654883775800 ) ) ;
#37791 = ORIENTED_EDGE ( 'NONE', *, *, #9156, .F. ) ;
#37792 = CARTESIAN_POINT ( 'NONE',  ( 94.20708369096698220, -25.14343533174585943, -14.10537061818067883 ) ) ;
#37793 = CARTESIAN_POINT ( 'NONE',  ( 114.2144281442453178, -8.166667518702817929, -8.995218007635859436 ) ) ;
#37794 = DIRECTION ( 'NONE',  ( -1.000000000000000000, 0.000000000000000000, 0.000000000000000000 ) ) ;
#37795 = CARTESIAN_POINT ( 'NONE',  ( 120.2296266859119953, -9.033780868592240054, -16.85052413769862056 ) ) ;
#37796 = ORIENTED_EDGE ( 'NONE', *, *, #20558, .F. ) ;
#37797 = DIRECTION ( 'NONE',  ( -1.000000000000000000, 0.000000000000000000, 0.000000000000000000 ) ) ;
#37798 = ORIENTED_EDGE ( 'NONE', *, *, #41775, .T. ) ;
#37799 = CARTESIAN_POINT ( 'NONE',  ( 121.8725281442453223, -3.383040157471821630, -19.15922257007629170 ) ) ;
#37800 = CARTESIAN_POINT ( 'NONE',  ( 112.2857214775786474, -4.089484607189486809, -7.948022111789456723 ) ) ;
#37801 = CARTESIAN_POINT ( 'NONE',  ( 117.4478481442453131, -9.565557343593413364, -10.61323700422348004 ) ) ;
#37802 =( NAMED_UNIT ( * ) SI_UNIT ( $, .STERADIAN. ) SOLID_ANGLE_UNIT ( ) );
#37803 = LINE ( 'NONE', #44894, #19178 ) ;
#37804 = AXIS2_PLACEMENT_3D ( 'NONE', #24715, #31997, #760 ) ;
#37805 = CARTESIAN_POINT ( 'NONE',  ( 121.0783548109119749, 0.2603800115204892296, -16.42320221600525088 ) ) ;
#37806 = CARTESIAN_POINT ( 'NONE',  ( 119.7736414775786358, -10.30919188438810075, -12.61870101168855918 ) ) ;
#37807 = CARTESIAN_POINT ( 'NONE',  ( 116.1777233795247781, -8.938348069036489818, -17.46756447353520159 ) ) ;
#37808 = CARTESIAN_POINT ( 'NONE',  ( 113.5904348109119866, -2.084020599724406786, -8.691656652584148546 ) ) ;
#37809 = CARTESIAN_POINT ( 'NONE',  ( 69.90440230179062553, -25.79449873085293987, -5.893215200338315363 ) ) ;
#37810 = ORIENTED_EDGE ( 'NONE', *, *, #4687, .T. ) ;
#37811 = CARTESIAN_POINT ( 'NONE',  ( 118.1852948109119836, -5.638512984488999180, -18.83840828888717311 ) ) ;
#37812 = EDGE_CURVE ( 'NONE', #6454, #6765, #35272, .T. ) ;
#37813 = CARTESIAN_POINT ( 'NONE',  ( 121.9470836909669913, -27.84333996136784961, -14.15691383771150136 ) ) ;
#37814 = CARTESIAN_POINT ( 'NONE',  ( 117.2776681442452968, -5.638512984488999180, -18.83840828888717311 ) ) ;
#37815 = ORIENTED_EDGE ( 'NONE', *, *, #18587, .T. ) ;
#37816 = CARTESIAN_POINT ( 'NONE',  ( 124.1983214775786166, -8.166667518702819706, -8.995218007635861213 ) ) ;
#37817 = LINE ( 'NONE', #30532, #33973 ) ;
#37818 = CARTESIAN_POINT ( 'NONE',  ( 113.8740681442453138, -9.859900752359374465, -12.68260735090039404 ) ) ;
#37819 = DIRECTION ( 'NONE',  ( 0.000000000000000000, 0.000000000000000000, -1.000000000000000000 ) ) ;
#37820 = CARTESIAN_POINT ( 'NONE',  ( 115.2355081442453155, 0.1319031606808879209, -14.10382304977623669 ) ) ;
#37821 = DIRECTION ( 'NONE',  ( 0.9609149988134837450, -0.1028163501681639419, 0.2570431154366518145 ) ) ;
#37822 = CARTESIAN_POINT ( 'NONE',  ( 119.1496481442453046, -6.222761293078241884, -8.102969835052219238 ) ) ;
#37823 = CONICAL_SURFACE ( 'NONE', #7257, 2.000000000000000444, 0.9599310885968830309 ) ;
#37824 = CARTESIAN_POINT ( 'NONE',  ( 109.2294421295247844, 0.8460904216231607267, -14.64321520033831447 ) ) ;
#37825 = CARTESIAN_POINT ( 'NONE',  ( 115.3489614775786407, -0.8288870151387760510, -10.36305467784173118 ) ) ;
#37826 = CARTESIAN_POINT ( 'NONE',  ( 114.1577014775786552, -6.344957434206662583, -7.627207830600332805 ) ) ;
#37827 = CARTESIAN_POINT ( 'NONE',  ( 120.9936110609119737, -3.163656168406935087, -18.89861972220014508 ) ) ;
#37828 = AXIS2_PLACEMENT_3D ( 'NONE', #31660, #28258, #29600 ) ;
#37829 = CARTESIAN_POINT ( 'NONE',  ( 114.1009748109119784, -4.089484607189486809, -7.948022111789456723 ) ) ;
#37830 = CARTESIAN_POINT ( 'NONE',  ( 113.1366214775786432, -7.643976991954077427, -18.09477374809248928 ) ) ;
#37831 = CARTESIAN_POINT ( 'NONE',  ( 118.4689281442453392, -10.15424416112533912, -14.75197769757731336 ) ) ;
#37832 = ORIENTED_EDGE ( 'NONE', *, *, #6805, .F. ) ;
#37833 = CARTESIAN_POINT ( 'NONE',  ( 114.8384214775786489, 0.9020085738987339008, -11.91225656197089222 ) ) ;
#37834 = CARTESIAN_POINT ( 'NONE',  ( 106.6626452545248611, 0.8980012041604421569, -11.00651665394454071 ) ) ;
#37835 = EDGE_CURVE ( 'NONE', #21444, #23574, #138, .T. ) ;
#37836 = CYLINDRICAL_SURFACE ( 'NONE', #24085, 5.000000000000004441 ) ;
#37837 = CARTESIAN_POINT ( 'NONE',  ( 70.19189222814998175, -53.90613343638955968, -34.76527462071035046 ) ) ;
#37838 = DIRECTION ( 'NONE',  ( 0.000000000000000000, 0.9284778069183720062, 0.3713878862591650232 ) ) ;
#37839 = CARTESIAN_POINT ( 'NONE',  ( 123.0070614775786169, 0.9020085738987339008, -11.91225656197089222 ) ) ;
#37840 = ORIENTED_EDGE ( 'NONE', *, *, #15053, .T. ) ;
#37841 = VECTOR ( 'NONE', #22183, 1000.000000000000114 ) ;
#37842 = CARTESIAN_POINT ( 'NONE',  ( 135.3184548109119874, -7.252096815532139473, -18.89748516540533529 ) ) ;
#37843 = CARTESIAN_POINT ( 'NONE',  ( 119.7169148109119874, -0.1624402480850797581, -16.17319339645315424 ) ) ;
#37844 = EDGE_CURVE ( 'NONE', #7733, #14619, #38642, .T. ) ;
#37845 = DIRECTION ( 'NONE',  ( 0.000000000000000000, 0.000000000000000000, -1.000000000000000000 ) ) ;
#37846 = CARTESIAN_POINT ( 'NONE',  ( 122.6099748109119929, -9.261995988541697145, -16.69588392320189030 ) ) ;
#37847 = EDGE_CURVE ( 'NONE', #18952, #2128, #38254, .T. ) ;
#37848 = CARTESIAN_POINT ( 'NONE',  ( 106.0375671295248310, -10.62599879583958540, -13.39321520033831447 ) ) ;
#37849 = CARTESIAN_POINT ( 'NONE',  ( 89.03851648532334195, -10.64689777002964455, -14.14321520033831803 ) ) ;
#37850 = EDGE_LOOP ( 'NONE', ( #3760, #5311, #39822, #38865 ) ) ;
#37851 = FACE_OUTER_BOUND ( 'NONE', #38964, .T. ) ;
#37852 = CARTESIAN_POINT ( 'NONE',  ( 126.1270281442452870, 0.1319031606808879209, -14.10382304977623669 ) ) ;
#37853 = CARTESIAN_POINT ( 'NONE',  ( 122.3830681442452857, -8.166667518702819706, -8.995218007635861213 ) ) ;
#37854 = CARTESIAN_POINT ( 'NONE',  ( 116.0864081442453113, -0.1624402480850797581, -16.17319339645315424 ) ) ;
#37855 = CARTESIAN_POINT ( 'NONE',  ( 70.19189222814998175, -75.31442247550839397, -37.94335727672635983 ) ) ;
#37856 = CARTESIAN_POINT ( 'NONE',  ( 119.7736414775786358, -10.30919188438810075, -12.61870101168855918 ) ) ;
#37857 = DIRECTION ( 'NONE',  ( -0.9908103287288501093, 0.1352586133457976958, 0.000000000000000000 ) ) ;
#37858 = CARTESIAN_POINT ( 'NONE',  ( 126.3243314201119603, -1.068588705931508676, -10.05747113621685429 ) ) ;
#37859 = CARTESIAN_POINT ( 'NONE',  ( 122.2696148109119889, -5.574606645277164318, -18.38911715685844683 ) ) ;
#37860 = ORIENTED_EDGE ( 'NONE', *, *, #15081, .F. ) ;
#37861 = EDGE_CURVE ( 'NONE', #2441, #25522, #31813, .T. ) ;
#37862 = DIRECTION ( 'NONE',  ( 0.000000000000000000, 0.000000000000000000, -1.000000000000000000 ) ) ;
#37863 = CARTESIAN_POINT ( 'NONE',  ( 116.9940348109119839, -9.988377603198976828, -10.36322818467138340 ) ) ;
#37864 = CARTESIAN_POINT ( 'NONE',  ( 124.5954081442453116, -6.222761293078241884, -8.102969835052219238 ) ) ;
#37865 = VERTEX_POINT ( 'NONE', #27968 ) ;
#37866 = ADVANCED_FACE ( 'NONE', ( #7414 ), #3554, .F. ) ;
#37867 = CARTESIAN_POINT ( 'NONE',  ( 123.4939235609119663, 0.6414057260225851653, -11.69287257290600657 ) ) ;
#37868 = CARTESIAN_POINT ( 'NONE',  ( 136.3514896075954539, -1.238236687199658181, -8.849319055121297239 ) ) ;
#37869 = ADVANCED_FACE ( 'NONE', ( #38209 ), #14494, .T. ) ;
#37870 = EDGE_CURVE ( 'NONE', #38570, #41059, #17498, .T. ) ;
#37871 = CARTESIAN_POINT ( 'NONE',  ( 122.9503348109119827, 0.5811942927096110934, -14.16772938898807510 ) ) ;
#37872 = CARTESIAN_POINT ( 'NONE',  ( 107.0793640045248196, -10.62599879583958717, -11.00651665394454604 ) ) ;
#37873 = CARTESIAN_POINT ( 'NONE',  ( 120.3409081442453044, -8.899110576539710493, -16.42337572283490132 ) ) ;
#37874 = ORIENTED_EDGE ( 'NONE', *, *, #32414, .T. ) ;
#37875 = ORIENTED_EDGE ( 'NONE', *, *, #15813, .T. ) ;
#37876 = AXIS2_PLACEMENT_3D ( 'NONE', #15423, #29328, #1725 ) ;
#37877 = CARTESIAN_POINT ( 'NONE',  ( 124.8790414775786246, -8.899110576539710493, -16.42337572283490132 ) ) ;
#37878 = DIRECTION ( 'NONE',  ( -0.9609149988134834119, 0.1028163501681648995, -0.2570431154366529802 ) ) ;
#37879 = APPLICATION_CONTEXT ( 'automotive_design' ) ;
#37880 = PLANE ( 'NONE',  #36044 ) ;
#37881 = DIRECTION ( 'NONE',  ( 0.7871354856660198740, 0.4483307682966886643, 0.4235767337848242442 ) ) ;
#37882 = CARTESIAN_POINT ( 'NONE',  ( 121.2485348109119769, -0.4660016031367893996, -10.09054647747474043 ) ) ;
#37883 = FACE_OUTER_BOUND ( 'NONE', #7554, .T. ) ;
#37884 = CARTESIAN_POINT ( 'NONE',  ( 138.2184548109119930, -3.719473736431747390, -16.16631137400202078 ) ) ;
#37885 = CARTESIAN_POINT ( 'NONE',  ( 118.1285681442453068, -7.893985811506177619, -18.51759400769804742 ) ) ;
#37887 = CARTESIAN_POINT ( 'NONE',  ( 119.5467348109119712, -5.574606645277164318, -18.38911715685844683 ) ) ;
#37886 = CARTESIAN_POINT ( 'NONE',  ( 117.9016614775786280, -9.988377603198976828, -10.36322818467138340 ) ) ;
#37888 = CARTESIAN_POINT ( 'NONE',  ( 123.2906948109119867, -1.833838273342659697, -17.42832698103878286 ) ) ;
#37889 = CARTESIAN_POINT ( 'NONE',  ( 116.0864081442453113, -9.988377603198976828, -10.36322818467138340 ) ) ;
#37890 = ORIENTED_EDGE ( 'NONE', *, *, #3188, .T. ) ;
#37891 = CARTESIAN_POINT ( 'NONE',  ( 125.8433948109119456, -7.643976991954077427, -18.09477374809248928 ) ) ;
#37892 = CARTESIAN_POINT ( 'NONE',  ( 125.0954081442453401, -3.517672760958747702, -18.63504008191803152 ) ) ;
#37893 = CARTESIAN_POINT ( 'NONE',  ( 107.2182702545248105, -10.62599879583958717, -15.77991374673208469 ) ) ;
#37894 = CARTESIAN_POINT ( 'NONE',  ( 108.5378796295247810, -4.863998795839590272, -8.388885654883775800 ) ) ;
#37895 = CARTESIAN_POINT ( 'NONE',  ( 109.0935046295247872, -4.863998795839590272, -7.631215200338315796 ) ) ;
#37896 = VECTOR ( 'NONE', #5858, 1000.000000000000000 ) ;
#37897 = CARTESIAN_POINT ( 'NONE',  ( 120.5678148109119832, -8.166667518702819706, -8.995218007635861213 ) ) ;
#37898 = CARTESIAN_POINT ( 'NONE',  ( 123.9146881442452894, -10.15424416112533912, -14.75197769757731336 ) ) ;
#37899 = EDGE_LOOP ( 'NONE', ( #32411, #2083, #24175, #38170 ) ) ;
#37900 = CARTESIAN_POINT ( 'NONE',  ( 124.3685014775786328, -10.63000616557722466, -14.87417383870573495 ) ) ;
#37901 = CARTESIAN_POINT ( 'NONE',  ( 112.2883483795247770, -0.7896495226426338832, -9.318865927141430916 ) ) ;
#37902 = CARTESIAN_POINT ( 'NONE',  ( 59.24641515291911986, -13.72835195454734425, -19.39321520033831803 ) ) ;
#37903 = CARTESIAN_POINT ( 'NONE',  ( 124.4819548109119722, -7.893985811506177619, -18.51759400769804742 ) ) ;
#37904 = CARTESIAN_POINT ( 'NONE',  ( 119.4900081442453086, -1.834011780172310813, -8.268836392978581529 ) ) ;
#37905 = CARTESIAN_POINT ( 'NONE',  ( 120.0212673109119805, -9.289237151508434209, -11.05642687123711276 ) ) ;
#37906 = CARTESIAN_POINT ( 'NONE',  ( 113.4202548109119846, -10.30919188438810075, -12.61870101168855918 ) ) ;
#37907 = CARTESIAN_POINT ( 'NONE',  ( 123.2161110609119703, -6.340755971794695078, -8.611740276972781771 ) ) ;
#37908 = CARTESIAN_POINT ( 'NONE',  ( 115.6915515045247531, -6.936859964151250502, -18.39754474579286025 ) ) ;
#37909 = ORIENTED_EDGE ( 'NONE', *, *, #23332, .F. ) ;
#37910 = CARTESIAN_POINT ( 'NONE',  ( 125.0125860817262122, -2.423081321603731908, -17.89265170041263175 ) ) ;
#37911 = AXIS2_PLACEMENT_3D ( 'NONE', #28383, #11058, #3974 ) ;
#37912 = CARTESIAN_POINT ( 'NONE',  ( 114.3505409221557443, -2.372251574601226043, -17.96033910819752322 ) ) ;
#37913 = CARTESIAN_POINT ( 'NONE',  ( 112.0020881442453344, 0.2603800115204892296, -16.42320221600525088 ) ) ;
#37914 = CARTESIAN_POINT ( 'NONE',  ( 108.1211608795247798, -1.325403438956436419, -16.93181055722141792 ) ) ;
#37915 = CARTESIAN_POINT ( 'NONE',  ( 105.6903015045248253, -6.936859964151250502, -18.39754474579286025 ) ) ;
#37916 = VECTOR ( 'NONE', #15873, 1000.000000000000000 ) ;
#37917 = CARTESIAN_POINT ( 'NONE',  ( 120.0572748109119772, -6.222761293078241884, -8.102969835052219238 ) ) ;
#37918 = PRODUCT_DEFINITION_CONTEXT ( 'detailed design', #23302, 'design' ) ;
#37919 = CARTESIAN_POINT ( 'NONE',  ( 115.9729548109119861, -3.505236298600246325, -18.68346056562440793 ) ) ;
#37920 = CARTESIAN_POINT ( 'NONE',  ( 113.0231681442453180, -10.15424416112533912, -14.75197769757731336 ) ) ;
#37921 = ORIENTED_EDGE ( 'NONE', *, *, #30678, .F. ) ;
#37922 = ADVANCED_FACE ( 'NONE', ( #26101 ), #8552, .F. ) ;
#37923 = CARTESIAN_POINT ( 'NONE',  ( 121.6186891859119896, -1.406689858478933353, -17.56299727309130887 ) ) ;
#37924 = CARTESIAN_POINT ( 'NONE',  ( 119.4900081442453086, -1.834011780172310813, -8.268836392978581529 ) ) ;
#37925 = CARTESIAN_POINT ( 'NONE',  ( 121.3655035264548872, -8.247323210606168686, -17.08054893949881148 ) ) ;
#37926 = EDGE_LOOP ( 'NONE', ( #32616, #17637, #21594, #15552 ) ) ;
#37927 = CARTESIAN_POINT ( 'NONE',  ( 126.2597653975841325, -9.021097607470126789, -16.20867439364996088 ) ) ;
#37928 = EDGE_CURVE ( 'NONE', #21122, #35115, #35316, .T. ) ;
#37929 = VERTEX_POINT ( 'NONE', #21786 ) ;
#37930 = ADVANCED_FACE ( 'NONE', ( #22453 ), #11532, .F. ) ;
#37931 = AXIS2_PLACEMENT_3D ( 'NONE', #38274, #11153, #14119 ) ;
#37932 = CARTESIAN_POINT ( 'NONE',  ( 113.2500748109119968, -3.505236298600246325, -18.68346056562440793 ) ) ;
#37933 = CARTESIAN_POINT ( 'NONE',  ( 115.3489614775786407, -0.8288870151387760510, -10.36305467784173118 ) ) ;
#37934 = EDGE_CURVE ( 'NONE', #24250, #20548, #36124, .T. ) ;
#37935 = CARTESIAN_POINT ( 'NONE',  ( 84.77016061404391678, -25.99489077589524300, -13.39321520033831625 ) ) ;
#37936 = CARTESIAN_POINT ( 'NONE',  ( 120.2990798109119766, -2.173413727453600508, -8.297982527556802879 ) ) ;
#37937 = ORIENTED_EDGE ( 'NONE', *, *, #20073, .T. ) ;
#37938 = DIRECTION ( 'NONE',  ( 1.000000000000000000, 0.000000000000000000, -0.000000000000000000 ) ) ;
#37939 = CARTESIAN_POINT ( 'NONE',  ( 62.66445125428926843, -3.444971829879546643, -7.594369504596270026 ) ) ;
#37940 = CARTESIAN_POINT ( 'NONE',  ( 115.6915515045247531, -2.477300249445798297, -7.631215200338321125 ) ) ;
#37941 = AXIS2_PLACEMENT_3D ( 'NONE', #28502, #29162, #14362 ) ;
#37942 = CARTESIAN_POINT ( 'NONE',  ( 115.9947331777918862, -0.01829820670803256055, -14.64321520033831447 ) ) ;
#37943 = AXIS2_PLACEMENT_3D ( 'NONE', #40082, #5637, #2214 ) ;
#37944 = CARTESIAN_POINT ( 'NONE',  ( 124.7088614775786226, -9.565557343593413364, -10.61323700422348004 ) ) ;
#37945 = CARTESIAN_POINT ( 'NONE',  ( 113.0798948109119948, -8.899110576539710493, -16.42337572283490132 ) ) ;
#37946 = CARTESIAN_POINT ( 'NONE',  ( 120.0549121015961163, -1.040089454026960292, -17.23633227186633476 ) ) ;
#37947 = EDGE_LOOP ( 'NONE', ( #25515, #4345, #23974, #2937 ) ) ;
#37948 = DIRECTION ( 'NONE',  ( 1.000000000000000000, 0.000000000000000000, -0.000000000000000000 ) ) ;
#37949 = CARTESIAN_POINT ( 'NONE',  ( 112.3424481442453384, -3.505236298600246325, -18.68346056562440793 ) ) ;
#37950 = FACE_OUTER_BOUND ( 'NONE', #43378, .T. ) ;
#37951 = FACE_OUTER_BOUND ( 'NONE', #41979, .T. ) ;
#37953 = DIRECTION ( 'NONE',  ( 0.5735764363510498232, -0.3127926500124802445, 0.7570804645221007600 ) ) ;
#37952 = CARTESIAN_POINT ( 'NONE',  ( 65.34289968162609341, -37.75951406093616214, -4.893215200338314474 ) ) ;
#37954 = CARTESIAN_POINT ( 'NONE',  ( 124.9924948109119924, -5.574606645277164318, -18.38911715685844683 ) ) ;
#37955 = EDGE_LOOP ( 'NONE', ( #12190, #29227, #38757, #43745, #41465 ) ) ;
#37956 = CARTESIAN_POINT ( 'NONE',  ( 113.6471614775786492, -5.638512984488999180, -18.83840828888717311 ) ) ;
#37957 = CARTESIAN_POINT ( 'NONE',  ( 126.5621572004088051, 0.1111755995133630603, -14.80766266791229135 ) ) ;
#37958 = CARTESIAN_POINT ( 'NONE',  ( 107.4266296295248821, -4.863998795839590272, -8.388885654883775800 ) ) ;
#37959 = CARTESIAN_POINT ( 'NONE',  ( 126.2404814775786264, -0.8288870151387760510, -10.36305467784173118 ) ) ;
#37960 = CARTESIAN_POINT ( 'NONE',  ( 124.4819548109119722, -2.084020599724406786, -8.691656652584148546 ) ) ;
#37961 = DIRECTION ( 'NONE',  ( -1.000000000000000000, 0.000000000000000000, 0.000000000000000000 ) ) ;
#37962 = CARTESIAN_POINT ( 'NONE',  ( 110.4131140045248287, 0.1403307496149616695, -15.46607636864997204 ) ) ;
#37963 = DIRECTION ( 'NONE',  ( -0.000000000000000000, -0.9284778069183718952, -0.3713878862591649677 ) ) ;
#37964 = CARTESIAN_POINT ( 'NONE',  ( 62.92618109310924268, -32.76310523276723785, -23.89321520033831803 ) ) ;
#37965 = AXIS2_PLACEMENT_3D ( 'NONE', #1397, #25362, #29442 ) ;
#37966 = CARTESIAN_POINT ( 'NONE',  ( 114.1577014775786552, -3.505236298600246325, -18.68346056562440793 ) ) ;
#37967 = CARTESIAN_POINT ( 'NONE',  ( 107.0793640045248196, -10.62599879583958717, -11.00651665394454604 ) ) ;
#37968 = DIRECTION ( 'NONE',  ( 0.000000000000000000, -0.3818493186865927203, 0.9242245927363029745 ) ) ;
#37969 = CARTESIAN_POINT ( 'NONE',  ( 108.5378796295247810, -4.863998795839590272, -19.15521520033831493 ) ) ;
#37970 = CARTESIAN_POINT ( 'NONE',  ( 123.6310548109119765, -5.638512984488999180, -18.83840828888717311 ) ) ;
#37971 = CARTESIAN_POINT ( 'NONE',  ( 112.2289948109119848, -7.643976991954077427, -18.09477374809248928 ) ) ;
#37972 = CARTESIAN_POINT ( 'NONE',  ( 111.9181031537514741, 0.4930828106259610433, -14.64321520033831447 ) ) ;
#37973 = CARTESIAN_POINT ( 'NONE',  ( 120.7947214775786193, -9.261995988541697145, -16.69588392320189030 ) ) ;
#37974 = CARTESIAN_POINT ( 'NONE',  ( 117.6747548109119919, -1.834011780172310813, -8.268836392978581529 ) ) ;
#37976 = ORIENTED_EDGE ( 'NONE', *, *, #6053, .F. ) ;
#37975 = EDGE_CURVE ( 'NONE', #2531, #23514, #42984, .T. ) ;
#37977 = CARTESIAN_POINT ( 'NONE',  ( 111.7751814775786556, -2.084020599724406786, -8.691656652584148546 ) ) ;
#37978 = VECTOR ( 'NONE', #32172, 1000.000000000000000 ) ;
#37979 = CARTESIAN_POINT ( 'NONE',  ( 123.5743281442453139, -7.893985811506177619, -18.51759400769804742 ) ) ;
#37980 = CARTESIAN_POINT ( 'NONE',  ( 114.0442481442453300, -1.834011780172310813, -8.268836392978581529 ) ) ;
#37981 = CARTESIAN_POINT ( 'NONE',  ( 116.9373081442452929, -1.833838273342659253, -17.42832698103878286 ) ) ;
#37982 = ORIENTED_EDGE ( 'NONE', *, *, #3000, .F. ) ;
#37983 = CARTESIAN_POINT ( 'NONE',  ( 119.0361948109119652, -2.084020599724406786, -8.691656652584148546 ) ) ;
#37984 = CARTESIAN_POINT ( 'NONE',  ( 117.6180281442453150, -0.4660016031367893996, -10.09054647747474043 ) ) ;
#37985 = ADVANCED_FACE ( 'NONE', ( #8329 ), #4451, .F. ) ;
#37986 = CARTESIAN_POINT ( 'NONE',  ( 123.5176014775786228, -0.8288870151387760510, -10.36305467784173118 ) ) ;
#37987 = CARTESIAN_POINT ( 'NONE',  ( 116.8583982284553144, -0.4292963591166082393, -16.22917518106288881 ) ) ;
#37988 = CARTESIAN_POINT ( 'NONE',  ( 113.9552233795247815, -8.938348069036489818, -17.46756447353520159 ) ) ;
#37989 = ORIENTED_EDGE ( 'NONE', *, *, #6249, .T. ) ;
#37990 = FACE_OUTER_BOUND ( 'NONE', #29312, .T. ) ;
#37991 = CARTESIAN_POINT ( 'NONE',  ( 125.7866681442452688, -0.4660016031367893996, -10.09054647747474043 ) ) ;
#37992 = CARTESIAN_POINT ( 'NONE',  ( 116.1777233795247781, -1.325403438956436419, -9.854619843455211026 ) ) ;
#37993 = VECTOR ( 'NONE', #18238, 1000.000000000000000 ) ;
#37994 = CARTESIAN_POINT ( 'NONE',  ( 117.3719165460472027, -2.191907684172563986, -18.20049396185734025 ) ) ;
#37995 = CARTESIAN_POINT ( 'NONE',  ( 117.0736591576486774, 1.652729585752748198, -5.467741361931248711 ) ) ;
#37996 = DIRECTION ( 'NONE',  ( -0.2768435750659241079, -0.3568721902840695792, 0.8921882507333129819 ) ) ;
#37997 = CARTESIAN_POINT ( 'NONE',  ( 107.7044421295247929, -9.868328341294093420, -13.39321520033831447 ) ) ;
#37998 = CARTESIAN_POINT ( 'NONE',  ( 115.3993696192402325, -1.111561923218680858, -17.14115599315434935 ) ) ;
#37999 = CARTESIAN_POINT ( 'NONE',  ( 117.8449348109119938, -8.166667518702817929, -8.995218007635861213 ) ) ;
#38000 = CARTESIAN_POINT ( 'NONE',  ( 35.67453213195965134, -67.60842401891365228, -7.393215200338315363 ) ) ;
#38001 = VECTOR ( 'NONE', #4741, 1000.000000000000000 ) ;
#38002 = DIRECTION ( 'NONE',  ( -0.2768435750659253847, -0.3568721902840677473, 0.8921882507333133150 ) ) ;
#38003 = EDGE_CURVE ( 'NONE', #5526, #20846, #40008, .T. ) ;
#38004 = DIRECTION ( 'NONE',  ( 1.000000000000000000, 0.000000000000000000, 0.000000000000000000 ) ) ;
#38005 = CARTESIAN_POINT ( 'NONE',  ( 120.9649014775786355, -6.222761293078241884, -8.102969835052219238 ) ) ;
#38006 = EDGE_LOOP ( 'NONE', ( #7516, #14013, #12521, #6428 ) ) ;
#38007 = CARTESIAN_POINT ( 'NONE',  ( 125.3895814775786448, -7.893985811506177619, -18.51759400769804742 ) ) ;
#38008 = CARTESIAN_POINT ( 'NONE',  ( 117.5613014775786525, 0.9020085738987339008, -11.91225656197089222 ) ) ;
#38009 = CARTESIAN_POINT ( 'NONE',  ( 117.0806140045248185, 0.1403307496149616695, -15.46607636864997204 ) ) ;
#38010 = CARTESIAN_POINT ( 'NONE',  ( 117.1642148109119859, -0.8288870151387760510, -10.36305467784173118 ) ) ;
#38011 = CARTESIAN_POINT ( 'NONE',  ( 126.0135748109119902, -8.166667518702819706, -8.995218007635861213 ) ) ;
#38012 = CARTESIAN_POINT ( 'NONE',  ( 111.3854577545248645, -7.250697342233347165, -7.631215200338321125 ) ) ;
#38013 = CARTESIAN_POINT ( 'NONE',  ( 105.4819421295248247, -9.868328341294093420, -13.39321520033831447 ) ) ;
#38014 = CARTESIAN_POINT ( 'NONE',  ( 82.84471951188260164, -31.80328994127697939, -23.17386122141205718 ) ) ;
#38015 = CARTESIAN_POINT ( 'NONE',  ( 118.4122014775786340, -9.859900752359374465, -12.68260735090039404 ) ) ;
#38016 = CARTESIAN_POINT ( 'NONE',  ( 120.5678148109119832, -1.833838273342659253, -17.42832698103878286 ) ) ;
#38017 = DIRECTION ( 'NONE',  ( 0.000000000000000000, 0.000000000000000000, -1.000000000000000000 ) ) ;
#38018 = CARTESIAN_POINT ( 'NONE',  ( 122.2437673109119629, 0.2312338769422704887, -16.08380026872395874 ) ) ;
#38019 = CARTESIAN_POINT ( 'NONE',  ( 109.9269421295247753, -9.868328341294093420, -13.39321520033831447 ) ) ;
#38020 = DIRECTION ( 'NONE',  ( 1.000000000000000000, 0.000000000000000000, -0.000000000000000000 ) ) ;
#38021 = CARTESIAN_POINT ( 'NONE',  ( 115.5191414775786569, -3.383040157471821630, -19.15922257007629170 ) ) ;
#38022 = CARTESIAN_POINT ( 'NONE',  ( 113.0231681442453322, 0.9020085738987339008, -11.91225656197089222 ) ) ;
#38023 = DIRECTION ( 'NONE',  ( -0.000000000000000000, -0.9284778069183718952, -0.3713878862591649677 ) ) ;
#38024 = VERTEX_POINT ( 'NONE', #28857 ) ;
#38025 = CARTESIAN_POINT ( 'NONE',  ( 123.6451722564640079, -3.285188920618888897, -14.24668229758334803 ) ) ;
#38026 = EDGE_LOOP ( 'NONE', ( #24969, #44105, #5569, #22992, #37921 ) ) ;
#38027 = CARTESIAN_POINT ( 'NONE',  ( 121.0783548109119749, 0.2603800115204892296, -16.42320221600525088 ) ) ;
#38028 = VECTOR ( 'NONE', #20474, 1000.000000000000114 ) ;
#38029 = CARTESIAN_POINT ( 'NONE',  ( 114.7249681442453237, 0.2603800115204892296, -16.42320221600525088 ) ) ;
#38030 = CARTESIAN_POINT ( 'NONE',  ( 117.6180281442453150, -8.899110576539710493, -16.42337572283490132 ) ) ;
#38031 = CARTESIAN_POINT ( 'NONE',  ( 91.77400275106518279, -24.14644159042263993, -12.62951656296512937 ) ) ;
#38032 = CARTESIAN_POINT ( 'NONE',  ( 123.6310548109119765, -5.638512984488999180, -18.83840828888717311 ) ) ;
#38033 = CARTESIAN_POINT ( 'NONE',  ( 118.4689281442453392, 0.9020085738987339008, -11.91225656197089222 ) ) ;
#38034 = CARTESIAN_POINT ( 'NONE',  ( 107.7044421295247929, -9.868328341294093420, -13.39321520033831447 ) ) ;
#38035 = CIRCLE ( 'NONE', #39503, 33.80000000000000426 ) ;
#38036 = EDGE_CURVE ( 'NONE', #40192, #26749, #18373, .T. ) ;
#38037 = CARTESIAN_POINT ( 'NONE',  ( 112.2289948109119848, -7.643976991954077427, -18.09477374809248928 ) ) ;
#38038 = CARTESIAN_POINT ( 'NONE',  ( 94.20708369096698220, -25.99489077589524300, -13.39321520033831447 ) ) ;
#38039 = ORIENTED_EDGE ( 'NONE', *, *, #276, .F. ) ;
#38040 = CARTESIAN_POINT ( 'NONE',  ( 117.3343948109119737, -3.383040157471821630, -19.15922257007629170 ) ) ;
#38041 = LINE ( 'NONE', #406, #8191 ) ;
#38042 = CARTESIAN_POINT ( 'NONE',  ( 116.4267681442453153, -3.383040157471821630, -19.15922257007629170 ) ) ;
#38043 = ORIENTED_EDGE ( 'NONE', *, *, #2447, .T. ) ;
#38044 = CARTESIAN_POINT ( 'NONE',  ( 114.3024890045248156, 0.8980012041604421569, -15.77991374673208469 ) ) ;
#38045 = CARTESIAN_POINT ( 'NONE',  ( 123.9146881442452894, 0.9020085738987339008, -11.91225656197089222 ) ) ;
#38046 = DIRECTION ( 'NONE',  ( 0.000000000000000000, 0.9554676365605390131, 0.2950959089608289343 ) ) ;
#38047 = CARTESIAN_POINT ( 'NONE',  ( 113.4769814775786330, 0.4262465694468514643, -12.03445270309931736 ) ) ;
#38048 = CARTESIAN_POINT ( 'NONE',  ( 78.02189457680029250, -57.61239323309698790, -1.007362850241582786 ) ) ;
#38049 = CARTESIAN_POINT ( 'NONE',  ( 116.1998614775786507, 0.4262465694468514643, -12.03445270309931736 ) ) ;
#38050 = CARTESIAN_POINT ( 'NONE',  ( 66.06194382436763135, -14.97931106434683635, -21.89321520033831447 ) ) ;
#38051 = CARTESIAN_POINT ( 'NONE',  ( 116.0864081442453113, -0.1624402480850797581, -16.17319339645315424 ) ) ;
#38052 = AXIS2_PLACEMENT_3D ( 'NONE', #13577, #41177, #37272 ) ;
#38053 = DIRECTION ( 'NONE',  ( -0.2768435750659239414, -0.3568721902840664151, 0.8921882507333142032 ) ) ;
#38054 = CARTESIAN_POINT ( 'NONE',  ( 120.0572748109119772, -6.222761293078241884, -8.102969835052219238 ) ) ;
#38055 = CARTESIAN_POINT ( 'NONE',  ( 121.8270485609119760, -10.36940331770106916, -15.09355782777062061 ) ) ;
#38056 = CARTESIAN_POINT ( 'NONE',  ( 116.4267681442453153, -3.383040157471821630, -19.15922257007629170 ) ) ;
#38057 = CARTESIAN_POINT ( 'NONE',  ( 112.3991748109119868, -1.833838273342658809, -17.42832698103878286 ) ) ;
#38058 = CARTESIAN_POINT ( 'NONE',  ( 115.9729548109119861, -3.505236298600246325, -18.68346056562440793 ) ) ;
#38059 = EDGE_LOOP ( 'NONE', ( #23322, #20598, #18072, #15356, #29685 ) ) ;
#38060 = CARTESIAN_POINT ( 'NONE',  ( 118.2987481442453088, -1.561330072975668504, -17.79121239304076951 ) ) ;
#38061 = CARTESIAN_POINT ( 'NONE',  ( 109.5796765045248122, -7.250697342233347165, -19.15521520033831138 ) ) ;
#38062 = CARTESIAN_POINT ( 'NONE',  ( 105.7597546295248350, -4.863998795839590272, -18.39754474579285315 ) ) ;
#38063 = AXIS2_PLACEMENT_3D ( 'NONE', #29519, #37015, #15844 ) ;
#38064 = DIRECTION ( 'NONE',  ( 1.000000000000000000, 0.000000000000000000, 0.000000000000000000 ) ) ;
#38065 = PLANE ( 'NONE',  #10215 ) ;
#38066 = CARTESIAN_POINT ( 'NONE',  ( 122.0427081442452817, 0.5811942927096110934, -14.16772938898807510 ) ) ;
#38067 = ORIENTED_EDGE ( 'NONE', *, *, #15652, .T. ) ;
#38068 = DIRECTION ( 'NONE',  ( 0.000000000000000000, 0.000000000000000000, 1.000000000000000000 ) ) ;
#38069 = CARTESIAN_POINT ( 'NONE',  ( 118.0718414775786442, -0.8288870151387760510, -10.36305467784173118 ) ) ;
#38070 = LINE ( 'NONE', #38284, #22663 ) ;
#38071 = CARTESIAN_POINT ( 'NONE',  ( 124.4819548109119722, -7.893985811506177619, -18.51759400769804742 ) ) ;
#38072 = CARTESIAN_POINT ( 'NONE',  ( 111.6632702545248605, 0.1403307496149616695, -11.32035403202665336 ) ) ;
#38073 = CARTESIAN_POINT ( 'NONE',  ( 89.28219092212185615, -9.933696230371026559, -13.53880969525256184 ) ) ;
#38074 = ORIENTED_EDGE ( 'NONE', *, *, #34491, .T. ) ;
#38075 = FACE_OUTER_BOUND ( 'NONE', #2234, .T. ) ;
#38076 = CARTESIAN_POINT ( 'NONE',  ( 126.2972081442452890, -2.084020599724406786, -8.691656652584148546 ) ) ;
#38077 = CARTESIAN_POINT ( 'NONE',  ( 122.8368814775786291, -1.561330072975668948, -17.79121239304076951 ) ) ;
#38078 = CARTESIAN_POINT ( 'NONE',  ( 115.5758681442453053, -7.894159318335828068, -9.358103419637847864 ) ) ;
#38079 = FACE_OUTER_BOUND ( 'NONE', #23137, .T. ) ;
#38080 = CARTESIAN_POINT ( 'NONE',  ( 120.5678148109119832, -8.166667518702819706, -8.995218007635861213 ) ) ;
#38081 = DIRECTION ( 'NONE',  ( -0.2768435750659239414, -0.3568721902840664151, 0.8921882507333142032 ) ) ;
#38082 = CARTESIAN_POINT ( 'NONE',  ( 121.5321681442453183, -0.1624402480850797581, -16.17319339645315424 ) ) ;
#38083 = ORIENTED_EDGE ( 'NONE', *, *, #23688, .F. ) ;
#38084 = AXIS2_PLACEMENT_3D ( 'NONE', #23277, #9144, #16217 ) ;
#38085 = CARTESIAN_POINT ( 'NONE',  ( 116.5945891742730822, -9.863394354262339903, -13.30644683333167855 ) ) ;
#38086 = CIRCLE ( 'NONE', #33711, 33.80000000000000426 ) ;
#38087 = CARTESIAN_POINT ( 'NONE',  ( 116.0864081442453113, -9.988377603198976828, -10.36322818467138340 ) ) ;
#38088 = CARTESIAN_POINT ( 'NONE',  ( 124.3685014775786328, 0.4262465694468514643, -12.03445270309931736 ) ) ;
#38089 = ORIENTED_EDGE ( 'NONE', *, *, #36192, .F. ) ;
#38090 = CARTESIAN_POINT ( 'NONE',  ( 120.8547048109119686, -7.554583864224885481, -18.48844787311982785 ) ) ;
#38091 = DIRECTION ( 'NONE',  ( 0.4225728684367167087, -0.9063289528979890930, -0.000000000000000000 ) ) ;
#38092 = CARTESIAN_POINT ( 'NONE',  ( 122.5532481442453019, -10.63000616557722466, -14.87417383870573495 ) ) ;
#38093 = CARTESIAN_POINT ( 'NONE',  ( 106.7320983795247855, -0.7896495226426338832, -9.318865927141430916 ) ) ;
#38094 = CARTESIAN_POINT ( 'NONE',  ( 121.0216281442452981, -7.894159318335828068, -9.358103419637847864 ) ) ;
#38095 = EDGE_CURVE ( 'NONE', #33768, #6720, #18810, .T. ) ;
#38096 = ORIENTED_EDGE ( 'NONE', *, *, #22804, .T. ) ;
#38097 = VECTOR ( 'NONE', #40520, 1000.000000000000000 ) ;
#38098 = VERTEX_POINT ( 'NONE', #10093 ) ;
#38099 = CARTESIAN_POINT ( 'NONE',  ( 115.1787814775786387, -9.988377603198976828, -10.36322818467138340 ) ) ;
#38100 = CARTESIAN_POINT ( 'NONE',  ( 123.5176014775786228, -0.8288870151387760510, -10.36305467784173118 ) ) ;
#38101 = DIRECTION ( 'NONE',  ( 0.000000000000000000, -0.7142857142857143016, 0.6998542122237653151 ) ) ;
#38102 = EDGE_CURVE ( 'NONE', #38550, #13151, #41707, .T. ) ;
#38103 = CARTESIAN_POINT ( 'NONE',  ( 122.4965214775786251, -10.30919188438810075, -12.61870101168855918 ) ) ;
#38104 = CARTESIAN_POINT ( 'NONE',  ( 111.3403343090046889, -8.955484211904590097, -16.47405415812863083 ) ) ;
#38105 = CARTESIAN_POINT ( 'NONE',  ( 118.3554748109119998, 0.2603800115204892296, -16.42320221600525088 ) ) ;
#38107 = CARTESIAN_POINT ( 'NONE',  ( 121.0783548109119749, -9.565557343593413364, -10.61323700422348004 ) ) ;
#38106 = CARTESIAN_POINT ( 'NONE',  ( 119.6601881442453106, -8.166667518702819706, -8.995218007635861213 ) ) ;
#38108 = DIRECTION ( 'NONE',  ( 0.9908103287288504424, -0.1352586133457952533, 0.000000000000000000 ) ) ;
#38109 = CARTESIAN_POINT ( 'NONE',  ( 117.1074881442453233, -10.63000616557722466, -14.87417383870573495 ) ) ;
#38110 = EDGE_LOOP ( 'NONE', ( #3021, #28647, #6406, #13159, #44803 ) ) ;
#38111 = EDGE_CURVE ( 'NONE', #32144, #18453, #37664, .T. ) ;
#38112 = CARTESIAN_POINT ( 'NONE',  ( 89.12784890491134604, -25.23119213852205789, -15.24166438581092109 ) ) ;
#38113 = CARTESIAN_POINT ( 'NONE',  ( 107.6349890045248401, 0.8980012041604421569, -15.77991374673208469 ) ) ;
#38114 = CIRCLE ( 'NONE', #263, 2.541999999999999371 ) ;
#38115 = CARTESIAN_POINT ( 'NONE',  ( 108.8851452545248151, -9.868328341294098749, -15.46607636864997204 ) ) ;
#38116 = CARTESIAN_POINT ( 'NONE',  ( 106.1764733795248219, -8.938348069036489818, -17.46756447353520159 ) ) ;
#38117 = CARTESIAN_POINT ( 'NONE',  ( 125.2194014775786286, -10.30919188438810075, -12.61870101168855918 ) ) ;
#38118 = CARTESIAN_POINT ( 'NONE',  ( 113.2500748109119968, -6.344957434206662583, -7.627207830600332805 ) ) ;
#38119 = VERTEX_POINT ( 'NONE', #10528 ) ;
#38120 = ADVANCED_FACE ( 'NONE', ( #34232 ), #14255, .T. ) ;
#38121 = CARTESIAN_POINT ( 'NONE',  ( 111.2646414775786496, -8.899110576539710493, -16.42337572283490132 ) ) ;
#38122 = CARTESIAN_POINT ( 'NONE',  ( 109.4407702545248355, -10.62599879583958717, -15.77991374673208469 ) ) ;
#38123 = PLANE ( 'NONE',  #27074 ) ;
#38124 = CARTESIAN_POINT ( 'NONE',  ( 123.4041481442452834, -10.30919188438810075, -12.61870101168855918 ) ) ;
#38125 = EDGE_CURVE ( 'NONE', #5080, #34215, #29513, .T. ) ;
#38126 = ADVANCED_FACE ( 'NONE', ( #30597 ), #252, .T. ) ;
#38127 = CARTESIAN_POINT ( 'NONE',  ( 124.7655881442452852, 0.5811942927096110934, -14.16772938898807510 ) ) ;
#38128 = DIRECTION ( 'NONE',  ( -0.1352586133457951423, -0.9908103287288504424, 0.000000000000000000 ) ) ;
#38129 = CARTESIAN_POINT ( 'NONE',  ( 112.7962614775786676, -3.383040157471821630, -19.15922257007629170 ) ) ;
#38130 = PLANE ( 'NONE',  #32060 ) ;
#38131 = CARTESIAN_POINT ( 'NONE',  ( 106.5931921295248372, 0.8980012041604618078, -13.39321520033831447 ) ) ;
#38132 = VERTEX_POINT ( 'NONE', #23996 ) ;
#38133 = CIRCLE ( 'NONE', #38867, 2.000000000000000444 ) ;
#38134 = DIRECTION ( 'NONE',  ( 0.000000000000000000, 0.000000000000000000, -1.000000000000000000 ) ) ;
#38135 = CARTESIAN_POINT ( 'NONE',  ( 114.3278814775786429, 0.1319031606808879209, -14.10382304977623669 ) ) ;
#38136 = CARTESIAN_POINT ( 'NONE',  ( 112.7395348109119766, -5.638512984488999180, -18.83840828888717311 ) ) ;
#38137 = CARTESIAN_POINT ( 'NONE',  ( 113.8857702545248003, -10.62599879583958717, -15.77991374673208469 ) ) ;
#38138 = CARTESIAN_POINT ( 'NONE',  ( 108.3989733795248753, -1.325403438956436419, -9.854619843455211026 ) ) ;
#38139 = CARTESIAN_POINT ( 'NONE',  ( 120.2274548109119934, -9.859900752359378018, -12.68260735090039759 ) ) ;
#38140 = CARTESIAN_POINT ( 'NONE',  ( 116.7104014775786425, -8.899110576539710493, -16.42337572283490132 ) ) ;
#38141 = CARTESIAN_POINT ( 'NONE',  ( 112.8529881442453160, -7.894159318335828068, -9.358103419637847864 ) ) ;
#38142 = ORIENTED_EDGE ( 'NONE', *, *, #19698, .F. ) ;
#38143 = CARTESIAN_POINT ( 'NONE',  ( 121.8270485609119760, -0.08252387247370887580, -11.91645802438286417 ) ) ;
#38144 = CYLINDRICAL_SURFACE ( 'NONE', #16417, 1.299999999999995604 ) ;
#38145 = CARTESIAN_POINT ( 'NONE',  ( 114.7249681442453237, -9.565557343593413364, -10.61323700422348004 ) ) ;
#38146 = VERTEX_POINT ( 'NONE', #37884 ) ;
#38147 = CYLINDRICAL_SURFACE ( 'NONE', #44233, 1.587500000000000577 ) ;
#38148 = TOROIDAL_SURFACE ( 'NONE', #6126, 6.500000000000000000, 1.500000000000000000 ) ;
#38149 = ADVANCED_FACE ( 'NONE', ( #20570 ), #13279, .T. ) ;
#38150 = VERTEX_POINT ( 'NONE', #34447 ) ;
#38151 = CARTESIAN_POINT ( 'NONE',  ( 117.1642148109119859, -0.8288870151387760510, -10.36305467784173118 ) ) ;
#38152 = CARTESIAN_POINT ( 'NONE',  ( 114.7249681442453237, -9.565557343593413364, -10.61323700422348004 ) ) ;
#38153 = DIRECTION ( 'NONE',  ( 1.000000000000000000, 0.000000000000000000, 0.000000000000000000 ) ) ;
#38154 = CARTESIAN_POINT ( 'NONE',  ( 124.6746266859119743, -9.033780868592240054, -16.85052413769862056 ) ) ;
#38155 = ORIENTED_EDGE ( 'NONE', *, *, #18920, .F. ) ;
#38156 = CARTESIAN_POINT ( 'NONE',  ( 59.58307739690713589, -13.63526775528383794, -7.397079453926873605 ) ) ;
#38157 = CARTESIAN_POINT ( 'NONE',  ( 125.0048763211386245, 1.969000387454901801, -10.12399143400218904 ) ) ;
#38158 = EDGE_CURVE ( 'NONE', #41822, #29144, #27858, .T. ) ;
#38159 = CARTESIAN_POINT ( 'NONE',  ( 107.0793640045248196, 0.1403307496149616695, -15.46607636864997204 ) ) ;
#38160 = CARTESIAN_POINT ( 'NONE',  ( 117.9810475888224062, -2.372251574601226043, -17.96033910819752322 ) ) ;
#38161 = CARTESIAN_POINT ( 'NONE',  ( 124.0848681442452772, -5.574606645277164318, -18.38911715685844683 ) ) ;
#38162 = CARTESIAN_POINT ( 'NONE',  ( 118.6391081442452986, -5.574606645277164318, -18.38911715685844683 ) ) ;
#38163 = CARTESIAN_POINT ( 'NONE',  ( 119.9766353496756608, -1.087735405160626723, -17.17288456429612964 ) ) ;
#38164 = VERTEX_POINT ( 'NONE', #13506 ) ;
#38165 = CARTESIAN_POINT ( 'NONE',  ( 126.2184548109119788, -4.863998795839242995, -13.39321520033831447 ) ) ;
#38166 = CARTESIAN_POINT ( 'NONE',  ( 115.9729548109119861, -3.505236298600246325, -18.68346056562440793 ) ) ;
#38167 = DIRECTION ( 'NONE',  ( 0.000000000000000000, 0.6004852223388321697, -0.7996358532186279566 ) ) ;
#38168 = CARTESIAN_POINT ( 'NONE',  ( 124.9924948109119924, -4.089484607189486809, -7.948022111789456723 ) ) ;
#38169 = CARTESIAN_POINT ( 'NONE',  ( 126.2404814775786264, -0.8288870151387760510, -10.36305467784173118 ) ) ;
#38170 = ORIENTED_EDGE ( 'NONE', *, *, #276, .T. ) ;
#38171 = CARTESIAN_POINT ( 'NONE',  ( 115.2355081442453155, -10.30919188438810075, -12.61870101168855918 ) ) ;
#38172 = DIRECTION ( 'NONE',  ( 0.000000000000000000, -0.3818493186865927203, 0.9242245927363029745 ) ) ;
#38173 = CARTESIAN_POINT ( 'NONE',  ( 116.0388171295248014, -10.62599879583958540, -13.39321520033831447 ) ) ;
#38174 = CARTESIAN_POINT ( 'NONE',  ( 113.0231681442453322, 0.9020085738987339008, -11.91225656197089222 ) ) ;
#38175 = EDGE_CURVE ( 'NONE', #44110, #6291, #44169, .T. ) ;
#38176 = CARTESIAN_POINT ( 'NONE',  ( 113.0231681442453322, 0.9020085738987339008, -11.91225656197089222 ) ) ;
#38178 = VECTOR ( 'NONE', #33262, 1000.000000000000000 ) ;
#38177 = CARTESIAN_POINT ( 'NONE',  ( 125.2761281442453054, 0.4262465694468514643, -12.03445270309931736 ) ) ;
#38179 = CARTESIAN_POINT ( 'NONE',  ( 112.5661608795247872, -1.325403438956436419, -16.93181055722138595 ) ) ;
#38180 = CARTESIAN_POINT ( 'NONE',  ( 111.4549108795247747, -1.325403438956436419, -16.93181055722141792 ) ) ;
#38181 = DIRECTION ( 'NONE',  ( -1.000000000000000000, 0.000000000000000000, 0.000000000000000000 ) ) ;
#38182 = CARTESIAN_POINT ( 'NONE',  ( 109.2294422726160974, -7.213534936028837663, -18.14492746615356822 ) ) ;
#38183 = CARTESIAN_POINT ( 'NONE',  ( 118.1285681442453068, -2.084020599724406786, -8.691656652584148546 ) ) ;
#38184 = LINE ( 'NONE', #34746, #40789 ) ;
#38185 = DIRECTION ( 'NONE',  ( 0.000000000000000000, 0.6004852223388321697, -0.7996358532186279566 ) ) ;
#38186 = CARTESIAN_POINT ( 'NONE',  ( 110.1353015045248469, -2.477300249445798297, -7.631215200338321125 ) ) ;
#38187 = LINE ( 'NONE', #44828, #13107 ) ;
#38188 = CARTESIAN_POINT ( 'NONE',  ( 124.4819548109119722, -7.893985811506177619, -18.51759400769804742 ) ) ;
#38189 = CARTESIAN_POINT ( 'NONE',  ( 125.3328548109119964, -9.261995988541379177, -16.69588392320231307 ) ) ;
#38190 = EDGE_CURVE ( 'NONE', #2587, #2194, #30823, .T. ) ;
#38191 = CARTESIAN_POINT ( 'NONE',  ( 118.9227414775786400, -10.63000616557722466, -14.87417383870573495 ) ) ;
#38192 = CARTESIAN_POINT ( 'NONE',  ( 117.8449348109119938, -8.166667518702817929, -8.995218007635861213 ) ) ;
#38193 = ORIENTED_EDGE ( 'NONE', *, *, #19475, .T. ) ;
#38194 = CARTESIAN_POINT ( 'NONE',  ( 115.4624148109119943, -4.153390946401321671, -8.397313243818183892 ) ) ;
#38195 = CARTESIAN_POINT ( 'NONE',  ( 125.5597614775786326, -1.561330072975669392, -17.79121239304076951 ) ) ;
#38196 = CARTESIAN_POINT ( 'NONE',  ( 113.9875214775786532, -0.4660016031367893996, -10.09054647747474043 ) ) ;
#38197 = CARTESIAN_POINT ( 'NONE',  ( 117.3911214775786505, -7.894159318335828068, -9.358103419637847864 ) ) ;
#38198 = ORIENTED_EDGE ( 'NONE', *, *, #16105, .F. ) ;
#38199 = CARTESIAN_POINT ( 'NONE',  ( 120.2841814775786276, -10.15424416112533912, -14.75197769757731336 ) ) ;
#38200 = VECTOR ( 'NONE', #7415, 1000.000000000000000 ) ;
#38201 = CARTESIAN_POINT ( 'NONE',  ( 116.4267681442453153, -3.383040157471821630, -19.15922257007629170 ) ) ;
#38202 = CARTESIAN_POINT ( 'NONE',  ( 115.5526452545247622, 0.8980012041604421569, -11.00651665394454071 ) ) ;
#38203 = ORIENTED_EDGE ( 'NONE', *, *, #22524, .F. ) ;
#38204 = AXIS2_PLACEMENT_3D ( 'NONE', #35964, #31874, #14781 ) ;
#38205 = CARTESIAN_POINT ( 'NONE',  ( 114.6874464091100947, -0.9924539043446216624, -17.29976612834909133 ) ) ;
#38206 = CARTESIAN_POINT ( 'NONE',  ( 112.7515004229301780, 0.1075849324168598464, -14.64321520033831447 ) ) ;
#38207 = CARTESIAN_POINT ( 'NONE',  ( 85.82015659721905365, -27.84333996136784961, -14.15691383771150136 ) ) ;
#38208 = CARTESIAN_POINT ( 'NONE',  ( 114.7249681442453237, 0.2603800115204892296, -16.42320221600525088 ) ) ;
#38209 = FACE_OUTER_BOUND ( 'NONE', #41432, .T. ) ;
#38210 = CARTESIAN_POINT ( 'NONE',  ( 121.5100746589382226, -8.341213398351550623, -17.25835129106723542 ) ) ;
#38211 = DIRECTION ( 'NONE',  ( -0.000000000000000000, -0.9284778069183721172, -0.3713878862591650232 ) ) ;
#38212 = EDGE_CURVE ( 'NONE', #32422, #38815, #7666, .T. ) ;
#38213 = DIRECTION ( 'NONE',  ( -0.1736481776669309696, -0.9848077530122079093, 0.000000000000000000 ) ) ;
#38214 = CARTESIAN_POINT ( 'NONE',  ( 116.2471765045247594, -2.791137627527939813, -8.388885654883777576 ) ) ;
#38215 = CARTESIAN_POINT ( 'NONE',  ( 118.4689281442453392, 0.9020085738987339008, -11.91225656197089222 ) ) ;
#38216 = DIRECTION ( 'NONE',  ( -0.000000000000000000, -0.9284778069183721172, -0.3713878862591650232 ) ) ;
#38217 = CARTESIAN_POINT ( 'NONE',  ( 124.4662673109119879, -9.289237151508565660, -11.05642687123736145 ) ) ;
#38218 = CARTESIAN_POINT ( 'NONE',  ( 122.7801548109119665, -6.222761293078241884, -8.102969835052219238 ) ) ;
#38219 = ORIENTED_EDGE ( 'NONE', *, *, #23071, .F. ) ;
#38220 = CARTESIAN_POINT ( 'NONE',  ( 125.9001214775786224, -4.089484607189486809, -7.948022111789456723 ) ) ;
#38221 = CARTESIAN_POINT ( 'NONE',  ( 118.5823814775786360, -1.834011780172310813, -8.268836392978581529 ) ) ;
#38222 = LINE ( 'NONE', #30946, #36497 ) ;
#38223 = CARTESIAN_POINT ( 'NONE',  ( 114.6682414775786469, -7.894159318335828068, -9.358103419637847864 ) ) ;
#38224 = CARTESIAN_POINT ( 'NONE',  ( 112.1155414775786454, -10.15424416112533912, -14.75197769757731336 ) ) ;
#38225 = CARTESIAN_POINT ( 'NONE',  ( 106.5237390045248418, -9.868328341294098749, -11.32035403202665869 ) ) ;
#38226 = CARTESIAN_POINT ( 'NONE',  ( 114.7192077545248594, -7.250697342233347165, -7.631215200338321125 ) ) ;
#38227 = CARTESIAN_POINT ( 'NONE',  ( 120.8514481442452961, -2.084020599724406786, -8.691656652584148546 ) ) ;
#38228 = CARTESIAN_POINT ( 'NONE',  ( 122.0994348109119443, -10.15424416112533912, -14.75197769757731336 ) ) ;
#38229 = EDGE_CURVE ( 'NONE', #1626, #259, #19326, .T. ) ;
#38230 = CARTESIAN_POINT ( 'NONE',  ( 109.2294439017210550, -0.2843800758933193173, -10.66990552702273476 ) ) ;
#38231 = CARTESIAN_POINT ( 'NONE',  ( 122.6604860609119640, -6.564341423271550902, -7.887810678476487425 ) ) ;
#38232 = CARTESIAN_POINT ( 'NONE',  ( 109.7880358795247986, -8.402594152722688392, -9.854619843455216355 ) ) ;
#38233 = ADVANCED_FACE ( 'NONE', ( #41551 ), #22253, .T. ) ;
#38234 = CARTESIAN_POINT ( 'NONE',  ( 69.69189222814998175, -41.76310523276723785, -24.89321520033831447 ) ) ;
#38235 = CARTESIAN_POINT ( 'NONE',  ( 113.9307948109119906, 0.9020085738987339008, -11.91225656197089222 ) ) ;
#38236 = CARTESIAN_POINT ( 'NONE',  ( 113.3635281442453504, -9.988377603198976828, -10.36322818467138340 ) ) ;
#38237 = DIRECTION ( 'NONE',  ( 0.9908103287288504424, -0.1352586133457950035, 0.000000000000000000 ) ) ;
#38238 = VERTEX_POINT ( 'NONE', #6879 ) ;
#38239 = CARTESIAN_POINT ( 'NONE',  ( 116.9582927111058552, -1.267766418764730840, -16.93314635290706605 ) ) ;
#38240 = VECTOR ( 'NONE', #29009, 1000.000000000000114 ) ;
#38241 = CARTESIAN_POINT ( 'NONE',  ( 120.3409081442453044, -0.4660016031367893996, -10.09054647747474043 ) ) ;
#38242 = CARTESIAN_POINT ( 'NONE',  ( 113.7606148109119886, -1.561330072975668060, -17.79121239304076596 ) ) ;
#38243 = CARTESIAN_POINT ( 'NONE',  ( 116.9373081442452929, -1.833838273342659253, -17.42832698103878286 ) ) ;
#38244 = FILL_AREA_STYLE_COLOUR ( '', #23535 ) ;
#38245 = CARTESIAN_POINT ( 'NONE',  ( 125.6732148109119862, 0.5811942927096110934, -14.16772938898807510 ) ) ;
#38246 = CARTESIAN_POINT ( 'NONE',  ( 118.5823814775786360, -1.834011780172310813, -8.268836392978581529 ) ) ;
#38247 = CARTESIAN_POINT ( 'NONE',  ( 108.9545983795247821, -8.402594152722688392, -16.93181055722141792 ) ) ;
#38248 = CARTESIAN_POINT ( 'NONE',  ( 112.4559014775786778, -0.1624402480850797581, -16.17319339645315424 ) ) ;
#38249 = CARTESIAN_POINT ( 'NONE',  ( 83.84865386347668448, -25.99489077589588604, -15.39321520033831625 ) ) ;
#38250 = ORIENTED_EDGE ( 'NONE', *, *, #30606, .T. ) ;
#38251 = CARTESIAN_POINT ( 'NONE',  ( 119.4332814775786318, -0.4660016031367893996, -10.09054647747474043 ) ) ;
#38252 = CARTESIAN_POINT ( 'NONE',  ( 120.7852516859119731, -9.665098340737509730, -17.37397104707595474 ) ) ;
#38253 = CARTESIAN_POINT ( 'NONE',  ( 114.7816948109119863, 0.5811942927096154232, -14.16772938898807155 ) ) ;
#38254 = CIRCLE ( 'NONE', #10620, 0.5000000000000004441 ) ;
#38255 = ORIENTED_EDGE ( 'NONE', *, *, #5533, .F. ) ;
#38256 = CARTESIAN_POINT ( 'NONE',  ( 114.6497546295247929, -4.863998795839590272, -7.631215200338315796 ) ) ;
#38257 = CARTESIAN_POINT ( 'NONE',  ( 125.3328548109119964, -9.261995988541697145, -16.69588392320189030 ) ) ;
#38258 = CARTESIAN_POINT ( 'NONE',  ( 128.2184548109119930, -4.863998795839242995, -13.39321520033831447 ) ) ;
#38259 = LINE ( 'NONE', #20951, #44436 ) ;
#38260 = DIRECTION ( 'NONE',  ( 0.9908103287288504424, -0.1352586133457950590, 0.000000000000000000 ) ) ;
#38261 = CARTESIAN_POINT ( 'NONE',  ( 120.1140014775786398, -7.894159318335828068, -9.358103419637847864 ) ) ;
#38262 = CARTESIAN_POINT ( 'NONE',  ( 120.0947965460471920, -2.191907684172563986, -18.20049396185734025 ) ) ;
#38263 = CONICAL_SURFACE ( 'NONE', #34648, 2.999999999999999556, 0.9599310885968830309 ) ;
#38264 = CARTESIAN_POINT ( 'NONE',  ( 119.3198281442452924, -9.859900752359374465, -12.68260735090039404 ) ) ;
#38265 = DIRECTION ( 'NONE',  ( -0.000000000000000000, -0.9284778069183721172, -0.3713878862591650232 ) ) ;
#38266 = CARTESIAN_POINT ( 'NONE',  ( 120.8514481442452961, -2.084020599724406786, -8.691656652584148546 ) ) ;
#38267 = CARTESIAN_POINT ( 'NONE',  ( 123.6328298109119714, -2.173413727453600508, -8.297982527556802879 ) ) ;
#38268 = CARTESIAN_POINT ( 'NONE',  ( 116.7104014775786425, -0.4660016031367893996, -10.09054647747474043 ) ) ;
#38269 = CARTESIAN_POINT ( 'NONE',  ( 119.7434548109119703, -2.421111938423274879, -5.775321541204940345 ) ) ;
#38270 = CARTESIAN_POINT ( 'NONE',  ( 116.3133148109120043, -2.084020599724406786, -8.691656652584148546 ) ) ;
#38271 = VERTEX_POINT ( 'NONE', #13945 ) ;
#38272 = CARTESIAN_POINT ( 'NONE',  ( 115.8027748109119841, -0.4660016031367893996, -10.09054647747474043 ) ) ;
#38273 = CARTESIAN_POINT ( 'NONE',  ( 108.9545983795247821, -0.7896495226426338832, -9.318865927141430916 ) ) ;
#38274 = CARTESIAN_POINT ( 'NONE',  ( 84.49707967414211396, -25.99489077589524300, -13.39321520033831625 ) ) ;
#38275 = DIRECTION ( 'NONE',  ( 0.000000000000000000, -0.9242245927363028635, -0.3818493186865930533 ) ) ;
#38276 = EDGE_CURVE ( 'NONE', #38683, #5080, #33, .T. ) ;
#38277 = DIRECTION ( 'NONE',  ( 1.000000000000000000, 0.000000000000000000, -0.000000000000000000 ) ) ;
#38278 = CIRCLE ( 'NONE', #43374, 1.000000000000000888 ) ;
#38279 = CARTESIAN_POINT ( 'NONE',  ( 122.7234281442452755, -5.638512984488999180, -18.83840828888717311 ) ) ;
#38280 = VERTEX_POINT ( 'NONE', #1370 ) ;
#38281 = CARTESIAN_POINT ( 'NONE',  ( 127.0553483106876484, -8.910448477848374793, -9.789625213634170819 ) ) ;
#38282 = CARTESIAN_POINT ( 'NONE',  ( 117.1074881442453233, 0.4262465694468514643, -12.03445270309931736 ) ) ;
#38283 = CARTESIAN_POINT ( 'NONE',  ( 115.8595014775786609, -1.834011780172301043, -8.268836392978595740 ) ) ;
#38284 = CARTESIAN_POINT ( 'NONE',  ( 125.4584548109119737, -2.529232162391097827, -8.971805383624054997 ) ) ;
#38285 = CARTESIAN_POINT ( 'NONE',  ( 123.7445081442452874, -1.561330072975668948, -17.79121239304076951 ) ) ;
#38286 = CARTESIAN_POINT ( 'NONE',  ( 113.7468640045248236, 0.1403307496149616695, -15.46607636864997204 ) ) ;
#38287 = DIRECTION ( 'NONE',  ( 0.000000000000000000, -0.4669533266896274681, -0.8842819633428525838 ) ) ;
#38288 = AXIS2_PLACEMENT_3D ( 'NONE', #39904, #8666, #29414 ) ;
#38289 = ORIENTED_EDGE ( 'NONE', *, *, #28401, .F. ) ;
#38290 = DIRECTION ( 'NONE',  ( 0.000000000000000000, 0.4669533266896293000, 0.8842819633428516957 ) ) ;
#38291 = CARTESIAN_POINT ( 'NONE',  ( 125.3328548109119964, -0.8288870151387760510, -10.36305467784173118 ) ) ;
#38292 = CARTESIAN_POINT ( 'NONE',  ( 122.6667014775786413, -7.893985811506177619, -18.51759400769804742 ) ) ;
#38293 = CARTESIAN_POINT ( 'NONE',  ( 117.9583881442453048, 0.1319031606808879209, -14.10382304977623669 ) ) ;
#38294 = CARTESIAN_POINT ( 'NONE',  ( 80.19189222814998175, -66.20485342690169261, -45.06987807991851724 ) ) ;
#38295 = CARTESIAN_POINT ( 'NONE',  ( 117.7882081442453170, -6.344957434206665248, -7.627207830600338134 ) ) ;
#38296 = DIRECTION ( 'NONE',  ( 0.000000000000000000, 0.9284778069183720062, 0.3713878862591650232 ) ) ;
#38297 = CARTESIAN_POINT ( 'NONE',  ( 122.9503348109119827, -9.859900752359378018, -12.68260735090039759 ) ) ;
#38298 = VERTEX_POINT ( 'NONE', #4336 ) ;
#38299 = AXIS2_PLACEMENT_3D ( 'NONE', #18007, #14588, #28506 ) ;
#38300 = CARTESIAN_POINT ( 'NONE',  ( 116.5987716749792895, -9.866677412677834269, -13.52174868289714027 ) ) ;
#38301 = CARTESIAN_POINT ( 'NONE',  ( 118.4689281442453392, 0.9020085738987339008, -11.91225656197089222 ) ) ;
#38302 = CARTESIAN_POINT ( 'NONE',  ( 123.4041481442452834, 0.1319031606808879209, -14.10382304977623669 ) ) ;
#38303 = ORIENTED_EDGE ( 'NONE', *, *, #23419, .T. ) ;
#38304 = PRODUCT ( 'MAT-055', 'MAT-055', '', ( #8368 ) ) ;
#38305 = LINE ( 'NONE', #7690, #32547 ) ;
#38306 = CARTESIAN_POINT ( 'NONE',  ( 67.30914723170953096, -60.66501133130886814, -38.36331010974746647 ) ) ;
#38307 = CARTESIAN_POINT ( 'NONE',  ( 121.6456214775786293, -10.63000616557722466, -14.87417383870573495 ) ) ;
#38308 = CARTESIAN_POINT ( 'NONE',  ( 109.0240515045248202, -2.477300249445798297, -7.631215200338321125 ) ) ;
#38309 = CARTESIAN_POINT ( 'NONE',  ( 119.8303681442453126, 0.4262465694468514643, -12.03445270309931736 ) ) ;
#38310 = ORIENTED_EDGE ( 'NONE', *, *, #38158, .F. ) ;
#38311 = VERTEX_POINT ( 'NONE', #11426 ) ;
#38312 = CARTESIAN_POINT ( 'NONE',  ( 115.1220548109119761, -8.166667518702817929, -8.995218007635861213 ) ) ;
#38313 = CARTESIAN_POINT ( 'NONE',  ( 125.5030348109119558, -6.222761293078241884, -8.102969835052219238 ) ) ;
#38314 = CARTESIAN_POINT ( 'NONE',  ( 70.19189222814998175, -55.19510675323109439, -35.28085945431567438 ) ) ;
#38315 = CARTESIAN_POINT ( 'NONE',  ( 80.91184012100937650, -3.933054092416038650, -15.89321520033831447 ) ) ;
#38316 = CARTESIAN_POINT ( 'NONE',  ( 123.4608748109119745, -10.63000616557722466, -14.87417383870573495 ) ) ;
#38317 = CONICAL_SURFACE ( 'NONE', #15032, 2.445500000000004448, 0.9599310885968757034 ) ;
#38318 = CARTESIAN_POINT ( 'NONE',  ( 79.72353890764954087, 4.236894767232761261, -12.14321520033831625 ) ) ;
#38319 = CARTESIAN_POINT ( 'NONE',  ( 70.19189222814998175, -100.0979043305785581, -53.24182196210380624 ) ) ;
#38320 = CARTESIAN_POINT ( 'NONE',  ( 122.7234281442452755, -5.638512984488999180, -18.83840828888717311 ) ) ;
#38322 = CARTESIAN_POINT ( 'NONE',  ( 123.4608748109119745, 0.4262465694468514643, -12.03445270309931736 ) ) ;
#38321 = CARTESIAN_POINT ( 'NONE',  ( 120.0005481442453146, -5.638512984488999180, -18.83840828888717311 ) ) ;
#38323 = CARTESIAN_POINT ( 'NONE',  ( 121.6456214775786293, 0.4262465694468514643, -12.03445270309931736 ) ) ;
#38324 = DIRECTION ( 'NONE',  ( -0.8636456077245090457, 0.5040994586965585889, 0.000000000000000000 ) ) ;
#38325 = CARTESIAN_POINT ( 'NONE',  ( 116.4267681442453153, -3.383040157471821630, -19.15922257007629170 ) ) ;
#38326 = ORIENTED_EDGE ( 'NONE', *, *, #4937, .F. ) ;
#38327 = AXIS2_PLACEMENT_3D ( 'NONE', #16409, #27351, #44685 ) ;
#38328 = CARTESIAN_POINT ( 'NONE',  ( 125.2655881442453278, 0.08617673920530924403, -14.09731900820076334 ) ) ;
#38329 = CARTESIAN_POINT ( 'NONE',  ( 115.1359265045248605, -2.791137627527939813, -8.388885654883777576 ) ) ;
#38330 = CARTESIAN_POINT ( 'NONE',  ( 110.6909265045248247, -2.791137627527939813, -8.388885654883777576 ) ) ;
#38331 = CARTESIAN_POINT ( 'NONE',  ( 105.8986608795248401, -8.938348069036489818, -9.318865927141430916 ) ) ;
#38332 = CARTESIAN_POINT ( 'NONE',  ( 124.8223148109119762, 0.9020085738987339008, -11.91225656197089222 ) ) ;
#38333 = CARTESIAN_POINT ( 'NONE',  ( 111.7184548109119788, -9.261995988541697145, -16.69588392320189030 ) ) ;
#38334 = ORIENTED_EDGE ( 'NONE', *, *, #38394, .T. ) ;
#38335 = CARTESIAN_POINT ( 'NONE',  ( 113.3068014775786594, -1.833838273342658809, -17.42832698103878286 ) ) ;
#38336 = CARTESIAN_POINT ( 'NONE',  ( 113.6774108795247997, -8.938348069036489818, -9.318865927141430916 ) ) ;
#38337 = CARTESIAN_POINT ( 'NONE',  ( 61.76986277844709861, -39.32091226840162079, -6.340220811149025693 ) ) ;
#38338 = CARTESIAN_POINT ( 'NONE',  ( 124.4252281442452812, -9.261995988541697145, -16.69588392320189030 ) ) ;
#38339 = FACE_OUTER_BOUND ( 'NONE', #8039, .T. ) ;
#38340 = CARTESIAN_POINT ( 'NONE',  ( -1.145390592550938891, -14.88589425535892019, -18.19321520033831519 ) ) ;
#38341 = CARTESIAN_POINT ( 'NONE',  ( 112.7395348109119766, -5.638512984488999180, -18.83840828888717311 ) ) ;
#38342 = CARTESIAN_POINT ( 'NONE',  ( 113.6079577545248043, -7.250697342233347165, -7.631215200338321125 ) ) ;
#38343 = CARTESIAN_POINT ( 'NONE',  ( 115.2748327545248657, -6.936859964151250502, -8.388885654883777576 ) ) ;
#38344 = VERTEX_POINT ( 'NONE', #38766 ) ;
#38345 = CARTESIAN_POINT ( 'NONE',  ( 116.2659068881580708, -12.01880880694303855, -20.89321520033831447 ) ) ;
#38346 = CARTESIAN_POINT ( 'NONE',  ( 116.9373081442452929, -1.833838273342659253, -17.42832698103878286 ) ) ;
#38347 = CARTESIAN_POINT ( 'NONE',  ( 113.2500748109119968, -6.344957434206662583, -7.627207830600332805 ) ) ;
#38348 = VECTOR ( 'NONE', #37474, 1000.000000000000000 ) ;
#38349 = CARTESIAN_POINT ( 'NONE',  ( 113.6774108795247997, -8.938348069036489818, -9.318865927141430916 ) ) ;
#38350 = CARTESIAN_POINT ( 'NONE',  ( 108.4684265045248424, -2.791137627527939813, -8.388885654883777576 ) ) ;
#38351 = CARTESIAN_POINT ( 'NONE',  ( 122.0427081442452817, -9.859900752359378018, -12.68260735090039759 ) ) ;
#38352 = CARTESIAN_POINT ( 'NONE',  ( 120.1707281442453166, -9.565557343593413364, -10.61323700422348004 ) ) ;
#38353 = CARTESIAN_POINT ( 'NONE',  ( 125.5597614775786326, -1.561330072975669392, -17.79121239304076951 ) ) ;
#38354 = VERTEX_POINT ( 'NONE', #14840 ) ;
#38355 = AXIS2_PLACEMENT_3D ( 'NONE', #22928, #1722, #12455 ) ;
#38356 = CARTESIAN_POINT ( 'NONE',  ( 125.1626748109119802, -0.1624402480850797581, -16.17319339645315424 ) ) ;
#38357 = CARTESIAN_POINT ( 'NONE',  ( 85.45605303719084134, -15.74807682313488222, -13.39321520033831447 ) ) ;
#38358 = CARTESIAN_POINT ( 'NONE',  ( 114.1009748109119784, -5.574606645277164318, -18.38911715685844683 ) ) ;
#38359 = ORIENTED_EDGE ( 'NONE', *, *, #31987, .T. ) ;
#38360 = CARTESIAN_POINT ( 'NONE',  ( 126.6390922358648368, -9.448224192814040023, -15.87040149726915139 ) ) ;
#38361 = CIRCLE ( 'NONE', #8536, 2.999999999999999556 ) ;
#38362 = CARTESIAN_POINT ( 'NONE',  ( 108.7462390045248242, -9.868328341294098749, -11.32035403202665869 ) ) ;
#38363 = VERTEX_POINT ( 'NONE', #7768 ) ;
#38364 = CARTESIAN_POINT ( 'NONE',  ( 119.5467348109119712, -5.574606645277164318, -18.38911715685844683 ) ) ;
#38365 = CARTESIAN_POINT ( 'NONE',  ( 113.2500748109119968, -3.505236298600246325, -18.68346056562440793 ) ) ;
#38366 = DIRECTION ( 'NONE',  ( 0.000000000000000000, 0.7996358532185066093, 0.6004852223389939292 ) ) ;
#38367 = ADVANCED_FACE ( 'NONE', ( #25551 ), #26618, .F. ) ;
#38368 = CARTESIAN_POINT ( 'NONE',  ( 120.7852516859119731, -9.665098340737509730, -17.37397104707595474 ) ) ;
#38369 = EDGE_LOOP ( 'NONE', ( #42012, #36027, #33999, #13497 ) ) ;
#38370 = CARTESIAN_POINT ( 'NONE',  ( 121.4571555643466922, -1.244021962887374544, -16.96476564598603076 ) ) ;
#38371 = CARTESIAN_POINT ( 'NONE',  ( 119.7434548109119845, -2.534040247545263469, -8.964764792708688645 ) ) ;
#38372 = CARTESIAN_POINT ( 'NONE',  ( 106.2459265045248173, -2.791137627527939813, -8.388885654883777576 ) ) ;
#38373 = AXIS2_PLACEMENT_3D ( 'NONE', #8607, #28464, #39621 ) ;
#38374 = CARTESIAN_POINT ( 'NONE',  ( 117.2294421295248128, -10.91793254776207611, -21.88709314391948269 ) ) ;
#38375 = CARTESIAN_POINT ( 'NONE',  ( 122.0994348109119443, -10.15424416112533912, -14.75197769757731336 ) ) ;
#38376 = CARTESIAN_POINT ( 'NONE',  ( 116.7104014775786425, -8.899110576539710493, -16.42337572283490132 ) ) ;
#38377 = CARTESIAN_POINT ( 'NONE',  ( 114.0442481442453300, -7.643976991954099631, -18.09477374809247152 ) ) ;
#38378 = ORIENTED_EDGE ( 'NONE', *, *, #24471, .T. ) ;
#38379 = CARTESIAN_POINT ( 'NONE',  ( 117.6747548109119919, -7.643976991954077427, -18.09477374809248928 ) ) ;
#38380 = CARTESIAN_POINT ( 'NONE',  ( 125.0492214775786266, -3.505236298600246325, -18.68346056562440793 ) ) ;
#38381 = CARTESIAN_POINT ( 'NONE',  ( 86.48169505875749508, -25.99489077589524300, -13.39321520033831625 ) ) ;
#38382 = FACE_OUTER_BOUND ( 'NONE', #6155, .T. ) ;
#38383 = CARTESIAN_POINT ( 'NONE',  ( 113.7606148109119886, -1.561330072975668060, -17.79121239304076596 ) ) ;
#38384 = EDGE_LOOP ( 'NONE', ( #13512, #10176, #1115, #11062, #31360, #32676, #36678 ) ) ;
#38385 = CARTESIAN_POINT ( 'NONE',  ( 115.2922348109119781, -10.63000616557722466, -14.87417383870573495 ) ) ;
#38386 = DIRECTION ( 'NONE',  ( 0.9609149988134843001, -0.1028163501681632064, 0.2570431154366505933 ) ) ;
#38387 = CARTESIAN_POINT ( 'NONE',  ( 109.9963952545248134, 0.8980012041604421569, -11.00651665394454071 ) ) ;
#38388 = CARTESIAN_POINT ( 'NONE',  ( 113.1366214775786432, -1.834011780172310813, -8.268836392978581529 ) ) ;
#38389 = CARTESIAN_POINT ( 'NONE',  ( 113.4769814775786330, -10.63000616557722466, -14.87417383870573495 ) ) ;
#38390 = VECTOR ( 'NONE', #5572, 1000.000000000000114 ) ;
#38391 = CARTESIAN_POINT ( 'NONE',  ( 122.6099748109119929, -0.8288870151387760510, -10.36305467784173118 ) ) ;
#38392 = PLANE ( 'NONE',  #31510 ) ;
#38393 = CARTESIAN_POINT ( 'NONE',  ( 110.6214733795247867, -1.325403438956436419, -9.854619843455211026 ) ) ;
#38394 = EDGE_CURVE ( 'NONE', #41326, #12923, #11323, .T. ) ;
#38395 = CARTESIAN_POINT ( 'NONE',  ( 111.9261565460472099, -2.191907684172563986, -18.20049396185734025 ) ) ;
#38396 = CARTESIAN_POINT ( 'NONE',  ( 109.2294421683802312, -8.290612149491295213, -17.51551637747833468 ) ) ;
#38397 = CARTESIAN_POINT ( 'NONE',  ( 116.1431348109119881, 0.1319031606808879209, -14.10382304977623669 ) ) ;
#38398 = CARTESIAN_POINT ( 'NONE',  ( 105.7597546295248350, -4.863998795839590272, -7.631215200338315796 ) ) ;
#38399 = CARTESIAN_POINT ( 'NONE',  ( 115.5526452545247622, -9.868328341294098749, -15.46607636864997204 ) ) ;
#38400 = CARTESIAN_POINT ( 'NONE',  ( 110.8298327545248299, -2.477300249445798297, -19.15521520033831138 ) ) ;
#38401 = CARTESIAN_POINT ( 'NONE',  ( 67.37136766119182596, -70.31694239570130378, -42.20474206142759499 ) ) ;
#38402 = CARTESIAN_POINT ( 'NONE',  ( 126.1837548109119211, -10.63000616557722466, -14.87417383870573495 ) ) ;
#38403 = CARTESIAN_POINT ( 'NONE',  ( 70.19189222814998175, -100.0979043305785581, -53.24182196210380624 ) ) ;
#38404 =( BOUNDED_CURVE ( )  B_SPLINE_CURVE ( 3, ( #15673, #18645, #39393, #29577 ),
 .UNSPECIFIED., .F., .F. ) 
 B_SPLINE_CURVE_WITH_KNOTS ( ( 4, 4 ),
 ( 0.000000000000000000, 3.141592653589795336 ),
 .UNSPECIFIED. ) 
 CURVE ( )  GEOMETRIC_REPRESENTATION_ITEM ( )  RATIONAL_B_SPLINE_CURVE ( ( 1.000000000000000000, 0.3333333333333335369, 0.3333333333333335369, 1.000000000000000000 ) ) 
 REPRESENTATION_ITEM ( '' )  );
#38405 = ADVANCED_FACE ( 'NONE', ( #8221 ), #10752, .F. ) ;
#38406 = CARTESIAN_POINT ( 'NONE',  ( 119.6601881442453106, -8.166667518702819706, -8.995218007635861213 ) ) ;
#38407 = CARTESIAN_POINT ( 'NONE',  ( 114.7249681442453237, 0.2603800115204892296, -16.42320221600525088 ) ) ;
#38408 = ORIENTED_EDGE ( 'NONE', *, *, #44365, .F. ) ;
#38409 = EDGE_CURVE ( 'NONE', #19235, #12781, #21676, .T. ) ;
#38410 = CARTESIAN_POINT ( 'NONE',  ( 114.6115148109119986, -6.222761293078241884, -8.102969835052219238 ) ) ;
#38411 = CARTESIAN_POINT ( 'NONE',  ( 124.2550481442452792, -9.988377603198980381, -10.36322818467138518 ) ) ;
#38412 = CARTESIAN_POINT ( 'NONE',  ( 116.9373081442452929, -8.166667518702817929, -8.995218007635861213 ) ) ;
#38413 = AXIS2_PLACEMENT_3D ( 'NONE', #24476, #10358, #30648 ) ;
#38414 = CARTESIAN_POINT ( 'NONE',  ( 116.1431348109119881, 0.1319031606808879209, -14.10382304977623669 ) ) ;
#38415 = ORIENTED_EDGE ( 'NONE', *, *, #34847, .F. ) ;
#38416 = CARTESIAN_POINT ( 'NONE',  ( 122.5532481442453019, 0.4262465694468514643, -12.03445270309931736 ) ) ;
#38417 = ADVANCED_FACE ( 'NONE', ( #7990 ), #32378, .T. ) ;
#38418 = CARTESIAN_POINT ( 'NONE',  ( 117.3911214775786505, -1.561330072975668504, -17.79121239304076951 ) ) ;
#38419 = CARTESIAN_POINT ( 'NONE',  ( 137.4696151216520263, 0.06564595942581503973, -14.47274270616910563 ) ) ;
#38420 = CARTESIAN_POINT ( 'NONE',  ( 115.6220983795247861, -0.7896495226426338832, -9.318865927141430916 ) ) ;
#38421 = EDGE_CURVE ( 'NONE', #29406, #13199, #28298, .T. ) ;
#38422 = EDGE_CURVE ( 'NONE', #25709, #17452, #40494, .T. ) ;
#38423 = EDGE_CURVE ( 'NONE', #5495, #22604, #4798, .T. ) ;
#38424 = LINE ( 'NONE', #27294, #1666 ) ;
#38425 = CARTESIAN_POINT ( 'NONE',  ( 124.9357681442453014, -1.834011780172310813, -8.268836392978581529 ) ) ;
#38426 = DIRECTION ( 'NONE',  ( 1.000000000000000000, 0.000000000000000000, -0.000000000000000000 ) ) ;
#38427 = CARTESIAN_POINT ( 'NONE',  ( 114.3278814775786429, -10.30919188438810075, -12.61870101168855918 ) ) ;
#38428 = CARTESIAN_POINT ( 'NONE',  ( 136.7860375664301387, -10.44385780544745401, -13.88278873169130456 ) ) ;
#38429 = FACE_OUTER_BOUND ( 'NONE', #4498, .T. ) ;
#38430 = CARTESIAN_POINT ( 'NONE',  ( 104.9263171295248327, 0.1403307496149613920, -13.39321520033831447 ) ) ;
#38431 = CARTESIAN_POINT ( 'NONE',  ( 91.77400275106518279, -25.99489077589524300, -13.39321520033831625 ) ) ;
#38432 = CARTESIAN_POINT ( 'NONE',  ( 116.5944421295247793, -9.868328341294093420, -13.39321520033831447 ) ) ;
#38433 = CARTESIAN_POINT ( 'NONE',  ( 118.8092881442453290, -9.988377603198976828, -10.36322818467138340 ) ) ;
#38434 = CARTESIAN_POINT ( 'NONE',  ( 123.4939235609119663, -9.645473719204776586, -14.86997237629375590 ) ) ;
#38435 = CARTESIAN_POINT ( 'NONE',  ( 111.7795248144346800, -2.280480477428481922, -18.08254604495228079 ) ) ;
#38436 = CARTESIAN_POINT ( 'NONE',  ( 119.1389604811917025, -3.807985514183269693, -19.09877912889401230 ) ) ;
#38437 = CARTESIAN_POINT ( 'NONE',  ( 124.0281414775786146, -7.643976991954077427, -18.09477374809248928 ) ) ;
#38438 = CARTESIAN_POINT ( 'NONE',  ( 117.9016614775786280, -0.1624402480850797581, -16.17319339645315424 ) ) ;
#38439 = ORIENTED_EDGE ( 'NONE', *, *, #9005, .T. ) ;
#38440 = CARTESIAN_POINT ( 'NONE',  ( 122.1179700565388941, -8.485573535863895955, -17.53172993199661178 ) ) ;
#38441 = CARTESIAN_POINT ( 'NONE',  ( 123.1205148109119563, -1.834011780172310813, -8.268836392978581529 ) ) ;
#38442 = CARTESIAN_POINT ( 'NONE',  ( 114.8581140045248361, 0.1403307496149616695, -15.46607636864997204 ) ) ;
#38443 = CARTESIAN_POINT ( 'NONE',  ( 114.2711548109119803, -0.1624402480850797581, -16.17319339645315424 ) ) ;
#38444 = CARTESIAN_POINT ( 'NONE',  ( 112.7395348109119766, -4.153390946401321671, -8.397313243818183892 ) ) ;
#38445 = CARTESIAN_POINT ( 'NONE',  ( 86.09796674931440918, -26.99705449037680438, -8.518632518551283894 ) ) ;
#38446 = CARTESIAN_POINT ( 'NONE',  ( 112.0799890045248475, 0.8980012041604421569, -15.77991374673208469 ) ) ;
#38447 = CARTESIAN_POINT ( 'NONE',  ( 120.6812681442452941, 0.1319031606808879209, -14.10382304977623669 ) ) ;
#38448 = CARTESIAN_POINT ( 'NONE',  ( 120.8514481442452961, -2.084020599724406786, -8.691656652584148546 ) ) ;
#38449 = CARTESIAN_POINT ( 'NONE',  ( 116.5965958012052539, -9.868328341294104078, -13.45749254416749174 ) ) ;
#38450 = LINE ( 'NONE', #3791, #5159 ) ;
#38451 = CARTESIAN_POINT ( 'NONE',  ( 120.5768923109119868, -9.959231468620755479, -10.70263013195267199 ) ) ;
#38452 = CARTESIAN_POINT ( 'NONE',  ( 110.8298327545248299, -6.936859964151250502, -8.388885654883777576 ) ) ;
#38453 = CARTESIAN_POINT ( 'NONE',  ( 70.19189222814998175, -52.61716011954800365, -34.24968978710501943 ) ) ;
#38454 = CARTESIAN_POINT ( 'NONE',  ( 118.2420214775786320, -3.383040157471821630, -19.15922257007629170 ) ) ;
#38455 = CARTESIAN_POINT ( 'NONE',  ( 113.5904348109119866, -7.893985811506177619, -18.51759400769804742 ) ) ;
#38456 = CARTESIAN_POINT ( 'NONE',  ( 110.6214733795247867, -8.938348069036489818, -17.46756447353520159 ) ) ;
#38457 = DIRECTION ( 'NONE',  ( 0.000000000000000000, 0.000000000000000000, 1.000000000000000000 ) ) ;
#38458 = VERTEX_POINT ( 'NONE', #17809 ) ;
#38459 = CARTESIAN_POINT ( 'NONE',  ( 113.2099653070359011, -1.196538596002804766, -17.02799684832027438 ) ) ;
#38460 = CARTESIAN_POINT ( 'NONE',  ( 121.1350814775786233, 0.5811942927096110934, -14.16772938898807510 ) ) ;
#38461 = CARTESIAN_POINT ( 'NONE',  ( 112.2289948109119848, -1.834011780172310813, -8.268836392978581529 ) ) ;
#38462 = CARTESIAN_POINT ( 'NONE',  ( 123.5176014775786228, -0.8288870151387760510, -10.36305467784173118 ) ) ;
#38463 = CARTESIAN_POINT ( 'NONE',  ( 124.8223148109119762, 0.9020085738987339008, -11.91225656197089222 ) ) ;
#38464 = CARTESIAN_POINT ( 'NONE',  ( 118.1285681442453068, -7.893985811506177619, -18.51759400769804742 ) ) ;
#38465 = CARTESIAN_POINT ( 'NONE',  ( 107.5655358795247736, -8.402594152722688392, -9.854619843455216355 ) ) ;
#38466 = CARTESIAN_POINT ( 'NONE',  ( 114.9518748109119883, -7.643976991954077427, -18.09477374809248928 ) ) ;
#38467 = DIRECTION ( 'NONE',  ( 0.000000000000000000, -0.9242245927363029745, -0.3818493186865927758 ) ) ;
#38468 = ORIENTED_EDGE ( 'NONE', *, *, #13318, .T. ) ;
#38469 = CARTESIAN_POINT ( 'NONE',  ( 120.0005481442453146, -5.638512984488999180, -18.83840828888717311 ) ) ;
#38470 = CARTESIAN_POINT ( 'NONE',  ( 91.38554522942851577, -25.99489077589524300, -13.39321520033831625 ) ) ;
#38471 = CARTESIAN_POINT ( 'NONE',  ( 117.4478481442453131, 0.2603800115204892296, -16.42320221600525088 ) ) ;
#38472 = ORIENTED_EDGE ( 'NONE', *, *, #7095, .T. ) ;
#38473 = CARTESIAN_POINT ( 'NONE',  ( 107.2182702545248105, 0.1403307496149616695, -11.32035403202665336 ) ) ;
#38474 = CARTESIAN_POINT ( 'NONE',  ( 123.9714148109119805, -0.4660016031367893996, -10.09054647747474043 ) ) ;
#38475 = DIRECTION ( 'NONE',  ( 1.000000000000000000, 0.000000000000000000, 0.000000000000000000 ) ) ;
#38476 = CARTESIAN_POINT ( 'NONE',  ( 115.8595014775786609, -7.643976991954077427, -18.09477374809248928 ) ) ;
#38477 =( BOUNDED_SURFACE ( )  B_SPLINE_SURFACE ( 1, 2, ( 
 ( #19029, #1692, #26097, #40002, #22899, #2135, #22673, #36793, #5562, #16065, #40467, #36569, #5346, #23136, #10359, #3276, #10579, #23826, #6014, #19938, #9677, #33825, #30649, #2596, #34715, #6711, #27005, #6928, #27237, #3499, #17199, #44567, #20836, #30874, #16526, #45017, #41152, #44344, #30425, #37243, #37713, #13103, #40926, #27686, #17416, #31307, #2825, #24265, #3054, #9913, #80, #13993, #27462, #23595, #37480, #16753, #31091, #41821, #10138, #13333, #6254, #20174, #27909, #38154, #34058 ),
 ( #6483, #20398, #13552, #34282, #16980, #44793, #41383, #24043, #37936, #20620, #34497, #13775, #41600, #39280, #8045, #38368, #14663, #21950, #38584, #35842, #38819, #14439, #4614, #7589, #14215, #741, #7824, #7141, #975, #18084, #42486, #31977, #1201, #29022, #21277, #31758, #31532, #4166, #28579, #21731, #28347, #24924, #42711, #21052, #11024, #34929, #21503, #42259, #15115, #3716, #14891, #17636, #28131, #11248, #25157, #39053, #35619, #35391, #303, #528, #4392, #35160, #18309, #32203, #42039 ) ),
 .UNSPECIFIED., .F., .F., .F. ) 
 B_SPLINE_SURFACE_WITH_KNOTS ( ( 2, 2 ),
 ( 3, 2, 2, 2, 2, 2, 2, 2, 2, 2, 2, 2, 2, 2, 2, 2, 2, 2, 2, 2, 2, 2, 2, 2, 2, 2, 2, 2, 2, 2, 2, 2, 3 ),
 ( 0.000000000000000000, 1.000000000000000000 ),
 ( 0.000000000000000000, 0.03125000000000000000, 0.06250000000000000000, 0.09375000000000000000, 0.1250000000000000000, 0.1562500000000000000, 0.1875000000000000000, 0.2187500000000000000, 0.2500000000000000000, 0.2812500000000000000, 0.3125000000000000000, 0.3437500000000000000, 0.3750000000000000000, 0.4062500000000000000, 0.4375000000000000000, 0.4687500000000000000, 0.5000000000000000000, 0.5312500000000000000, 0.5625000000000000000, 0.5937500000000000000, 0.6250000000000000000, 0.6562500000000000000, 0.6875000000000000000, 0.7187500000000000000, 0.7500000000000000000, 0.7812500000000000000, 0.8125000000000000000, 0.8437500000000000000, 0.8750000000000000000, 0.9062500000000000000, 0.9375000000000000000, 0.9687500000000000000, 1.000000000000000000 ),
 .UNSPECIFIED. ) 
 GEOMETRIC_REPRESENTATION_ITEM ( )  RATIONAL_B_SPLINE_SURFACE ( (
 ( 1.000000000000000000, 0.9238795325112869605, 1.000000000000000000, 0.9238795325112869605, 1.000000000000000000, 0.9238795325112869605, 1.000000000000000000, 0.9238795325112869605, 1.000000000000000000, 0.9238795325112869605, 1.000000000000000000, 0.9238795325112869605, 1.000000000000000000, 0.9238795325112869605, 1.000000000000000000, 0.9238795325112869605, 1.000000000000000000, 0.9238795325112869605, 1.000000000000000000, 0.9238795325112869605, 1.000000000000000000, 0.9238795325112869605, 1.000000000000000000, 0.9238795325112869605, 1.000000000000000000, 0.9238795325112869605, 1.000000000000000000, 0.9238795325112869605, 1.000000000000000000, 0.9238795325112869605, 1.000000000000000000, 0.9238795325112869605, 1.000000000000000000, 0.9238795325112869605, 1.000000000000000000, 0.9238795325112869605, 1.000000000000000000, 0.9238795325112869605, 1.000000000000000000, 0.9238795325112869605, 1.000000000000000000, 0.9238795325112869605, 1.000000000000000000, 0.9238795325112869605, 1.000000000000000000, 0.9238795325112869605, 1.000000000000000000, 0.9238795325112869605, 1.000000000000000000, 0.9238795325112869605, 1.000000000000000000, 0.9238795325112869605, 1.000000000000000000, 0.9238795325112869605, 1.000000000000000000, 0.9238795325112869605, 1.000000000000000000, 0.9238795325112869605, 1.000000000000000000, 0.9238795325112869605, 1.000000000000000000, 0.9238795325112869605, 1.000000000000000000, 0.9238795325112869605, 1.000000000000000000),
 ( 1.000000000000000000, 0.9238795325112869605, 1.000000000000000000, 0.9238795325112869605, 1.000000000000000000, 0.9238795325112869605, 1.000000000000000000, 0.9238795325112869605, 1.000000000000000000, 0.9238795325112869605, 1.000000000000000000, 0.9238795325112869605, 1.000000000000000000, 0.9238795325112869605, 1.000000000000000000, 0.9238795325112869605, 1.000000000000000000, 0.9238795325112869605, 1.000000000000000000, 0.9238795325112869605, 1.000000000000000000, 0.9238795325112869605, 1.000000000000000000, 0.9238795325112869605, 1.000000000000000000, 0.9238795325112869605, 1.000000000000000000, 0.9238795325112869605, 1.000000000000000000, 0.9238795325112869605, 1.000000000000000000, 0.9238795325112869605, 1.000000000000000000, 0.9238795325112869605, 1.000000000000000000, 0.9238795325112869605, 1.000000000000000000, 0.9238795325112869605, 1.000000000000000000, 0.9238795325112869605, 1.000000000000000000, 0.9238795325112869605, 1.000000000000000000, 0.9238795325112869605, 1.000000000000000000, 0.9238795325112869605, 1.000000000000000000, 0.9238795325112869605, 1.000000000000000000, 0.9238795325112869605, 1.000000000000000000, 0.9238795325112869605, 1.000000000000000000, 0.9238795325112869605, 1.000000000000000000, 0.9238795325112869605, 1.000000000000000000, 0.9238795325112869605, 1.000000000000000000, 0.9238795325112869605, 1.000000000000000000, 0.9238795325112869605, 1.000000000000000000, 0.9238795325112869605, 1.000000000000000000) ) ) 
 REPRESENTATION_ITEM ( '' )  SURFACE ( )  );
#38478 = DIRECTION ( 'NONE',  ( 0.000000000000000000, 0.000000000000000000, -1.000000000000000000 ) ) ;
#38479 = ADVANCED_FACE ( 'NONE', ( #21453, #15062 ), #921, .F. ) ;
#38480 = CARTESIAN_POINT ( 'NONE',  ( 121.0783548109119749, -9.565557343593413364, -10.61323700422348004 ) ) ;
#38481 = DIRECTION ( 'NONE',  ( 0.000000000000000000, -0.3818493186865927203, 0.9242245927363029745 ) ) ;
#38482 = CARTESIAN_POINT ( 'NONE',  ( 120.7379948109119709, 0.4262465694468514643, -12.03445270309931736 ) ) ;
#38483 = CARTESIAN_POINT ( 'NONE',  ( 125.0660727672602803, -10.95232013398726423, -8.993724727021167098 ) ) ;
#38484 = CARTESIAN_POINT ( 'NONE',  ( 121.1350814775786233, -9.859900752359378018, -12.68260735090039759 ) ) ;
#38485 = CARTESIAN_POINT ( 'NONE',  ( 123.4244704359119709, 1.345710702986147034, -13.97328579221134426 ) ) ;
#38486 = CARTESIAN_POINT ( 'NONE',  ( 114.1577014775786552, -6.344957434206662583, -7.627207830600332805 ) ) ;
#38487 = DIRECTION ( 'NONE',  ( 1.000000000000000000, 0.000000000000000000, -0.000000000000000000 ) ) ;
#38488 = CARTESIAN_POINT ( 'NONE',  ( 119.0361948109119652, -2.084020599724406786, -8.691656652584148546 ) ) ;
#38489 = ORIENTED_EDGE ( 'NONE', *, *, #10952, .T. ) ;
#38490 = CARTESIAN_POINT ( 'NONE',  ( 116.2565881442452991, -9.261995988541697145, -16.69588392320189030 ) ) ;
#38491 = CARTESIAN_POINT ( 'NONE',  ( 106.5237390045248418, 0.8980012041604421569, -15.77991374673208469 ) ) ;
#38492 = CARTESIAN_POINT ( 'NONE',  ( 115.6893214775786447, -9.859900752359374465, -12.68260735090037983 ) ) ;
#38493 = CARTESIAN_POINT ( 'NONE',  ( 114.2330358795247776, -8.402594152722736354, -9.854619843455244776 ) ) ;
#38494 = CARTESIAN_POINT ( 'NONE',  ( 123.3243636130535350, -8.422568683347405383, -17.41241596312870854 ) ) ;
#38495 = CARTESIAN_POINT ( 'NONE',  ( 121.8158014775786171, -5.638512984488999180, -18.83840828888717311 ) ) ;
#38496 = ORIENTED_EDGE ( 'NONE', *, *, #22278, .T. ) ;
#38497 = CARTESIAN_POINT ( 'NONE',  ( 126.3671785243040659, -8.266574344583974110, -9.628621930846563259 ) ) ;
#38498 = CARTESIAN_POINT ( 'NONE',  ( 116.6536748109119941, -10.15424416112533912, -14.75197769757731336 ) ) ;
#38499 = CARTESIAN_POINT ( 'NONE',  ( 125.1063270177812115, -8.332880733164756748, -17.24257150086102897 ) ) ;
#38500 = CARTESIAN_POINT ( 'NONE',  ( 61.15357748477988764, -14.46166092335914755, -19.21272425282928964 ) ) ;
#38501 = CARTESIAN_POINT ( 'NONE',  ( 125.3895814775786448, -7.893985811506177619, -18.51759400769804742 ) ) ;
#38502 = CARTESIAN_POINT ( 'NONE',  ( 111.1076452545248259, -9.868328341294098749, -15.46607636864997204 ) ) ;
#38503 = CARTESIAN_POINT ( 'NONE',  ( 124.6050267045123690, -8.310145695945278632, -17.19951755478114563 ) ) ;
#38504 = ORIENTED_EDGE ( 'NONE', *, *, #16469, .F. ) ;
#38505 = CARTESIAN_POINT ( 'NONE',  ( 114.7249681442453237, 0.2603800115204892296, -16.42320221600525088 ) ) ;
#38506 = CARTESIAN_POINT ( 'NONE',  ( 112.5126281442453120, -10.30919188438810075, -12.61870101168855918 ) ) ;
#38507 = CARTESIAN_POINT ( 'NONE',  ( 124.8223148109119762, 0.9020085738987339008, -11.91225656197089222 ) ) ;
#38508 = CARTESIAN_POINT ( 'NONE',  ( 116.7104014775786425, -8.899110576539710493, -16.42337572283490132 ) ) ;
#38509 = CARTESIAN_POINT ( 'NONE',  ( 125.4584548109119737, -4.863998795839242995, -13.39321520033831447 ) ) ;
#38510 = CARTESIAN_POINT ( 'NONE',  ( 120.2841814775786276, 0.9020085738987339008, -11.91225656197089222 ) ) ;
#38511 = DIRECTION ( 'NONE',  ( 0.1352586133457905626, 0.9908103287288509975, 0.000000000000000000 ) ) ;
#38512 = DIRECTION ( 'NONE',  ( -2.439015257082815255E-15, 1.000000000000000000, 0.000000000000000000 ) ) ;
#38513 = DIRECTION ( 'NONE',  ( 0.000000000000000000, 0.000000000000000000, 1.000000000000000000 ) ) ;
#38514 = CARTESIAN_POINT ( 'NONE',  ( 121.4187148109119789, -3.505236298600246325, -18.68346056562440793 ) ) ;
#38515 = ORIENTED_EDGE ( 'NONE', *, *, #798, .F. ) ;
#38516 = FACE_OUTER_BOUND ( 'NONE', #21768, .T. ) ;
#38517 = CARTESIAN_POINT ( 'NONE',  ( 115.7460481442453357, 0.9020085738987339008, -11.91225656197089222 ) ) ;
#38518 = CARTESIAN_POINT ( 'NONE',  ( 124.9357681442453014, -7.643976991954077427, -18.09477374809248928 ) ) ;
#38519 = ORIENTED_EDGE ( 'NONE', *, *, #17306, .T. ) ;
#38520 = CARTESIAN_POINT ( 'NONE',  ( 112.3991748109119868, -8.166667518702817929, -8.995218007635859436 ) ) ;
#38521 = CARTESIAN_POINT ( 'NONE',  ( 120.5678148109119832, -8.166667518702819706, -8.995218007635861213 ) ) ;
#38522 = CARTESIAN_POINT ( 'NONE',  ( 105.8986608795248401, -8.938348069036489818, -9.318865927141430916 ) ) ;
#38523 = CARTESIAN_POINT ( 'NONE',  ( 121.6456214775786293, 0.4262465694468514643, -12.03445270309931736 ) ) ;
#38524 = ORIENTED_EDGE ( 'NONE', *, *, #40070, .T. ) ;
#38525 = VERTEX_POINT ( 'NONE', #4564 ) ;
#38526 = CARTESIAN_POINT ( 'NONE',  ( 116.0296814775786345, -8.166667518702817929, -8.995218007635861213 ) ) ;
#38527 = ADVANCED_FACE ( 'NONE', ( #18488 ), #43381, .T. ) ;
#38528 = AXIS2_PLACEMENT_3D ( 'NONE', #41906, #21146, #35251 ) ;
#38529 = CARTESIAN_POINT ( 'NONE',  ( 125.2194014775786286, 0.1319031606808879209, -14.10382304977623669 ) ) ;
#38530 = VECTOR ( 'NONE', #37953, 1000.000000000000114 ) ;
#38531 = CARTESIAN_POINT ( 'NONE',  ( 87.44708369096657918, -21.99489077589588604, -4.893215200338314474 ) ) ;
#38532 = CARTESIAN_POINT ( 'NONE',  ( 59.39246203831174853, -12.83800168394059682, -9.393215200338312698 ) ) ;
#38533 = CARTESIAN_POINT ( 'NONE',  ( 124.6521348109119884, -1.561330072975668948, -17.79121239304076951 ) ) ;
#38534 = LINE ( 'NONE', #7988, #26263 ) ;
#38535 = DIRECTION ( 'NONE',  ( -0.9908103287288504424, 0.1352586133457954476, 0.000000000000000000 ) ) ;
#38536 = CARTESIAN_POINT ( 'NONE',  ( 122.8368814775786291, -1.561330072975668948, -17.79121239304076951 ) ) ;
#38538 = CARTESIAN_POINT ( 'NONE',  ( 121.7023481442452919, -0.8288870151387760510, -10.36305467784173118 ) ) ;
#38537 = CARTESIAN_POINT ( 'NONE',  ( 120.8514481442452961, -7.893985811506177619, -18.51759400769804742 ) ) ;
#38539 = CARTESIAN_POINT ( 'NONE',  ( 120.1140014775786398, -7.894159318335828068, -9.358103419637847864 ) ) ;
#38540 = CARTESIAN_POINT ( 'NONE',  ( 67.30914723170953096, -58.80805571747214344, -37.62053433722914519 ) ) ;
#38541 = CARTESIAN_POINT ( 'NONE',  ( 114.6682414775786469, -1.561330072975668060, -17.79121239304076596 ) ) ;
#38542 = ORIENTED_EDGE ( 'NONE', *, *, #98, .T. ) ;
#38543 = CARTESIAN_POINT ( 'NONE',  ( 124.9924948109119924, -5.574606645276184658, -18.38911715685858539 ) ) ;
#38544 = CARTESIAN_POINT ( 'NONE',  ( 112.8439733795247832, -1.325403438956436419, -9.854619843455211026 ) ) ;
#38545 = CARTESIAN_POINT ( 'NONE',  ( 107.5655358795247736, -8.402594152722688392, -9.854619843455216355 ) ) ;
#38546 = CARTESIAN_POINT ( 'NONE',  ( 112.0799890045248475, -9.868328341294098749, -11.32035403202665869 ) ) ;
#38547 = ADVANCED_FACE ( 'NONE', ( #28976 ), #35336, .F. ) ;
#38548 = CARTESIAN_POINT ( 'NONE',  ( 124.9924948109119924, -4.089484607189486809, -7.948022111789456723 ) ) ;
#38549 = CARTESIAN_POINT ( 'NONE',  ( 112.3424481442453384, -6.344957434206662583, -7.627207830600332805 ) ) ;
#38550 = VERTEX_POINT ( 'NONE', #31703 ) ;
#38551 = CARTESIAN_POINT ( 'NONE',  ( 111.4915481442453142, -1.833838273342658365, -17.42832698103878286 ) ) ;
#38552 = CARTESIAN_POINT ( 'NONE',  ( 113.1217858795247935, -0.7896495226426338832, -17.46756447353520159 ) ) ;
#38553 = CARTESIAN_POINT ( 'NONE',  ( 78.69189222814998175, -46.76310523276723785, -6.893215200338315363 ) ) ;
#38554 = CARTESIAN_POINT ( 'NONE',  ( 124.9924948109119924, -4.089484607189486809, -7.948022111789456723 ) ) ;
#38555 = CARTESIAN_POINT ( 'NONE',  ( 125.2761281442453054, -10.63000616557722466, -14.87417383870573495 ) ) ;
#38556 = PLANE ( 'NONE',  #11925 ) ;
#38557 = CARTESIAN_POINT ( 'NONE',  ( 115.9729548109119861, -6.344957434206662583, -7.627207830600332805 ) ) ;
#38558 = CARTESIAN_POINT ( 'NONE',  ( 112.6356140045247827, -10.62599879583958717, -11.00651665394454604 ) ) ;
#38559 = CARTESIAN_POINT ( 'NONE',  ( 114.5108483795247878, -8.402594152722688392, -16.93181055722141792 ) ) ;
#38560 = ORIENTED_EDGE ( 'NONE', *, *, #21494, .F. ) ;
#38561 = CARTESIAN_POINT ( 'NONE',  ( 126.2597653975816883, -7.679457989152358444, -9.236116388709978864 ) ) ;
#38562 = CARTESIAN_POINT ( 'NONE',  ( 116.2565881442453133, -0.8288870151387760510, -10.36305467784173118 ) ) ;
#38563 = CARTESIAN_POINT ( 'NONE',  ( 114.2144281442453178, -8.166667518702817929, -8.995218007635859436 ) ) ;
#38564 = CIRCLE ( 'NONE', #18917, 5.132259260909280307 ) ;
#38565 = CARTESIAN_POINT ( 'NONE',  ( 115.5526452545247622, 0.8980012041604421569, -11.00651665394454071 ) ) ;
#38566 = CARTESIAN_POINT ( 'NONE',  ( 104.9957702545248566, 0.1403307496149616695, -11.32035403202665336 ) ) ;
#38567 = CARTESIAN_POINT ( 'NONE',  ( 122.6099748109119929, -0.8288870151387760510, -10.36305467784173118 ) ) ;
#38568 = CARTESIAN_POINT ( 'NONE',  ( 119.9438214775786378, -2.084020599724406786, -8.691656652584148546 ) ) ;
#38569 = CARTESIAN_POINT ( 'NONE',  ( 125.5030348109119558, -3.383040157471821630, -19.15922257007629170 ) ) ;
#38570 = VERTEX_POINT ( 'NONE', #7310 ) ;
#38571 = CARTESIAN_POINT ( 'NONE',  ( 125.7299414775786346, -10.15424416112533912, -14.75197769757731336 ) ) ;
#38572 = CIRCLE ( 'NONE', #21104, 8.000000000000001776 ) ;
#38573 = DIRECTION ( 'NONE',  ( 1.000000000000000000, 0.000000000000000000, -0.000000000000000000 ) ) ;
#38574 = CARTESIAN_POINT ( 'NONE',  ( 115.0086014775786509, -5.574606645277164318, -18.38911715685844683 ) ) ;
#38575 = VERTEX_POINT ( 'NONE', #38999 ) ;
#38576 = VECTOR ( 'NONE', #26837, 1000.000000000000000 ) ;
#38577 = CARTESIAN_POINT ( 'NONE',  ( 126.3230600034150370, -9.125685433939677793, -16.10726513031420737 ) ) ;
#38578 = CARTESIAN_POINT ( 'NONE',  ( 111.8886348109120092, -3.383040157471821630, -19.15922257007629170 ) ) ;
#38579 = CARTESIAN_POINT ( 'NONE',  ( 109.9963952545248134, -9.868328341294098749, -15.46607636864997204 ) ) ;
#38580 = ORIENTED_EDGE ( 'NONE', *, *, #17301, .F. ) ;
#38581 = CARTESIAN_POINT ( 'NONE',  ( 119.7736414775786358, 0.1319031606808879209, -14.10382304977623669 ) ) ;
#38582 = CARTESIAN_POINT ( 'NONE',  ( 112.1722681442453222, -8.899110576539710493, -16.42337572283490132 ) ) ;
#38583 = CARTESIAN_POINT ( 'NONE',  ( 124.5767528389142029, -9.826152869829959613, -14.03118282328476596 ) ) ;
#38584 = CARTESIAN_POINT ( 'NONE',  ( 120.9936110609119737, -3.163656168406935087, -18.89861972220014508 ) ) ;
#38585 = EDGE_LOOP ( 'NONE', ( #10786, #29664 ) ) ;
#38586 = CARTESIAN_POINT ( 'NONE',  ( 121.3393286996681866, -1.172797794773259072, -17.05961127468926719 ) ) ;
#38587 = CARTESIAN_POINT ( 'NONE',  ( 124.3692356341917105, -2.419758938359494849, -5.831664186524730731 ) ) ;
#38588 = CARTESIAN_POINT ( 'NONE',  ( 106.1070202545248407, 0.1403307496149616695, -11.32035403202665336 ) ) ;
#38589 = VECTOR ( 'NONE', #7722, 1000.000000000000000 ) ;
#38590 = B_SPLINE_CURVE_WITH_KNOTS ( 'NONE', 3,
 ( #44474, #23268, #43797, #41291, #9588, #34188, #40833, #9821, #37150, #40371, #16890, #30331, #20528, #19614, #33498, #15977, #34408, #2277 ),
 .UNSPECIFIED., .F., .F.,
 ( 4, 2, 2, 1, 1, 1, 1, 2, 2, 2, 4 ),
 ( 0.000000000000000000, 0.2500000000001928457, 0.3750000000002891021, 0.4375000000003371747, 0.4687500000003585465, 0.4843750000003703149, 0.4921875000003760325, 0.4960937500003751999, 0.5000000000003742562, 0.7500000000001871836, 1.000000000000000000 ),
 .UNSPECIFIED. ) ;
#38591 = CARTESIAN_POINT ( 'NONE',  ( 112.6828081442453282, -7.893985811506177619, -18.51759400769804742 ) ) ;
#38592 = CARTESIAN_POINT ( 'NONE',  ( 113.0231681442453322, 0.9020085738987339008, -11.91225656197089222 ) ) ;
#38593 = CARTESIAN_POINT ( 'NONE',  ( 117.7314814775786260, -5.574606645277164318, -18.38911715685844683 ) ) ;
#38594 = CARTESIAN_POINT ( 'NONE',  ( 114.1460714802850305, -3.929494816604741203, -18.62311481910882804 ) ) ;
#38595 = VERTEX_POINT ( 'NONE', #35108 ) ;
#38596 = CARTESIAN_POINT ( 'NONE',  ( 116.0864081442453113, -0.1624402480850797581, -16.17319339645315424 ) ) ;
#38597 = CARTESIAN_POINT ( 'NONE',  ( 116.2471765045247594, -7.250697342233347165, -19.15521520033831138 ) ) ;
#38598 = CARTESIAN_POINT ( 'NONE',  ( 84.82510614249602554, -29.13926788429013470, -9.862835514873660614 ) ) ;
#38599 = DIRECTION ( 'NONE',  ( 0.000000000000000000, -0.3818493186865927203, 0.9242245927363029745 ) ) ;
#38600 = CARTESIAN_POINT ( 'NONE',  ( 114.8951481442453115, -0.4660016031367893996, -10.09054647747474043 ) ) ;
#38601 = VERTEX_POINT ( 'NONE', #473 ) ;
#38602 = VECTOR ( 'NONE', #13944, 1000.000000000000227 ) ;
#38603 = CARTESIAN_POINT ( 'NONE',  ( 116.9940348109119839, -9.988377603198976828, -10.36322818467138340 ) ) ;
#38604 = CARTESIAN_POINT ( 'NONE',  ( 109.6527889883689824, 0.3193521225029610777, -12.14321520033828072 ) ) ;
#38605 = CARTESIAN_POINT ( 'NONE',  ( 109.6491296295247793, -4.863998795839590272, -19.15521520033831493 ) ) ;
#38606 = CARTESIAN_POINT ( 'NONE',  ( 112.9097148109120070, 0.2603800115204892296, -16.42320221600525088 ) ) ;
#38607 = CARTESIAN_POINT ( 'NONE',  ( 113.3068014775786594, -8.166667518702817929, -8.995218007635859436 ) ) ;
#38608 = CARTESIAN_POINT ( 'NONE',  ( 124.5386814775786206, -4.153390946401325223, -8.397313243818185668 ) ) ;
#38609 = CARTESIAN_POINT ( 'NONE',  ( 61.55121550909755257, -14.46605081255149905, -17.91752732931888303 ) ) ;
#38610 = CARTESIAN_POINT ( 'NONE',  ( 107.9128015045248219, -6.936859964151250502, -18.39754474579286025 ) ) ;
#38611 = VERTEX_POINT ( 'NONE', #14386 ) ;
#38612 = CARTESIAN_POINT ( 'NONE',  ( 121.9568993241987300, -6.333924026435813204, -18.89660969823682279 ) ) ;
#38613 = CARTESIAN_POINT ( 'NONE',  ( 109.2296097124207250, -8.834719573337491028, -17.03747813294903324 ) ) ;
#38614 = CARTESIAN_POINT ( 'NONE',  ( 117.5045748109119756, -9.859900752359374465, -12.68260735090039404 ) ) ;
#38615 = CARTESIAN_POINT ( 'NONE',  ( 111.2184548109119788, -8.862178061932382889, -16.39564131203247399 ) ) ;
#38616 = CARTESIAN_POINT ( 'NONE',  ( 116.7333483795247844, -8.402594152722688392, -16.93181055722141792 ) ) ;
#38617 = CARTESIAN_POINT ( 'NONE',  ( 108.8851452545248151, 0.8980012041604421569, -11.00651665394454071 ) ) ;
#38618 = CARTESIAN_POINT ( 'NONE',  ( 70.36267391504958368, -5.685877709920885259, -21.89321520033831447 ) ) ;
#38619 = CARTESIAN_POINT ( 'NONE',  ( 125.6732148109119862, 0.5811942927096110934, -14.16772938898807510 ) ) ;
#38620 = LINE ( 'NONE', #21765, #40091 ) ;
#38621 = CARTESIAN_POINT ( 'NONE',  ( 122.4965214775786251, -10.30919188438810075, -12.61870101168855918 ) ) ;
#38622 = EDGE_CURVE ( 'NONE', #10810, #15070, #1156, .T. ) ;
#38623 = CARTESIAN_POINT ( 'NONE',  ( 116.3700414775786527, -5.638512984488999180, -18.83840828888717311 ) ) ;
#38624 = ORIENTED_EDGE ( 'NONE', *, *, #42337, .T. ) ;
#38625 = CARTESIAN_POINT ( 'NONE',  ( 115.0653281442453277, -3.505236298600246325, -18.68346056562440793 ) ) ;
#38626 = CARTESIAN_POINT ( 'NONE',  ( 126.0703014775786102, -9.988377603198980381, -10.36322818467138518 ) ) ;
#38627 = AXIS2_PLACEMENT_3D ( 'NONE', #37568, #34139, #5426 ) ;
#38628 = CARTESIAN_POINT ( 'NONE',  ( 117.5613014775786525, 0.9020085738987339008, -11.91225656197089222 ) ) ;
#38629 = CARTESIAN_POINT ( 'NONE',  ( 117.9016614775786280, -0.1624402480850797581, -16.17319339645315424 ) ) ;
#38630 = EDGE_LOOP ( 'NONE', ( #32204, #20255, #16444, #7229 ) ) ;
#38631 = CARTESIAN_POINT ( 'NONE',  ( 120.9081748109119872, -4.153390946401325223, -8.397313243818185668 ) ) ;
#38632 = AXIS2_PLACEMENT_3D ( 'NONE', #3529, #20869, #18343 ) ;
#38633 = CARTESIAN_POINT ( 'NONE',  ( 116.7104014775786425, -0.4660016031367893996, -10.09054647747474043 ) ) ;
#38634 = CARTESIAN_POINT ( 'NONE',  ( 136.5689201998072804, 0.8250495500204333421, -12.80989719292719009 ) ) ;
#38635 = CARTESIAN_POINT ( 'NONE',  ( 110.4131140045248287, -10.62599879583958717, -11.00651665394454604 ) ) ;
#38636 = AXIS2_PLACEMENT_3D ( 'NONE', #25349, #39243, #35809 ) ;
#38637 = CARTESIAN_POINT ( 'NONE',  ( 69.29215060918571112, -65.97558228610364495, -36.22947046937226645 ) ) ;
#38638 = CARTESIAN_POINT ( 'NONE',  ( 126.4230588806227189, 0.2350761378584792227, -13.57469946490973989 ) ) ;
#38639 = ADVANCED_FACE ( 'NONE', ( #18029 ), #41220, .T. ) ;
#38640 = CARTESIAN_POINT ( 'NONE',  ( 88.22708560785949317, -3.622631779710408395, -18.64321520033831803 ) ) ;
#38641 = CARTESIAN_POINT ( 'NONE',  ( 114.1577014775786552, -6.344957434206662583, -7.627207830600332805 ) ) ;
#38642 = LINE ( 'NONE', #41659, #4015 ) ;
#38643 = CARTESIAN_POINT ( 'NONE',  ( 112.5693548109119888, 0.4262465694468514643, -12.03445270309931736 ) ) ;
#38644 = EDGE_CURVE ( 'NONE', #25324, #32403, #37105, .T. ) ;
#38645 = CARTESIAN_POINT ( 'NONE',  ( 70.19189222814998175, -62.62292920857806422, -38.25196254438899501 ) ) ;
#38646 = DIRECTION ( 'NONE',  ( -0.000000000000000000, -0.9284778069183721172, -0.3713878862591650232 ) ) ;
#38647 = CARTESIAN_POINT ( 'NONE',  ( 116.8722546295247895, -4.863998795839590272, -18.39754474579285315 ) ) ;
#38648 = CARTESIAN_POINT ( 'NONE',  ( 112.7962614775786676, -6.222761293078241884, -8.102969835052219238 ) ) ;
#38649 = CARTESIAN_POINT ( 'NONE',  ( 123.2161110609119703, -6.340755971794695078, -8.611740276972781771 ) ) ;
#38650 = EDGE_CURVE ( 'NONE', #19947, #42200, #12076, .T. ) ;
#38651 = AXIS2_PLACEMENT_3D ( 'NONE', #10486, #24388, #14566 ) ;
#38652 = CARTESIAN_POINT ( 'NONE',  ( 75.14134903615895666, -42.50702760616825771, -16.39321520033831447 ) ) ;
#38654 = CARTESIAN_POINT ( 'NONE',  ( 115.6893214775786447, 0.5811942927096154232, -14.16772938898807155 ) ) ;
#38653 = DIRECTION ( 'NONE',  ( 0.000000000000000000, 0.000000000000000000, 1.000000000000000000 ) ) ;
#38655 = CARTESIAN_POINT ( 'NONE',  ( 123.8579614775786126, -9.859900752359378018, -12.68260735090039759 ) ) ;
#38656 = CARTESIAN_POINT ( 'NONE',  ( 118.4689281442453392, -10.15424416112533912, -14.75197769757731336 ) ) ;
#38657 = ORIENTED_EDGE ( 'NONE', *, *, #43179, .T. ) ;
#38658 = LINE ( 'NONE', #4907, #45014 ) ;
#38659 = CARTESIAN_POINT ( 'NONE',  ( 123.5176014775786228, -9.261995988541697145, -16.69588392320189030 ) ) ;
#38660 = CARTESIAN_POINT ( 'NONE',  ( 114.3024890045248156, -9.868328341294098749, -11.32035403202665869 ) ) ;
#38661 = CARTESIAN_POINT ( 'NONE',  ( 118.6958348109119754, -3.505236298600246325, -18.68346056562440793 ) ) ;
#38662 =( BOUNDED_CURVE ( )  B_SPLINE_CURVE ( 3, ( #34575, #2904, #14069, #30726 ),
 .UNSPECIFIED., .F., .T. ) 
 B_SPLINE_CURVE_WITH_KNOTS ( ( 4, 4 ),
 ( 0.2801472849774039875, 0.7487301044471339484 ),
 .UNSPECIFIED. ) 
 CURVE ( )  GEOMETRIC_REPRESENTATION_ITEM ( )  RATIONAL_B_SPLINE_CURVE ( ( 1.000000000000000000, 0.9817860582945869830, 0.9817860582945869830, 1.000000000000000000 ) ) 
 REPRESENTATION_ITEM ( '' )  );
#38663 = ADVANCED_FACE ( 'NONE', ( #16191 ), #12831, .T. ) ;
#38664 = CARTESIAN_POINT ( 'NONE',  ( 113.7038881442453402, -6.222761293078241884, -8.102969835052219238 ) ) ;
#38665 = CARTESIAN_POINT ( 'NONE',  ( 86.28794317325427699, -26.53699186446346658, -8.429793386229720298 ) ) ;
#38666 = CARTESIAN_POINT ( 'NONE',  ( 111.6632702545248605, -10.62599879583958717, -15.77991374673208469 ) ) ;
#38667 = CARTESIAN_POINT ( 'NONE',  ( 120.1140014775786398, -7.894159318335828068, -9.358103419637847864 ) ) ;
#38668 = CONICAL_SURFACE ( 'NONE', #16836, 1.610000000000000986, 0.9599310885968765916 ) ;
#38669 = CARTESIAN_POINT ( 'NONE',  ( 118.7525614775786380, -1.833838273342659253, -17.42832698103878286 ) ) ;
#38670 = CARTESIAN_POINT ( 'NONE',  ( 116.8238548109119819, -5.574606645277192740, -18.38911715685844328 ) ) ;
#38671 = CARTESIAN_POINT ( 'NONE',  ( 109.2294421335984111, -7.460416756848673003, -8.322835172996224884 ) ) ;
#38672 = CARTESIAN_POINT ( 'NONE',  ( 87.14323352029596492, -25.99489077589524300, -13.39321520033831625 ) ) ;
#38673 = CARTESIAN_POINT ( 'NONE',  ( 109.4407702545248355, 0.1403307496149616695, -11.32035403202665336 ) ) ;
#38674 = PRODUCT_DEFINITION_SHAPE ( 'NONE', 'NONE',  #45149 ) ;
#38675 = EDGE_CURVE ( 'NONE', #31995, #13929, #22422, .T. ) ;
#38676 = FACE_OUTER_BOUND ( 'NONE', #37947, .T. ) ;
#38677 = CARTESIAN_POINT ( 'NONE',  ( 116.4834948109119779, -1.561330072975668504, -17.79121239304076951 ) ) ;
#38678 = CARTESIAN_POINT ( 'NONE',  ( 115.1787814775786387, -9.988377603198976828, -10.36322818467138340 ) ) ;
#38679 = CARTESIAN_POINT ( 'NONE',  ( 109.5796765045248122, -7.250697342233347165, -19.15521520033831138 ) ) ;
#38680 = CARTESIAN_POINT ( 'NONE',  ( 113.3635281442453504, -9.988377603198976828, -10.36322818467138340 ) ) ;
#38681 = EDGE_CURVE ( 'NONE', #2361, #42996, #1860, .T. ) ;
#38682 = EDGE_CURVE ( 'NONE', #30525, #38595, #39011, .T. ) ;
#38683 = VERTEX_POINT ( 'NONE', #20516 ) ;
#38684 = FACE_OUTER_BOUND ( 'NONE', #40835, .T. ) ;
#38685 = CARTESIAN_POINT ( 'NONE',  ( 121.6456214775786293, -10.63000616557722466, -14.87417383870573495 ) ) ;
#38686 = CARTESIAN_POINT ( 'NONE',  ( 116.8238548109119819, -4.089484607189486809, -7.948022111789456723 ) ) ;
#38687 = CARTESIAN_POINT ( 'NONE',  ( 120.2841814775786276, -10.15424416112533912, -14.75197769757731336 ) ) ;
#38688 =( LENGTH_UNIT ( ) NAMED_UNIT ( * ) SI_UNIT ( .MILLI., .METRE. ) );
#38689 = CARTESIAN_POINT ( 'NONE',  ( 125.4463081442452932, -5.638512984488999180, -18.83840828888717311 ) ) ;
#38690 = CARTESIAN_POINT ( 'NONE',  ( 121.1350814775786233, 0.5811942927096110934, -14.16772938898807510 ) ) ;
#38691 = CARTESIAN_POINT ( 'NONE',  ( 115.4137390045248566, 0.8980012041604421569, -15.77991374673208469 ) ) ;
#38692 = AXIS2_PLACEMENT_3D ( 'NONE', #14871, #28782, #15313 ) ;
#38693 = CARTESIAN_POINT ( 'NONE',  ( 116.9940348109119839, -0.1624402480850797581, -16.17319339645315424 ) ) ;
#38694 = CARTESIAN_POINT ( 'NONE',  ( 85.15861813568058380, -25.99489077589524300, -13.39321520033831625 ) ) ;
#38695 = ORIENTED_EDGE ( 'NONE', *, *, #10825, .T. ) ;
#38696 = CARTESIAN_POINT ( 'NONE',  ( 123.1205148109119563, -1.834011780172310813, -8.268836392978581529 ) ) ;
#38697 = CARTESIAN_POINT ( 'NONE',  ( 123.0077516859119839, -9.665098340737509730, -17.37397104707595474 ) ) ;
#38698 = CARTESIAN_POINT ( 'NONE',  ( 120.2274548109119934, 0.5811942927096110934, -14.16772938898807510 ) ) ;
#38699 = VERTEX_POINT ( 'NONE', #37824 ) ;
#38700 = CARTESIAN_POINT ( 'NONE',  ( 107.0099108795247815, -1.325403438956436419, -16.93181055722141792 ) ) ;
#38701 = AXIS2_PLACEMENT_3D ( 'NONE', #19395, #4806, #25350 ) ;
#38702 = FACE_OUTER_BOUND ( 'NONE', #40348, .T. ) ;
#38703 = CARTESIAN_POINT ( 'NONE',  ( 119.6784740574772457, -2.443475742715334853, -17.86549347949429389 ) ) ;
#38704 = CARTESIAN_POINT ( 'NONE',  ( 114.2144281442453178, -1.833838273342658809, -17.42832698103878286 ) ) ;
#38705 = CARTESIAN_POINT ( 'NONE',  ( 124.2610829359119862, -4.360640073283670759, -8.004713379073534085 ) ) ;
#38706 = CARTESIAN_POINT ( 'NONE',  ( 120.6812681442452941, 0.1319031606808879209, -14.10382304977623669 ) ) ;
#38707 = DIRECTION ( 'NONE',  ( 0.000000000000000000, -0.3818493186865936084, 0.9242245927363024194 ) ) ;
#38708 = CARTESIAN_POINT ( 'NONE',  ( 122.7801548109119665, -6.222761293078241884, -8.102969835052219238 ) ) ;
#38709 = ADVANCED_FACE ( 'NONE', ( #16420 ), #34616, .T. ) ;
#38710 = CARTESIAN_POINT ( 'NONE',  ( 86.39381242489322688, -8.190259192973641689, -8.143215200338314474 ) ) ;
#38711 = CARTESIAN_POINT ( 'NONE',  ( 120.3409081442453044, -8.899110576539710493, -16.42337572283490132 ) ) ;
#38712 = CARTESIAN_POINT ( 'NONE',  ( 122.5215798109119874, -2.173413727453600508, -8.297982527556802879 ) ) ;
#38713 = CARTESIAN_POINT ( 'NONE',  ( 115.5191414775786569, -3.383040157471821630, -19.15922257007629170 ) ) ;
#38714 = CARTESIAN_POINT ( 'NONE',  ( 112.7395348109119766, -5.638512984488999180, -18.83840828888717311 ) ) ;
#38715 = DIRECTION ( 'NONE',  ( -1.000000000000000000, 0.000000000000000000, -0.000000000000000000 ) ) ;
#38716 = CARTESIAN_POINT ( 'NONE',  ( 119.3765548109119834, -10.15424416112533912, -14.75197769757731336 ) ) ;
#38717 = ORIENTED_EDGE ( 'NONE', *, *, #7486, .T. ) ;
#38718 = CARTESIAN_POINT ( 'NONE',  ( 115.7460481442453357, 0.9020085738987339008, -11.91225656197089222 ) ) ;
#38719 = CARTESIAN_POINT ( 'NONE',  ( 114.9275671295247889, 0.1403307496149613920, -13.39321520033831447 ) ) ;
#38720 = CARTESIAN_POINT ( 'NONE',  ( 70.19189222814998175, -54.47411573338475677, -34.99246555962335492 ) ) ;
#38721 = CARTESIAN_POINT ( 'NONE',  ( 87.44708369096657918, -25.99489077589588604, -15.39321520033831625 ) ) ;
#38722 = VECTOR ( 'NONE', #34429, 1000.000000000000000 ) ;
#38723 = CARTESIAN_POINT ( 'NONE',  ( 124.2550481442452792, -9.988377603198980381, -10.36322818467138518 ) ) ;
#38724 = EDGE_LOOP ( 'NONE', ( #19925, #39707, #9754, #44411, #10304 ) ) ;
#38725 = CARTESIAN_POINT ( 'NONE',  ( 126.5561942423852315, -8.491916856930616930, -9.711375107224954562 ) ) ;
#38726 = CARTESIAN_POINT ( 'NONE',  ( 121.3619881442452879, -5.574606645277164318, -18.38911715685844683 ) ) ;
#38727 = CARTESIAN_POINT ( 'NONE',  ( 120.5768923109119868, -9.959231468620755479, -10.70263013195267199 ) ) ;
#38728 = CARTESIAN_POINT ( 'NONE',  ( 65.34856691214200453, -14.13229026159626045, -17.32302191349986487 ) ) ;
#38729 = ADVANCED_FACE ( 'NONE', ( #20957 ), #16513, .T. ) ;
#38730 = DIRECTION ( 'NONE',  ( 0.5735764363510498232, -0.3127926500124802445, 0.7570804645221007600 ) ) ;
#38731 = CARTESIAN_POINT ( 'NONE',  ( 110.6909265045248247, -2.791137627527939813, -8.388885654883777576 ) ) ;
#38732 = CYLINDRICAL_SURFACE ( 'NONE', #15558, 0.8999999999999980238 ) ;
#38733 = EDGE_LOOP ( 'NONE', ( #43596, #15481, #18573, #33075 ) ) ;
#38734 = CARTESIAN_POINT ( 'NONE',  ( 116.2565881442452991, -9.261995988541697145, -16.69588392320189030 ) ) ;
#38735 = AXIS2_PLACEMENT_3D ( 'NONE', #16894, #41294, #3192 ) ;
#38736 = CARTESIAN_POINT ( 'NONE',  ( 125.2194014775786286, 0.1319031606808879209, -14.10382304977623669 ) ) ;
#38737 = CARTESIAN_POINT ( 'NONE',  ( 124.0281414775786146, -1.834011780172310813, -8.268836392978581529 ) ) ;
#38738 = ADVANCED_FACE ( 'NONE', ( #6831, #34396, #27582 ), #20736, .T. ) ;
#38739 = CARTESIAN_POINT ( 'NONE',  ( 119.4900081442453086, -7.643976991954077427, -18.09477374809248928 ) ) ;
#38740 = CARTESIAN_POINT ( 'NONE',  ( 126.2275303246277502, -4.044442676264679015, -8.456153826979251775 ) ) ;
#38741 = CARTESIAN_POINT ( 'NONE',  ( 124.0848681442452772, -4.089484607189486809, -7.948022111789456723 ) ) ;
#38742 = CARTESIAN_POINT ( 'NONE',  ( 111.8424481442453242, -6.210324830718715994, -8.151390318758327425 ) ) ;
#38743 = ADVANCED_FACE ( 'NONE', ( #30767 ), #7046, .F. ) ;
#38744 = CARTESIAN_POINT ( 'NONE',  ( 70.19189222814998175, -100.0979043305785581, -53.24182196210380624 ) ) ;
#38745 = CARTESIAN_POINT ( 'NONE',  ( 68.42836698684014607, -67.15337231239986693, -42.03592829731906733 ) ) ;
#38746 = DIRECTION ( 'NONE',  ( 0.000000000000000000, 0.000000000000000000, 1.000000000000000000 ) ) ;
#38747 = VERTEX_POINT ( 'NONE', #44242 ) ;
#38748 = LINE ( 'NONE', #6862, #1585 ) ;
#38749 = CARTESIAN_POINT ( 'NONE',  ( 120.0005481442453146, -5.638512984488999180, -18.83840828888717311 ) ) ;
#38750 = SHAPE_REPRESENTATION ( 'Adjuster Locknut', ( #12375 ), #32226 ) ;
#38751 = CARTESIAN_POINT ( 'NONE',  ( 136.7478768735732046, -8.464786658626188398, -17.71247759265823873 ) ) ;
#38752 = VERTEX_POINT ( 'NONE', #10036 ) ;
#38753 = CARTESIAN_POINT ( 'NONE',  ( 67.84197459855160162, -55.51165166589005651, -36.13664933202900897 ) ) ;
#38754 = CARTESIAN_POINT ( 'NONE',  ( 122.7801548109119665, -3.383040157471821630, -19.15922257007629170 ) ) ;
#38755 = CARTESIAN_POINT ( 'NONE',  ( 107.4266296295248821, -4.863998795839590272, -19.15521520033831493 ) ) ;
#38756 = CARTESIAN_POINT ( 'NONE',  ( 123.5743281442453139, -2.084020599724406786, -8.691656652584148546 ) ) ;
#38757 = ORIENTED_EDGE ( 'NONE', *, *, #14764, .T. ) ;
#38758 = CARTESIAN_POINT ( 'NONE',  ( 113.8740681442453138, 0.5811942927096154232, -14.16772938898807155 ) ) ;
#38759 = CARTESIAN_POINT ( 'NONE',  ( 87.44708369096657918, -21.99489077589588604, -20.89321520033831447 ) ) ;
#38760 = DIRECTION ( 'NONE',  ( -0.000000000000000000, -0.9284778069183718952, -0.3713878862591649677 ) ) ;
#38761 = MECHANICAL_DESIGN_GEOMETRIC_PRESENTATION_REPRESENTATION (  '', ( #13317 ), #29344 ) ;
#38762 = CARTESIAN_POINT ( 'NONE',  ( 60.06931813437629586, -14.72076136720887085, -18.18301750815651374 ) ) ;
#38763 = CARTESIAN_POINT ( 'NONE',  ( 111.4348214775786801, -3.505236298600246325, -18.68346056562440793 ) ) ;
#38764 = CARTESIAN_POINT ( 'NONE',  ( 122.9251895652850521, -6.239497348973043422, -18.71779138178828106 ) ) ;
#38765 = AXIS2_PLACEMENT_3D ( 'NONE', #11858, #910, #15496 ) ;
#38766 = CARTESIAN_POINT ( 'NONE',  ( 69.51487126532624927, -51.06495315005575719, -31.09787670850536756 ) ) ;
#38767 = CARTESIAN_POINT ( 'NONE',  ( 123.4608748109119745, -10.63000616557722466, -14.87417383870573495 ) ) ;
#38769 = CARTESIAN_POINT ( 'NONE',  ( 123.8012348109119642, -9.565557343593413364, -10.61323700422348004 ) ) ;
#38768 = CARTESIAN_POINT ( 'NONE',  ( 122.2128881442453263, -1.834011780172310813, -8.268836392978581529 ) ) ;
#38770 = CARTESIAN_POINT ( 'NONE',  ( 120.7379948109119709, 0.4262465694468514643, -12.03445270309931736 ) ) ;
#38771 = CARTESIAN_POINT ( 'NONE',  ( 125.6626748109119802, -9.522524984348629928, -10.63868154973292768 ) ) ;
#38772 = CARTESIAN_POINT ( 'NONE',  ( 117.3343948109119737, -3.383040157471821630, -19.15922257007629170 ) ) ;
#38773 = VERTEX_POINT ( 'NONE', #3177 ) ;
#38774 = ADVANCED_FACE ( 'NONE', ( #17100, #13226 ), #44917, .T. ) ;
#38775 = VERTEX_POINT ( 'NONE', #23490 ) ;
#38776 = DIRECTION ( 'NONE',  ( 0.000000000000000000, -0.9242245927363029745, -0.3818493186865927203 ) ) ;
#38777 = DIRECTION ( 'NONE',  ( 0.000000000000000000, 0.000000000000000000, -1.000000000000000000 ) ) ;
#38778 = CARTESIAN_POINT ( 'NONE',  ( 112.5661608795247872, -1.325403438956436419, -16.93181055722141792 ) ) ;
#38779 = CARTESIAN_POINT ( 'NONE',  ( 109.6491296295247793, -4.863998795839590272, -8.388885654883775800 ) ) ;
#38780 = CARTESIAN_POINT ( 'NONE',  ( 111.7327233795247849, -1.325403438956436419, -9.854619843455211026 ) ) ;
#38781 = CARTESIAN_POINT ( 'NONE',  ( 125.5030348109119558, -3.383040157471821630, -19.15922257007629170 ) ) ;
#38782 = CARTESIAN_POINT ( 'NONE',  ( 124.9924948109119924, -5.574606645277164318, -18.38911715685844683 ) ) ;
#38783 = VERTEX_POINT ( 'NONE', #20066 ) ;
#38784 = CARTESIAN_POINT ( 'NONE',  ( 112.5126281442453120, 0.1319031606808879209, -14.10382304977623669 ) ) ;
#38785 = CARTESIAN_POINT ( 'NONE',  ( 110.5520202545248054, -10.62599879583958717, -15.77991374673208469 ) ) ;
#38786 = CARTESIAN_POINT ( 'NONE',  ( 94.20708369096698220, -27.10035099198479358, -13.29271931396930739 ) ) ;
#38787 = DIRECTION ( 'NONE',  ( 0.5735764363510499342, 0.3127926500124801890, -0.7570804645221008711 ) ) ;
#38788 = CARTESIAN_POINT ( 'NONE',  ( 123.0637881442452937, -0.4660016031367893996, -10.09054647747474043 ) ) ;
#38789 = CARTESIAN_POINT ( 'NONE',  ( 79.33697550240769658, 5.018751399745532638, -6.205043556752605660 ) ) ;
#38790 = CARTESIAN_POINT ( 'NONE',  ( 114.4980614775786592, -7.893985811506177619, -18.51759400769804742 ) ) ;
#38791 = CARTESIAN_POINT ( 'NONE',  ( 114.3719421295247827, 0.8980012041604618078, -13.39321520033831447 ) ) ;
#38792 = CARTESIAN_POINT ( 'NONE',  ( 111.3854577545248645, -2.791137627527939813, -18.39754474579286025 ) ) ;
#38793 = ORIENTED_EDGE ( 'NONE', *, *, #4136, .T. ) ;
#38794 = DIRECTION ( 'NONE',  ( 0.000000000000000000, 0.000000000000000000, 1.000000000000000000 ) ) ;
#38795 = CARTESIAN_POINT ( 'NONE',  ( 116.0864081442453113, -0.1624402480850797581, -16.17319339645315424 ) ) ;
#38796 = AXIS2_PLACEMENT_3D ( 'NONE', #34307, #27034, #12910 ) ;
#38797 = CARTESIAN_POINT ( 'NONE',  ( 113.9307948109119906, 0.9020085738987339008, -11.91225656197089222 ) ) ;
#38798 = EDGE_CURVE ( 'NONE', #15657, #25112, #16876, .T. ) ;
#38799 = CARTESIAN_POINT ( 'NONE',  ( 113.0231681442453322, 0.9020085738987339008, -11.91225656197089222 ) ) ;
#38800 = CARTESIAN_POINT ( 'NONE',  ( 118.3554748109119856, -9.565557343593388495, -10.61323700422345162 ) ) ;
#38801 = UNCERTAINTY_MEASURE_WITH_UNIT (LENGTH_MEASURE( 1.000000000000000082E-05 ), #15721, 'distance_accuracy_value', 'NONE');
#38802 = CARTESIAN_POINT ( 'NONE',  ( 121.3052614775786111, -7.643976991954077427, -18.09477374809248928 ) ) ;
#38803 = CARTESIAN_POINT ( 'NONE',  ( 125.8433948109119456, -1.834011780172310813, -8.268836392978581529 ) ) ;
#38804 = EDGE_LOOP ( 'NONE', ( #38039, #37293 ) ) ;
#38805 = AXIS2_PLACEMENT_3D ( 'NONE', #27742, #42315, #136 ) ;
#38806 = CARTESIAN_POINT ( 'NONE',  ( 121.2714235609119697, -9.645473719204776586, -14.86997237629376656 ) ) ;
#38807 = AXIS2_PLACEMENT_3D ( 'NONE', #31362, #23880, #6308 ) ;
#38808 = CARTESIAN_POINT ( 'NONE',  ( 113.4872481608379786, 0.3867979994853637526, -14.64321520033833401 ) ) ;
#38809 = CARTESIAN_POINT ( 'NONE',  ( 113.5904348109119866, -2.084020599724406786, -8.691656652584148546 ) ) ;
#38810 = ORIENTED_EDGE ( 'NONE', *, *, #7243, .T. ) ;
#38811 = DIRECTION ( 'NONE',  ( -0.9908103287288504424, 0.1352586133457950035, 0.000000000000000000 ) ) ;
#38812 = DIRECTION ( 'NONE',  ( 0.000000000000000000, 1.000000000000000000, 0.000000000000000000 ) ) ;
#38813 = CARTESIAN_POINT ( 'NONE',  ( 112.3578015045248861, -6.936859964151250502, -18.39754474579286025 ) ) ;
#38814 = CARTESIAN_POINT ( 'NONE',  ( 122.7801548109119665, -6.222761293078241884, -8.102969835052219238 ) ) ;
#38815 = VERTEX_POINT ( 'NONE', #41498 ) ;
#38816 = CARTESIAN_POINT ( 'NONE',  ( 117.5613014775786525, -10.15424416112533912, -14.75197769757731336 ) ) ;
#38817 = CARTESIAN_POINT ( 'NONE',  ( 117.6747548109119919, -7.643976991954077427, -18.09477374809248928 ) ) ;
#38818 = CARTESIAN_POINT ( 'NONE',  ( 69.69189222814998175, -41.76310523276723785, -24.39321520033831447 ) ) ;
#38819 = CARTESIAN_POINT ( 'NONE',  ( 121.1325173109119788, 0.2312338769422704887, -16.08380026872395874 ) ) ;
#38820 = ORIENTED_EDGE ( 'NONE', *, *, #40951, .F. ) ;
#38821 = AXIS2_PLACEMENT_3D ( 'NONE', #23513, #9597, #5707 ) ;
#38822 = CARTESIAN_POINT ( 'NONE',  ( 74.19189222814998175, -41.76310523276723785, -6.393215200338315363 ) ) ;
#38823 = CARTESIAN_POINT ( 'NONE',  ( 84.38170309240724976, -25.23119213852205789, -15.24166438581092109 ) ) ;
#38824 = CARTESIAN_POINT ( 'NONE',  ( 113.2606921295247702, 0.8980012041604618078, -13.39321520033831447 ) ) ;
#38825 = CIRCLE ( 'NONE', #23559, 4.000000000000000888 ) ;
#38826 = CARTESIAN_POINT ( 'NONE',  ( 111.9453614775786434, -1.561330072975668060, -17.79121239304076596 ) ) ;
#38827 = CARTESIAN_POINT ( 'NONE',  ( 126.1837548109119496, 0.4262465694468514643, -12.03445270309931736 ) ) ;
#38828 = CARTESIAN_POINT ( 'NONE',  ( 117.9583881442453048, 0.1319031606808879209, -14.10382304977623669 ) ) ;
#38829 = CARTESIAN_POINT ( 'NONE',  ( 138.2184548109119930, 2.066246953222917959, -14.37896053134723040 ) ) ;
#38830 = ORIENTED_EDGE ( 'NONE', *, *, #6443, .T. ) ;
#38831 = CARTESIAN_POINT ( 'NONE',  ( 114.6115148109119986, -6.222761293078241884, -8.102969835052219238 ) ) ;
#38832 = CARTESIAN_POINT ( 'NONE',  ( 115.2748327545248657, -2.477300249445798297, -19.15521520033831138 ) ) ;
#38833 = AXIS2_PLACEMENT_3D ( 'NONE', #39388, #14539, #17960 ) ;
#38834 = CARTESIAN_POINT ( 'NONE',  ( 84.59925623653033711, -29.75466480065543706, -10.12692979306177143 ) ) ;
#38835 = CARTESIAN_POINT ( 'NONE',  ( 92.32016463086877422, -27.84333996136784961, -14.15691383771150136 ) ) ;
#38836 = CARTESIAN_POINT ( 'NONE',  ( 114.1577014775786552, -6.344957434206662583, -7.627207830600332805 ) ) ;
#38837 = VERTEX_POINT ( 'NONE', #33951 ) ;
#38838 = CARTESIAN_POINT ( 'NONE',  ( 118.3554748109119998, 0.2603800115204892296, -16.42320221600525088 ) ) ;
#38839 = CARTESIAN_POINT ( 'NONE',  ( 123.9584548109119737, -11.17722486020181627, -8.479644537342501565 ) ) ;
#38840 = CARTESIAN_POINT ( 'NONE',  ( 113.3995983795247895, -0.7896495226426338832, -9.318865927141430916 ) ) ;
#38841 = CARTESIAN_POINT ( 'NONE',  ( 114.2711548109119803, -9.988377603198976828, -10.36322818467138340 ) ) ;
#38842 = CARTESIAN_POINT ( 'NONE',  ( 115.2922348109119781, -10.63000616557722466, -14.87417383870573495 ) ) ;
#38843 = CARTESIAN_POINT ( 'NONE',  ( 127.0264730702700433, -10.25983759373953319, -13.69028692805868452 ) ) ;
#38844 = CARTESIAN_POINT ( 'NONE',  ( 121.9470836909669913, -25.99489077589524300, -13.39321520033831447 ) ) ;
#38845 = CARTESIAN_POINT ( 'NONE',  ( 111.5938171295247940, 0.1403307496149613920, -13.39321520033831447 ) ) ;
#38846 = B_SPLINE_CURVE_WITH_KNOTS ( 'NONE', 3,
 ( #32142, #39215, #14830, #21887, #42645, #35783, #4552, #18478, #32367, #1134, #15052, #12761, #9560, #19590, #44449, #37124, #26885, #40346, #40804, #12989, #23476, #13216, #37362, #20053, #5672, #26661, #9795, #22782, #33471, #2251 ),
 .UNSPECIFIED., .F., .F.,
 ( 4, 2, 2, 1, 1, 1, 2, 2, 2, 1, 1, 1, 2, 2, 1, 1, 2, 2, 4 ),
 ( 0.000000000000000000, 0.2499999999998695488, 0.3749999999997916111, 0.4374999999997516986, 0.4687499999997186140, 0.4843749999996893041, 0.4921874999996895261, 0.4999999999996898037, 0.6249999999999032996, 0.6875000000000216493, 0.7187500000000807132, 0.7343750000000988098, 0.7421875000001069145, 0.7500000000001149081, 0.8125000000000915934, 0.8437500000000796030, 0.8593750000000660583, 0.8750000000000524025, 1.000000000000000000 ),
 .UNSPECIFIED. ) ;
#38847 = EDGE_LOOP ( 'NONE', ( #36811, #986, #25830, #7400 ) ) ;
#38848 = CARTESIAN_POINT ( 'NONE',  ( 112.3058127483929383, -2.423081321603721694, -17.89265170041262465 ) ) ;
#38849 = CARTESIAN_POINT ( 'NONE',  ( 109.2296393276947271, -6.249043720356506348, -18.46636368634833048 ) ) ;
#38850 = CARTESIAN_POINT ( 'NONE',  ( 115.2922348109119781, 0.4262465694468514643, -12.03445270309931736 ) ) ;
#38851 = ADVANCED_FACE ( 'NONE', ( #2719 ), #16645, .F. ) ;
#38852 = CARTESIAN_POINT ( 'NONE',  ( 64.41506894153299356, -13.04641652406104946, -11.17147419670170194 ) ) ;
#38853 = CARTESIAN_POINT ( 'NONE',  ( 118.0151148109119816, -10.63000616557722111, -14.87417383870573850 ) ) ;
#38854 = CARTESIAN_POINT ( 'NONE',  ( 107.4266296295248821, -4.863998795839590272, -19.15521520033831493 ) ) ;
#38855 = CARTESIAN_POINT ( 'NONE',  ( 127.0915067942480192, -5.196864950038682984, -7.966870886606466584 ) ) ;
#38856 = CARTESIAN_POINT ( 'NONE',  ( 115.6325948109119821, -9.565557343593413364, -10.61323700422348004 ) ) ;
#38857 = CYLINDRICAL_SURFACE ( 'NONE', #59, 5.000000000000000888 ) ;
#38858 = CARTESIAN_POINT ( 'NONE',  ( 125.7299414775786346, 0.9020085738987339008, -11.91225656197089222 ) ) ;
#38859 = CARTESIAN_POINT ( 'NONE',  ( 115.8595014775786609, -1.834011780172310813, -8.268836392978581529 ) ) ;
#38860 = ORIENTED_EDGE ( 'NONE', *, *, #2161, .T. ) ;
#38861 = CARTESIAN_POINT ( 'NONE',  ( 115.2922348109119781, 0.4262465694468514643, -12.03445270309931736 ) ) ;
#38862 = CARTESIAN_POINT ( 'NONE',  ( 112.0588148109119828, 0.5811942927096154232, -14.16772938898807155 ) ) ;
#38863 = CARTESIAN_POINT ( 'NONE',  ( 117.3343948109119737, -3.383040157471821630, -19.15922257007629170 ) ) ;
#38864 = CARTESIAN_POINT ( 'NONE',  ( 117.8449348109119938, -1.833838273342659253, -17.42832698103878286 ) ) ;
#38865 = ORIENTED_EDGE ( 'NONE', *, *, #31425, .T. ) ;
#38866 = CARTESIAN_POINT ( 'NONE',  ( 122.3263414775786373, -3.505236298600246325, -18.68346056562440793 ) ) ;
#38867 = AXIS2_PLACEMENT_3D ( 'NONE', #1745, #5614, #22501 ) ;
#38868 = CARTESIAN_POINT ( 'NONE',  ( 116.7671281442453335, -1.834011780172310813, -8.268836392978581529 ) ) ;
#38869 = CYLINDRICAL_SURFACE ( 'NONE', #41315, 1.000000000000000888 ) ;
#38870 = CARTESIAN_POINT ( 'NONE',  ( 110.2742077545248094, -7.250697342233347165, -7.631215200338321125 ) ) ;
#38871 = CARTESIAN_POINT ( 'NONE',  ( 60.91427317013854292, -14.50360402731886644, -8.693199542283664982 ) ) ;
#38872 = CARTESIAN_POINT ( 'NONE',  ( 116.8928740015602870, 0.2848729546123598966, -14.64321520033831447 ) ) ;
#38873 = CARTESIAN_POINT ( 'NONE',  ( 115.4137390045248566, -9.868328341294098749, -11.32035403202665869 ) ) ;
#38874 = CARTESIAN_POINT ( 'NONE',  ( 112.9664414775786412, 0.5811942927096154232, -14.16772938898807155 ) ) ;
#38875 = CARTESIAN_POINT ( 'NONE',  ( 117.1020249174801506, 1.596432964241469188, -5.416842142801578497 ) ) ;
#38876 = CARTESIAN_POINT ( 'NONE',  ( 115.2922348109119781, 0.4262465694468514643, -12.03445270309931736 ) ) ;
#38877 = DIRECTION ( 'NONE',  ( 0.9609149988134837450, -0.1028163501681639419, 0.2570431154366518145 ) ) ;
#38878 = DIRECTION ( 'NONE',  ( -1.000000000000000000, 0.000000000000000000, 0.000000000000000000 ) ) ;
#38879 = CARTESIAN_POINT ( 'NONE',  ( 113.6079577545248043, -2.791137627527939813, -18.39754474579286025 ) ) ;
#38880 = CARTESIAN_POINT ( 'NONE',  ( 114.4413348109119823, -0.8288870151387760510, -10.36305467784173118 ) ) ;
#38881 = AXIS2_PLACEMENT_3D ( 'NONE', #40413, #27181, #2315 ) ;
#38882 = DIRECTION ( 'NONE',  ( 0.9609149988134837450, -0.1028163501681639419, 0.2570431154366518145 ) ) ;
#38883 = CARTESIAN_POINT ( 'NONE',  ( 73.07463722459043254, -53.85408697697087632, -33.84994832705423562 ) ) ;
#38885 = CARTESIAN_POINT ( 'NONE',  ( 119.6601881442453106, -8.166667518702819706, -8.995218007635861213 ) ) ;
#38884 = CARTESIAN_POINT ( 'NONE',  ( 64.81496985121363252, -15.50732193479129606, -9.201218580878807174 ) ) ;
#38886 = CARTESIAN_POINT ( 'NONE',  ( 123.4041481442452834, 0.1319031606808879209, -14.10382304977623669 ) ) ;
#38887 = CARTESIAN_POINT ( 'NONE',  ( 117.6180281442453150, -8.899110576539710493, -16.42337572283490132 ) ) ;
#38888 = CARTESIAN_POINT ( 'NONE',  ( 113.2500748109119968, -3.505236298600246325, -18.68346056562440793 ) ) ;
#38889 = ORIENTED_EDGE ( 'NONE', *, *, #27064, .T. ) ;
#38890 = CARTESIAN_POINT ( 'NONE',  ( 137.5082292857711650, -8.089093314163772419, -9.561117199659015853 ) ) ;
#38891 = CARTESIAN_POINT ( 'NONE',  ( 123.0070614775786169, 0.9020085738987339008, -11.91225656197089222 ) ) ;
#38892 = CARTESIAN_POINT ( 'NONE',  ( 114.2330358795247776, -8.402594152722688392, -9.854619843455216355 ) ) ;
#38893 = CARTESIAN_POINT ( 'NONE',  ( 118.7525614775786380, -1.833838273342659253, -17.42832698103878286 ) ) ;
#38894 = CARTESIAN_POINT ( 'NONE',  ( 114.6115148109119986, -6.222761293078241884, -8.102969835052219238 ) ) ;
#38895 = CARTESIAN_POINT ( 'NONE',  ( 85.34837758929681684, -28.81250896213596135, -9.554009972945269880 ) ) ;
#38896 = CARTESIAN_POINT ( 'NONE',  ( 112.9134265045247645, -7.250697342233347165, -19.15521520033831138 ) ) ;
#38897 = CARTESIAN_POINT ( 'NONE',  ( 120.0572748109119772, -6.222761293078241884, -8.102969835052219238 ) ) ;
#38898 = CARTESIAN_POINT ( 'NONE',  ( 124.3117748109119844, 0.1319031606808879209, -14.10382304977623669 ) ) ;
#38899 = CARTESIAN_POINT ( 'NONE',  ( 116.5944421295247793, -9.868328341294093420, -13.39321520033827007 ) ) ;
#38900 = CARTESIAN_POINT ( 'NONE',  ( 109.2295733927577146, -1.759256525978093677, -8.933306666141186625 ) ) ;
#38901 = CARTESIAN_POINT ( 'NONE',  ( 123.9800954359119771, -11.07370829466463569, -12.81314460846529002 ) ) ;
#38902 = CARTESIAN_POINT ( 'NONE',  ( 113.3995983795247895, -0.7896495226426338832, -9.318865927141430916 ) ) ;
#38903 = LINE ( 'NONE', #25241, #40817 ) ;
#38904 = CARTESIAN_POINT ( 'NONE',  ( 118.3554748109119998, 0.2603800115204892296, -16.42320221600525088 ) ) ;
#38905 = CARTESIAN_POINT ( 'NONE',  ( 114.5547881442453217, -5.638512984488999180, -18.83840828888717311 ) ) ;
#38906 = CARTESIAN_POINT ( 'NONE',  ( 112.0799890045248475, 0.8980012041604421569, -15.77991374673208469 ) ) ;
#38907 = CARTESIAN_POINT ( 'NONE',  ( 114.3278814775786429, -10.30919188438810075, -12.61870101168855918 ) ) ;
#38908 = ORIENTED_EDGE ( 'NONE', *, *, #13061, .T. ) ;
#38909 = CARTESIAN_POINT ( 'NONE',  ( 63.56235174433628998, -1.192518024930046661, -17.37770299495512205 ) ) ;
#38910 = AXIS2_PLACEMENT_3D ( 'NONE', #38818, #25383, #526 ) ;
#38911 = CARTESIAN_POINT ( 'NONE',  ( 123.9146881442452894, 0.9020085738987339008, -11.91225656197089222 ) ) ;
#38912 = CARTESIAN_POINT ( 'NONE',  ( 115.0086014775786509, -4.089484607189486809, -7.948022111789456723 ) ) ;
#38913 = CARTESIAN_POINT ( 'NONE',  ( 122.0994348109119443, -10.15424416112533912, -14.75197769757731336 ) ) ;
#38914 = PRODUCT_CONTEXT ( 'NONE', #23025, 'mechanical' ) ;
#38915 = CARTESIAN_POINT ( 'NONE',  ( 124.3685014775786328, -10.63000616557722466, -14.87417383870573495 ) ) ;
#38916 = CARTESIAN_POINT ( 'NONE',  ( 122.3830681442452857, -8.166667518702819706, -8.995218007635861213 ) ) ;
#38917 = VECTOR ( 'NONE', #7532, 1000.000000000000000 ) ;
#38918 = ADVANCED_FACE ( 'NONE', ( #27799 ), #26898, .T. ) ;
#38919 = CARTESIAN_POINT ( 'NONE',  ( 115.4831921295247952, 0.8980012041604618078, -13.39321520033831447 ) ) ;
#38920 = CARTESIAN_POINT ( 'NONE',  ( 115.1787814775786387, -0.1624402480850797581, -16.17319339645315424 ) ) ;
#38921 = CARTESIAN_POINT ( 'NONE',  ( 123.6781775979231384, -6.000908072660331882, -18.26596850864147470 ) ) ;
#38922 = ORIENTED_EDGE ( 'NONE', *, *, #25875, .F. ) ;
#38923 = CARTESIAN_POINT ( 'NONE',  ( 121.0216281442452981, -1.561330072975668948, -17.79121239304076951 ) ) ;
#38924 = CARTESIAN_POINT ( 'NONE',  ( 121.8270485609119760, -10.36940331770106916, -15.09355782777062061 ) ) ;
#38925 = CARTESIAN_POINT ( 'NONE',  ( 117.7314814775786260, -4.089484607189486809, -7.948022111789456723 ) ) ;
#38926 = VERTEX_POINT ( 'NONE', #41051 ) ;
#38927 = CARTESIAN_POINT ( 'NONE',  ( 106.7320983795247855, -8.402594152722688392, -16.93181055722141792 ) ) ;
#38928 = CARTESIAN_POINT ( 'NONE',  ( 64.67456875498254476, -2.676871470862063340, -8.178078223173255168 ) ) ;
#38929 = FACE_OUTER_BOUND ( 'NONE', #21323, .T. ) ;
#38930 = CARTESIAN_POINT ( 'NONE',  ( 117.2776681442452968, -4.153390946401321671, -8.397313243818183892 ) ) ;
#38931 = EDGE_CURVE ( 'NONE', #38146, #1246, #9808, .T. ) ;
#38932 = CARTESIAN_POINT ( 'NONE',  ( 127.5515731338752516, -0.8914282735556431359, -17.43429686027660352 ) ) ;
#38933 = CARTESIAN_POINT ( 'NONE',  ( 64.40742206494232391, -35.25845966367313622, -5.871648730333305366 ) ) ;
#38934 =( BOUNDED_SURFACE ( )  B_SPLINE_SURFACE ( 1, 2, ( 
 ( #13185, #20250, #16372, #30275, #44200, #40771, #16834, #6101, #30727, #2674, #44650, #16606, #41233, #23902, #37785, #6558, #20475, #30951, #34356, #17059, #44875, #13631, #27542, #14516, #31384, #605, #28428, #38226, #42341, #24560, #28210, #20917, #32056, #380, #17279, #42561, #31611, #3360, #11100, #31170, #25002, #7665, #14292, #34792, #14744, #20698, #45091, #823, #25233, #21581, #28655, #3575, #35238, #38896, #17487, #18160, #17937, #21354, #155, #6789, #11322, #42118, #34576, #13847, #14070, #38446, #24342, #10878, #10654, #7434, #24775, #38666, #27762, #10435, #27988, #3787, #7217, #4014, #35468, #41677, #31836, #4243, #7008, #21129, #41893, #35004, #17712, #29321, #15870, #12453, #15642, #1494, #36597, #43234, #29093, #12000, #22031, #39130, #21804, #32503, #19290, #1277, #18830, #11551, #14965, #7897, #15189, #42790, #39809, #39588, #15416, #4915, #25903, #18611, #35697, #5373, #32722, #43463, #8575, #32943, #43004, #18393, #1719, #8349, #43678, #1050, #28878, #4473, #32285, #29546, #11773, #22701, #22476, #36370, #22252, #25459, #39362, #12228, #33169, #25681, #36147, #5141, #19057, #26125, #1945, #35925, #8129, #40030, #4692, #8794, #29768, #34084, #33617, #26354, #12681, #34308, #40493, #19733, #9707, #44596, #13131 ),
 ( #22926, #40262, #6041, #33389, #3081, #23620, #37506, #23387, #30676, #19964, #17009, #36819, #9028, #33852, #2163, #30898, #6280, #20200, #2851, #16783, #16554, #20424, #13359, #27265, #12911, #44821, #41178, #2394, #9938, #23852, #37738, #6509, #2621, #5588, #19511, #37273, #16323, #16090, #29995, #26579, #30225, #30449, #44369, #27035, #23162, #43912, #9254, #37043, #40950, #5813, #44145, #26807, #40717, #9476, #21077, #20648, #34954, #3740, #6738, #24950, #7166, #11047, #7386, #24508, #38845, #21304, #38180, #35186, #3964, #45041, #17885, #31334, #17663, #27713, #7615, #31559, #24070, #4191, #38393, #10163, #31782, #37962, #555, #14465, #328, #41627, #21528, #3523, #18110, #34525, #14240, #31117, #6957, #10383, #13801, #24293, #28372, #10824, #20862, #42286, #35415, #32003, #34742, #13578, #41846, #3302, #17441, #14021, #108, #41407, #28157, #27489, #17227, #27936, #42067, #10606, #24722, #38610, #35866, #4639, #9141, #35647, #23046, #1226, #12570, #7849, #32675, #18561, #36933, #1443, #12794, #21754, #42737, #11721, #5704, #19621, #39537, #9365, #42513, #766, #25634, #4421, #23274, #43804, #26475, #33505, #29887, #36096, #40607, #2284, #16214, #32452, #5932, #30117, #21978, #44032, #40379, #26695, #37156, #8298, #19854 ) ),
 .UNSPECIFIED., .F., .F., .T. ) 
 B_SPLINE_SURFACE_WITH_KNOTS ( ( 2, 2 ),
 ( 3, 2, 2, 2, 2, 2, 2, 2, 2, 2, 2, 2, 2, 2, 2, 2, 2, 2, 2, 2, 2, 2, 2, 2, 2, 2, 2, 2, 2, 2, 2, 2, 2, 2, 2, 2, 2, 2, 2, 2, 2, 2, 2, 2, 2, 2, 2, 2, 2, 2, 2, 2, 2, 2, 2, 2, 2, 2, 2, 2, 2, 2, 2, 2, 2, 2, 2, 2, 2, 2, 2, 2, 2, 2, 2, 2, 2, 2, 2, 2, 3 ),
 ( 0.000000000000000000, 1.000000000000000000 ),
 ( 0.000000000000000000, 0.01250000000000000069, 0.02500000000000000139, 0.03749999999999999861, 0.05000000000000000278, 0.06250000000000000000, 0.07499999999999999722, 0.08749999999999999445, 0.1000000000000000056, 0.1125000000000000028, 0.1250000000000000000, 0.1375000000000000111, 0.1499999999999999944, 0.1625000000000000056, 0.1749999999999999889, 0.1875000000000000000, 0.2000000000000000111, 0.2124999999999999944, 0.2250000000000000056, 0.2374999999999999889, 0.2500000000000000000, 0.2625000000000000111, 0.2750000000000000222, 0.2874999999999999778, 0.2999999999999999889, 0.3125000000000000000, 0.3250000000000000111, 0.3375000000000000222, 0.3499999999999999778, 0.3624999999999999889, 0.3750000000000000000, 0.3875000000000000111, 0.4000000000000000222, 0.4124999999999999778, 0.4249999999999999889, 0.4375000000000000000, 0.4500000000000000111, 0.4625000000000000222, 0.4749999999999999778, 0.4874999999999999889, 0.5000000000000000000, 0.5124999999999999556, 0.5250000000000000222, 0.5374999999999999778, 0.5500000000000000444, 0.5625000000000000000, 0.5749999999999999556, 0.5875000000000000222, 0.5999999999999999778, 0.6125000000000000444, 0.6250000000000000000, 0.6374999999999999556, 0.6500000000000000222, 0.6624999999999999778, 0.6750000000000000444, 0.6875000000000000000, 0.6999999999999999556, 0.7125000000000000222, 0.7249999999999999778, 0.7375000000000000444, 0.7500000000000000000, 0.7624999999999999556, 0.7750000000000000222, 0.7874999999999999778, 0.8000000000000000444, 0.8125000000000000000, 0.8249999999999999556, 0.8375000000000000222, 0.8499999999999999778, 0.8625000000000000444, 0.8750000000000000000, 0.8874999999999999556, 0.9000000000000000222, 0.9124999999999999778, 0.9250000000000000444, 0.9375000000000000000, 0.9499999999999999556, 0.9625000000000000222, 0.9749999999999999778, 0.9875000000000000444, 1.000000000000000000 ),
 .UNSPECIFIED. ) 
 GEOMETRIC_REPRESENTATION_ITEM ( )  RATIONAL_B_SPLINE_SURFACE ( (
 ( 1.000000000000000000, 0.9238795325112869605, 1.000000000000000000, 0.9238795325112869605, 1.000000000000000000, 0.9238795325112869605, 1.000000000000000000, 0.9238795325112869605, 1.000000000000000000, 0.9238795325112869605, 1.000000000000000000, 0.9238795325112869605, 1.000000000000000000, 0.9238795325112869605, 1.000000000000000000, 0.9238795325112869605, 1.000000000000000000, 0.9238795325112869605, 1.000000000000000000, 0.9238795325112869605, 1.000000000000000000, 0.9238795325112869605, 1.000000000000000000, 0.9238795325112869605, 1.000000000000000000, 0.9238795325112869605, 1.000000000000000000, 0.9238795325112869605, 1.000000000000000000, 0.9238795325112869605, 1.000000000000000000, 0.9238795325112869605, 1.000000000000000000, 0.9238795325112869605, 1.000000000000000000, 0.9238795325112869605, 1.000000000000000000, 0.9238795325112869605, 1.000000000000000000, 0.9238795325112869605, 1.000000000000000000, 0.9238795325112869605, 1.000000000000000000, 0.9238795325112869605, 1.000000000000000000, 0.9238795325112869605, 1.000000000000000000, 0.9238795325112869605, 1.000000000000000000, 0.9238795325112869605, 1.000000000000000000, 0.9238795325112869605, 1.000000000000000000, 0.9238795325112869605, 1.000000000000000000, 0.9238795325112869605, 1.000000000000000000, 0.9238795325112869605, 1.000000000000000000, 0.9238795325112869605, 1.000000000000000000, 0.9238795325112869605, 1.000000000000000000, 0.9238795325112869605, 1.000000000000000000, 0.9238795325112869605, 1.000000000000000000, 0.9238795325112869605, 1.000000000000000000, 0.9238795325112869605, 1.000000000000000000, 0.9238795325112869605, 1.000000000000000000, 0.9238795325112869605, 1.000000000000000000, 0.9238795325112869605, 1.000000000000000000, 0.9238795325112869605, 1.000000000000000000, 0.9238795325112869605, 1.000000000000000000, 0.9238795325112869605, 1.000000000000000000, 0.9238795325112869605, 1.000000000000000000, 0.9238795325112869605, 1.000000000000000000, 0.9238795325112869605, 1.000000000000000000, 0.9238795325112869605, 1.000000000000000000, 0.9238795325112869605, 1.000000000000000000, 0.9238795325112869605, 1.000000000000000000, 0.9238795325112869605, 1.000000000000000000, 0.9238795325112869605, 1.000000000000000000, 0.9238795325112869605, 1.000000000000000000, 0.9238795325112869605, 1.000000000000000000, 0.9238795325112869605, 1.000000000000000000, 0.9238795325112869605, 1.000000000000000000, 0.9238795325112869605, 1.000000000000000000, 0.9238795325112869605, 1.000000000000000000, 0.9238795325112869605, 1.000000000000000000, 0.9238795325112869605, 1.000000000000000000, 0.9238795325112869605, 1.000000000000000000, 0.9238795325112869605, 1.000000000000000000, 0.9238795325112869605, 1.000000000000000000, 0.9238795325112869605, 1.000000000000000000, 0.9238795325112869605, 1.000000000000000000, 0.9238795325112869605, 1.000000000000000000, 0.9238795325112869605, 1.000000000000000000, 0.9238795325112869605, 1.000000000000000000, 0.9238795325112869605, 1.000000000000000000, 0.9238795325112869605, 1.000000000000000000, 0.9238795325112869605, 1.000000000000000000, 0.9238795325112869605, 1.000000000000000000, 0.9238795325112869605, 1.000000000000000000, 0.9238795325112869605, 1.000000000000000000, 0.9238795325112869605, 1.000000000000000000, 0.9238795325112869605, 1.000000000000000000, 0.9238795325112869605, 1.000000000000000000, 0.9238795325112869605, 1.000000000000000000, 0.9238795325112869605, 1.000000000000000000, 0.9238795325112869605, 1.000000000000000000, 0.9238795325112869605, 1.000000000000000000, 0.9238795325112869605, 1.000000000000000000, 0.9238795325112869605, 1.000000000000000000),
 ( 1.000000000000000000, 0.9238795325112869605, 1.000000000000000000, 0.9238795325112869605, 1.000000000000000000, 0.9238795325112869605, 1.000000000000000000, 0.9238795325112869605, 1.000000000000000000, 0.9238795325112869605, 1.000000000000000000, 0.9238795325112869605, 1.000000000000000000, 0.9238795325112869605, 1.000000000000000000, 0.9238795325112869605, 1.000000000000000000, 0.9238795325112869605, 1.000000000000000000, 0.9238795325112869605, 1.000000000000000000, 0.9238795325112869605, 1.000000000000000000, 0.9238795325112869605, 1.000000000000000000, 0.9238795325112869605, 1.000000000000000000, 0.9238795325112869605, 1.000000000000000000, 0.9238795325112869605, 1.000000000000000000, 0.9238795325112869605, 1.000000000000000000, 0.9238795325112869605, 1.000000000000000000, 0.9238795325112869605, 1.000000000000000000, 0.9238795325112869605, 1.000000000000000000, 0.9238795325112869605, 1.000000000000000000, 0.9238795325112869605, 1.000000000000000000, 0.9238795325112869605, 1.000000000000000000, 0.9238795325112869605, 1.000000000000000000, 0.9238795325112869605, 1.000000000000000000, 0.9238795325112869605, 1.000000000000000000, 0.9238795325112869605, 1.000000000000000000, 0.9238795325112869605, 1.000000000000000000, 0.9238795325112869605, 1.000000000000000000, 0.9238795325112869605, 1.000000000000000000, 0.9238795325112869605, 1.000000000000000000, 0.9238795325112869605, 1.000000000000000000, 0.9238795325112869605, 1.000000000000000000, 0.9238795325112869605, 1.000000000000000000, 0.9238795325112869605, 1.000000000000000000, 0.9238795325112869605, 1.000000000000000000, 0.9238795325112869605, 1.000000000000000000, 0.9238795325112869605, 1.000000000000000000, 0.9238795325112869605, 1.000000000000000000, 0.9238795325112869605, 1.000000000000000000, 0.9238795325112869605, 1.000000000000000000, 0.9238795325112869605, 1.000000000000000000, 0.9238795325112869605, 1.000000000000000000, 0.9238795325112869605, 1.000000000000000000, 0.9238795325112869605, 1.000000000000000000, 0.9238795325112869605, 1.000000000000000000, 0.9238795325112869605, 1.000000000000000000, 0.9238795325112869605, 1.000000000000000000, 0.9238795325112869605, 1.000000000000000000, 0.9238795325112869605, 1.000000000000000000, 0.9238795325112869605, 1.000000000000000000, 0.9238795325112869605, 1.000000000000000000, 0.9238795325112869605, 1.000000000000000000, 0.9238795325112869605, 1.000000000000000000, 0.9238795325112869605, 1.000000000000000000, 0.9238795325112869605, 1.000000000000000000, 0.9238795325112869605, 1.000000000000000000, 0.9238795325112869605, 1.000000000000000000, 0.9238795325112869605, 1.000000000000000000, 0.9238795325112869605, 1.000000000000000000, 0.9238795325112869605, 1.000000000000000000, 0.9238795325112869605, 1.000000000000000000, 0.9238795325112869605, 1.000000000000000000, 0.9238795325112869605, 1.000000000000000000, 0.9238795325112869605, 1.000000000000000000, 0.9238795325112869605, 1.000000000000000000, 0.9238795325112869605, 1.000000000000000000, 0.9238795325112869605, 1.000000000000000000, 0.9238795325112869605, 1.000000000000000000, 0.9238795325112869605, 1.000000000000000000, 0.9238795325112869605, 1.000000000000000000, 0.9238795325112869605, 1.000000000000000000, 0.9238795325112869605, 1.000000000000000000, 0.9238795325112869605, 1.000000000000000000, 0.9238795325112869605, 1.000000000000000000, 0.9238795325112869605, 1.000000000000000000, 0.9238795325112869605, 1.000000000000000000, 0.9238795325112869605, 1.000000000000000000, 0.9238795325112869605, 1.000000000000000000, 0.9238795325112869605, 1.000000000000000000, 0.9238795325112869605, 1.000000000000000000) ) ) 
 REPRESENTATION_ITEM ( '' )  SURFACE ( )  );
#38935 = CARTESIAN_POINT ( 'NONE',  ( 118.4689281442453250, -10.15424416112533912, -14.75197769757731336 ) ) ;
#38936 = EDGE_CURVE ( 'NONE', #33632, #1444, #13453, .T. ) ;
#38937 = EDGE_CURVE ( 'NONE', #44761, #10907, #41985, .T. ) ;
#38938 = CARTESIAN_POINT ( 'NONE',  ( 121.8618404811916918, -3.807985514183269693, -19.09877912889401230 ) ) ;
#38939 = CARTESIAN_POINT ( 'NONE',  ( 120.2274548109119934, -9.859900752359378018, -12.68260735090039759 ) ) ;
#38940 = VECTOR ( 'NONE', #37819, 1000.000000000000000 ) ;
#38941 = CARTESIAN_POINT ( 'NONE',  ( 128.2184548109119930, -4.863998795839242995, -13.39321520033831447 ) ) ;
#38942 = CARTESIAN_POINT ( 'NONE',  ( 119.4900081442453086, -7.643976991954077427, -18.09477374809248928 ) ) ;
#38943 = CARTESIAN_POINT ( 'NONE',  ( 113.6471614775786492, -5.638512984488999180, -18.83840828888717311 ) ) ;
#38944 = CARTESIAN_POINT ( 'NONE',  ( 118.7525614775786380, -8.166667518702819706, -8.995218007635861213 ) ) ;
#38945 = CARTESIAN_POINT ( 'NONE',  ( 113.3068014775786594, -8.166667518702817929, -8.995218007635859436 ) ) ;
#38946 = FACE_OUTER_BOUND ( 'NONE', #43361, .T. ) ;
#38947 = AXIS2_PLACEMENT_3D ( 'NONE', #16764, #19948, #10369 ) ;
#38948 = CARTESIAN_POINT ( 'NONE',  ( 121.6456214775786293, 0.4262465694468514643, -12.03445270309931736 ) ) ;
#38949 = EDGE_LOOP ( 'NONE', ( #3234, #26791, #20167, #13659 ) ) ;
#38950 = CARTESIAN_POINT ( 'NONE',  ( 115.6325948109119821, 0.2603800115204892296, -16.42320221600525088 ) ) ;
#38951 = CARTESIAN_POINT ( 'NONE',  ( 112.5661608795247872, -1.325403438956436419, -16.93181055722141792 ) ) ;
#38952 = DIRECTION ( 'NONE',  ( 0.9609149988134837450, -0.1028163501681639419, 0.2570431154366518145 ) ) ;
#38953 = CARTESIAN_POINT ( 'NONE',  ( 77.05532149770296257, 0.06670422450934243574, -18.64321520033831803 ) ) ;
#38954 = CARTESIAN_POINT ( 'NONE',  ( 113.4437166496844895, 0.5600166689815611054, -12.14321520033829849 ) ) ;
#38955 = CARTESIAN_POINT ( 'NONE',  ( 125.0492214775786266, -6.344957434206665248, -7.627207830600338134 ) ) ;
#38956 = VERTEX_POINT ( 'NONE', #10918 ) ;
#38957 = CARTESIAN_POINT ( 'NONE',  ( 126.3243314201095160, -8.199742859958636387, -9.597805110430360997 ) ) ;
#38958 = CARTESIAN_POINT ( 'NONE',  ( 121.1918081442452859, -10.15424416112533912, -14.75197769757731336 ) ) ;
#38959 = CARTESIAN_POINT ( 'NONE',  ( -13.32377113153209791, -5.100909530930220370, -18.19321520033831874 ) ) ;
#38960 = CARTESIAN_POINT ( 'NONE',  ( 64.81488287508310009, -15.50725790103587087, -17.58527714782560025 ) ) ;
#38961 = CARTESIAN_POINT ( 'NONE',  ( 120.3506102343419428, -8.309924745830986836, -17.19909913565936321 ) ) ;
#38962 = CARTESIAN_POINT ( 'NONE',  ( 112.4967077545247633, -2.791137627527939813, -18.39754474579286025 ) ) ;
#38963 = ADVANCED_FACE ( 'NONE', ( #10696 ), #18438, .F. ) ;
#38964 = EDGE_LOOP ( 'NONE', ( #15289, #8741 ) ) ;
#38965 = CARTESIAN_POINT ( 'NONE',  ( 115.8027748109119841, -0.4660016031367893996, -10.09054647747474043 ) ) ;
#38966 = CARTESIAN_POINT ( 'NONE',  ( 114.2711548109119803, -9.988377603198976828, -10.36322818467138340 ) ) ;
#38967 = CARTESIAN_POINT ( 'NONE',  ( 88.71490820114844666, -11.16028234076525649, -14.09374590680978123 ) ) ;
#38968 = CARTESIAN_POINT ( 'NONE',  ( 121.7023481442452919, -0.8288870151387760510, -10.36305467784173118 ) ) ;
#38969 = CARTESIAN_POINT ( 'NONE',  ( 86.48169505875749508, -25.99489077589524300, -13.39321520033831625 ) ) ;
#38970 = CARTESIAN_POINT ( 'NONE',  ( 123.5743281442453139, -7.893985811506177619, -18.51759400769804742 ) ) ;
#38971 = CARTESIAN_POINT ( 'NONE',  ( 111.2646414775786496, -8.899110576539710493, -16.42337572283490132 ) ) ;
#38972 = CARTESIAN_POINT ( 'NONE',  ( 118.7315769107182177, -2.467220198592778413, -17.83387418641524391 ) ) ;
#38973 = CARTESIAN_POINT ( 'NONE',  ( 63.69189222814998175, -64.02637234200076932, -46.77412892735921446 ) ) ;
#38974 = ADVANCED_FACE ( 'NONE', ( #7478 ), #471, .T. ) ;
#38975 = DIRECTION ( 'NONE',  ( -0.2768435750659243855, -0.3568721902840678029, 0.8921882507333135370 ) ) ;
#38976 = ORIENTED_EDGE ( 'NONE', *, *, #38644, .F. ) ;
#38977 = EDGE_CURVE ( 'NONE', #22388, #44662, #1185, .T. ) ;
#38978 = AXIS2_PLACEMENT_3D ( 'NONE', #43212, #40238, #22007 ) ;
#38979 = CARTESIAN_POINT ( 'NONE',  ( 115.8304577545247582, -2.791137627527939813, -18.39754474579286025 ) ) ;
#38980 = CARTESIAN_POINT ( 'NONE',  ( 120.6812681442452941, -10.30919188438810075, -12.61870101168855918 ) ) ;
#38981 = CARTESIAN_POINT ( 'NONE',  ( 137.5098831408920717, -8.939295190008330394, -16.29222226817870123 ) ) ;
#38982 = ORIENTED_EDGE ( 'NONE', *, *, #29029, .T. ) ;
#38983 = CARTESIAN_POINT ( 'NONE',  ( 136.9012041053448172, 0.1731349627440442185, -11.10994756160400954 ) ) ;
#38984 = CARTESIAN_POINT ( 'NONE',  ( 124.9924948109119924, -4.089484607189486809, -7.948022111789456723 ) ) ;
#38985 = VECTOR ( 'NONE', #22614, 1000.000000000000114 ) ;
#38986 = DIRECTION ( 'NONE',  ( 0.000000000000000000, 0.6004852223388321697, -0.7996358532186279566 ) ) ;
#38987 = CARTESIAN_POINT ( 'NONE',  ( 123.8579614775786126, -9.859900752359378018, -12.68260735090039759 ) ) ;
#38988 = ORIENTED_EDGE ( 'NONE', *, *, #9323, .T. ) ;
#38989 = CARTESIAN_POINT ( 'NONE',  ( 113.3068014775786594, -8.166667518702817929, -8.995218007635859436 ) ) ;
#38990 = CARTESIAN_POINT ( 'NONE',  ( 85.72471707980444933, -15.28778963902104060, -18.64321520033831803 ) ) ;
#38991 = ADVANCED_FACE ( 'NONE', ( #7709 ), #39792, .T. ) ;
#38992 = DIRECTION ( 'NONE',  ( -0.3127730236694426513, 0.9498278979187093629, 0.000000000000000000 ) ) ;
#38993 = EDGE_CURVE ( 'NONE', #26514, #35134, #37588, .T. ) ;
#38994 = EDGE_CURVE ( 'NONE', #22801, #7584, #1646, .T. ) ;
#38995 = CARTESIAN_POINT ( 'NONE',  ( 135.4522060580519849, -5.622586528377011561, -7.441387646177292758 ) ) ;
#38996 = CARTESIAN_POINT ( 'NONE',  ( 124.2550481442452792, -9.988377603198980381, -10.36322818467138518 ) ) ;
#38997 = CARTESIAN_POINT ( 'NONE',  ( 111.7184548109119788, -8.862178061932382889, -16.39564131203247399 ) ) ;
#38998 = B_SPLINE_CURVE_WITH_KNOTS ( 'NONE', 3,
 ( #8128, #22030, #15869, #15641, #12452, #5372, #19289, #33616, #43233, #5812, #2393, #29545, #16322, #33168, #22251, #32721, #2162, #36146, #26124, #9027, #26578, #23161, #1944, #9253, #5587, #22700, #37042, #19510, #36369, #33388, #16089, #11999, #29994, #43462, #29767, #25902 ),
 .UNSPECIFIED., .F., .F.,
 ( 4, 2, 2, 2, 2, 1, 2, 2, 2, 2, 2, 2, 2, 1, 2, 2, 2, 2, 4 ),
 ( 0.000000000000000000, 0.06250000000003873291, 0.1250000000000774658, 0.1875000000001161848, 0.2187500000001320610, 0.2343750000001399159, 0.2421875000001464662, 0.2500000000001529887, 0.3750000000000988098, 0.5000000000000446310, 0.6249999999999905631, 0.6874999999999634737, 0.7187499999999548139, 0.7343749999999514833, 0.7421874999999552580, 0.7499999999999589217, 0.8124999999999692468, 0.8749999999999795719, 1.000000000000000000 ),
 .UNSPECIFIED. ) ;
#38999 = CARTESIAN_POINT ( 'NONE',  ( 64.69189222814998175, -41.76310523276723785, -6.393215200338315363 ) ) ;
#39000 = CARTESIAN_POINT ( 'NONE',  ( 121.9292548109119849, -1.561330072975668948, -17.79121239304076951 ) ) ;
#39002 = CARTESIAN_POINT ( 'NONE',  ( 124.7088614775786226, -9.565557343593413364, -10.61323700422348004 ) ) ;
#39001 = CARTESIAN_POINT ( 'NONE',  ( 121.0783548109119749, 0.2603800115204892296, -16.42320221600525088 ) ) ;
#39003 = CARTESIAN_POINT ( 'NONE',  ( 116.7565503026016813, -4.863998795840742240, -18.55532337341522364 ) ) ;
#39004 = CARTESIAN_POINT ( 'NONE',  ( 123.6310548109119765, -4.153390946401325223, -8.397313243818185668 ) ) ;
#39005 = CARTESIAN_POINT ( 'NONE',  ( 123.9584548109119737, -4.863998795839242995, -13.39321520033831447 ) ) ;
#39006 = CARTESIAN_POINT ( 'NONE',  ( 121.0783548109119749, 0.2603800115204892296, -16.42320221600525088 ) ) ;
#39007 = VERTEX_POINT ( 'NONE', #42603 ) ;
#39008 = VERTEX_POINT ( 'NONE', #11369 ) ;
#39009 = CARTESIAN_POINT ( 'NONE',  ( 122.4013540574772492, -2.443475742715334853, -17.86549347949429389 ) ) ;
#39010 = CARTESIAN_POINT ( 'NONE',  ( 115.5526452545247622, 0.8980012041604421569, -11.00651665394454071 ) ) ;
#39011 = CIRCLE ( 'NONE', #7696, 0.5000000000000004441 ) ;
#39012 = CARTESIAN_POINT ( 'NONE',  ( 114.4413952545248350, -9.868328341294098749, -15.46607636864997204 ) ) ;
#39013 = CARTESIAN_POINT ( 'NONE',  ( 112.0105358795248804, -8.402594152722688392, -9.854619843455216355 ) ) ;
#39014 = CARTESIAN_POINT ( 'NONE',  ( 126.1837548109119211, -10.63000616557722466, -14.87417383870573495 ) ) ;
#39015 = CARTESIAN_POINT ( 'NONE',  ( 126.6375681442452930, -10.15424416112533912, -14.75197769757731336 ) ) ;
#39016 = EDGE_LOOP ( 'NONE', ( #17905, #27079, #4947, #42085 ) ) ;
#39017 = CARTESIAN_POINT ( 'NONE',  ( 112.2289948109119848, -7.643976991954077427, -18.09477374809248928 ) ) ;
#39018 = CARTESIAN_POINT ( 'NONE',  ( 109.1629577545248395, -7.250697342233347165, -7.631215200338321125 ) ) ;
#39019 = FACE_BOUND ( 'NONE', #9841, .T. ) ;
#39020 = CARTESIAN_POINT ( 'NONE',  ( 125.7299414775786346, 0.9020085738987339008, -11.91225656197089222 ) ) ;
#39022 = AXIS2_PLACEMENT_3D ( 'NONE', #27518, #34553, #17255 ) ;
#39021 = CARTESIAN_POINT ( 'NONE',  ( 65.48165112743716065, -14.20078584921842513, -17.21198551020792067 ) ) ;
#39023 = CARTESIAN_POINT ( 'NONE',  ( 117.8449348109119938, -8.166667518702817929, -8.995218007635861213 ) ) ;
#39024 = CARTESIAN_POINT ( 'NONE',  ( 113.0523327545247838, -2.477300249445798297, -19.15521520033831138 ) ) ;
#39025 = CARTESIAN_POINT ( 'NONE',  ( 109.8574890045248509, -9.868328341294098749, -11.32035403202665869 ) ) ;
#39026 = ORIENTED_EDGE ( 'NONE', *, *, #15579, .F. ) ;
#39027 = DIRECTION ( 'NONE',  ( 0.9609149988134837450, -0.1028163501681639419, 0.2570431154366518145 ) ) ;
#39028 = CARTESIAN_POINT ( 'NONE',  ( 116.7104014775786425, -8.899110576539710493, -16.42337572283490132 ) ) ;
#39029 = CARTESIAN_POINT ( 'NONE',  ( 117.1642148109119859, -9.261995988541697145, -16.69588392320189030 ) ) ;
#39030 = VECTOR ( 'NONE', #35309, 1000.000000000000000 ) ;
#39031 = CARTESIAN_POINT ( 'NONE',  ( 112.7962614775786676, -3.383040157471821630, -19.15922257007629170 ) ) ;
#39032 = CARTESIAN_POINT ( 'NONE',  ( 124.8790414775786246, -8.899110576539710493, -16.42337572283490132 ) ) ;
#39033 = CARTESIAN_POINT ( 'NONE',  ( 120.7947214775786193, -0.8288870151387760510, -10.36305467784173118 ) ) ;
#39034 = CARTESIAN_POINT ( 'NONE',  ( 116.8238548109119819, -5.574606645277164318, -18.38911715685844683 ) ) ;
#39035 = ORIENTED_EDGE ( 'NONE', *, *, #4405, .F. ) ;
#39036 = CARTESIAN_POINT ( 'NONE',  ( 120.5074391859119913, -8.844754642576884152, -8.592115655440050404 ) ) ;
#39037 = CIRCLE ( 'NONE', #43409, 2.445500000000004448 ) ;
#39038 = CARTESIAN_POINT ( 'NONE',  ( 113.2226630180080775, 0.7607806665038616689, -14.64321520033831447 ) ) ;
#39039 = CARTESIAN_POINT ( 'NONE',  ( 116.5402214775786405, -9.565557343593413364, -10.61323700422348004 ) ) ;
#39040 = ORIENTED_EDGE ( 'NONE', *, *, #42868, .T. ) ;
#39041 = CARTESIAN_POINT ( 'NONE',  ( 110.7164878519203768, 0.2518737723193609224, -12.14321520033831625 ) ) ;
#39042 = EDGE_CURVE ( 'NONE', #21831, #35857, #4074, .T. ) ;
#39043 = CARTESIAN_POINT ( 'NONE',  ( 111.9453614775786434, -1.561330072975668060, -17.79121239304076596 ) ) ;
#39044 = CARTESIAN_POINT ( 'NONE',  ( 115.0664733795247798, -8.938348069036489818, -17.46756447353520159 ) ) ;
#39045 = CARTESIAN_POINT ( 'NONE',  ( 113.1366214775786432, -7.643976991954077427, -18.09477374809248928 ) ) ;
#39046 = AXIS2_PLACEMENT_3D ( 'NONE', #42379, #21621, #11143 ) ;
#39047 = ORIENTED_EDGE ( 'NONE', *, *, #32802, .F. ) ;
#39048 = VERTEX_POINT ( 'NONE', #1317 ) ;
#39049 = CARTESIAN_POINT ( 'NONE',  ( 118.6958348109119754, -3.505236298600246325, -18.68346056562440793 ) ) ;
#39050 = CARTESIAN_POINT ( 'NONE',  ( 119.0361948109119652, -2.084020599724406786, -8.691656652584148546 ) ) ;
#39051 = CARTESIAN_POINT ( 'NONE',  ( 124.5497899996740614, -9.862906267826742734, -13.24824213233555170 ) ) ;
#39052 = AXIS2_PLACEMENT_3D ( 'NONE', #41823, #21733, #25386 ) ;
#39053 = CARTESIAN_POINT ( 'NONE',  ( 123.5633766859119760, -0.06289925094097943703, -9.412459353600674206 ) ) ;
#39054 = VERTEX_POINT ( 'NONE', #12043 ) ;
#39055 = DIRECTION ( 'NONE',  ( 1.000000000000000000, 0.000000000000000000, 0.000000000000000000 ) ) ;
#39056 = CARTESIAN_POINT ( 'NONE',  ( 119.7434548109119845, -2.537457910315239040, -8.963164679308437854 ) ) ;
#39057 = CARTESIAN_POINT ( 'NONE',  ( 111.8716296295247901, -4.863998795839590272, -19.15521520033831493 ) ) ;
#39058 = CARTESIAN_POINT ( 'NONE',  ( 113.4769814775786330, -10.63000616557722466, -14.87417383870573495 ) ) ;
#39059 = PRODUCT_DEFINITION_SHAPE ( 'NONE', 'NONE',  #45150 ) ;
#39060 = CARTESIAN_POINT ( 'NONE',  ( 111.8319081442453182, -5.638512984488999180, -18.83840828888717311 ) ) ;
#39061 = EDGE_CURVE ( 'NONE', #19163, #16083, #35966, .T. ) ;
#39062 = CARTESIAN_POINT ( 'NONE',  ( 117.1642148109119859, -0.8288870151387760510, -10.36305467784173118 ) ) ;
#39063 = FACE_OUTER_BOUND ( 'NONE', #36202, .T. ) ;
#39064 = VERTEX_POINT ( 'NONE', #43503 ) ;
#39065 = CARTESIAN_POINT ( 'NONE',  ( 116.8805814775786445, -3.505236298600246325, -18.68346056562440793 ) ) ;
#39066 = CARTESIAN_POINT ( 'NONE',  ( 73.07463722459043254, -56.63952039772598823, -34.96411198583172819 ) ) ;
#39067 = CARTESIAN_POINT ( 'NONE',  ( 84.43379914120473018, -30.20550309442903725, -11.21534971632906519 ) ) ;
#39068 = CARTESIAN_POINT ( 'NONE',  ( 116.3166296295247832, -4.863998795839590272, -19.15521520033831493 ) ) ;
#39069 = AXIS2_PLACEMENT_3D ( 'NONE', #717, #28556, #42461 ) ;
#39070 = CARTESIAN_POINT ( 'NONE',  ( 113.3068014775786594, -8.166667518702817929, -8.995218007635859436 ) ) ;
#39071 = ORIENTED_EDGE ( 'NONE', *, *, #34210, .F. ) ;
#39072 = CARTESIAN_POINT ( 'NONE',  ( 118.2987481442453088, -1.561330072975668504, -17.79121239304076951 ) ) ;
#39073 = CARTESIAN_POINT ( 'NONE',  ( 109.5577383310706807, 0.1843591316377651834, -12.14321520033833757 ) ) ;
#39074 = CARTESIAN_POINT ( 'NONE',  ( 113.8857702545248003, -10.62599879583958717, -15.77991374673208469 ) ) ;
#39075 = CARTESIAN_POINT ( 'NONE',  ( 118.1852948109119836, -5.638512984488999180, -18.83840828888717311 ) ) ;
#39076 = CARTESIAN_POINT ( 'NONE',  ( 114.6682414775786469, -1.561330072975668060, -17.79121239304076596 ) ) ;
#39077 = CARTESIAN_POINT ( 'NONE',  ( 125.7299414775786346, -10.15424416112533912, -14.75197769757731336 ) ) ;
#39078 = CARTESIAN_POINT ( 'NONE',  ( 112.0799890045248759, -9.868328341294150263, -11.32035403202671020 ) ) ;
#39079 = CYLINDRICAL_SURFACE ( 'NONE', #24108, 0.5000000000000039968 ) ;
#39080 = CIRCLE ( 'NONE', #31810, 2.000000000000000444 ) ;
#39081 = ORIENTED_EDGE ( 'NONE', *, *, #9432, .F. ) ;
#39082 = LINE ( 'NONE', #35189, #9929 ) ;
#39083 = CARTESIAN_POINT ( 'NONE',  ( 109.2294364582409116, -3.949221096940591202, -18.45898293540659907 ) ) ;
#39084 = CARTESIAN_POINT ( 'NONE',  ( 115.8027748109119841, -8.899110576539710493, -16.42337572283490132 ) ) ;
#39085 = CARTESIAN_POINT ( 'NONE',  ( 63.90740853991285064, -12.84492318790033138, -10.77114471798664042 ) ) ;
#39086 = CARTESIAN_POINT ( 'NONE',  ( 115.3442858795247759, -8.402594152722688392, -9.854619843455216355 ) ) ;
#39087 = CARTESIAN_POINT ( 'NONE',  ( 106.7320983795247855, -0.7896495226426338832, -9.318865927141430916 ) ) ;
#39088 = CARTESIAN_POINT ( 'NONE',  ( 121.9470836909669913, -25.99489077589524300, -13.39321520033831447 ) ) ;
#39089 = CARTESIAN_POINT ( 'NONE',  ( 114.6115148109119986, -6.222761293078241884, -8.102969835052219238 ) ) ;
#39090 = DIRECTION ( 'NONE',  ( 0.000000000000000000, 0.000000000000000000, 1.000000000000000000 ) ) ;
#39091 = CARTESIAN_POINT ( 'NONE',  ( 123.8012348109119642, 0.2603800115204892296, -16.42320221600525088 ) ) ;
#39092 = CARTESIAN_POINT ( 'NONE',  ( 121.5888948109119809, -10.30919188438810075, -12.61870101168855918 ) ) ;
#39093 = ORIENTED_EDGE ( 'NONE', *, *, #33687, .T. ) ;
#39094 = CARTESIAN_POINT ( 'NONE',  ( 117.2209414775786485, -2.084020599724406786, -8.691656652584148546 ) ) ;
#39095 = DIRECTION ( 'NONE',  ( 0.000000000000000000, -0.3818493186865927203, 0.9242245927363029745 ) ) ;
#39096 = CARTESIAN_POINT ( 'NONE',  ( 118.4122014775786340, 0.5811942927096110934, -14.16772938898807510 ) ) ;
#39097 = CARTESIAN_POINT ( 'NONE',  ( 120.4543614775786295, -5.574606645277164318, -18.38911715685844683 ) ) ;
#39098 = ORIENTED_EDGE ( 'NONE', *, *, #18106, .T. ) ;
#39099 = CARTESIAN_POINT ( 'NONE',  ( 121.9859814775786333, -9.565557343593413364, -10.61323700422348004 ) ) ;
#39100 = CARTESIAN_POINT ( 'NONE',  ( 118.6391081442452986, -4.089484607189486809, -7.948022111789456723 ) ) ;
#39101 = CARTESIAN_POINT ( 'NONE',  ( 136.6523348889540443, 0.4072479916814358836, -15.49606817166481321 ) ) ;
#39102 = AXIS2_PLACEMENT_3D ( 'NONE', #27512, #42089, #27961 ) ;
#39103 = CARTESIAN_POINT ( 'NONE',  ( 108.5378796295247810, -4.863998795839590272, -19.15521520033831493 ) ) ;
#39104 = CARTESIAN_POINT ( 'NONE',  ( 70.36267391504958368, -5.685877709920885259, -4.893215200338314474 ) ) ;
#39105 = CARTESIAN_POINT ( 'NONE',  ( 127.7425183523501744, 0.8652765085452543969, -12.77968882490997338 ) ) ;
#39106 = VECTOR ( 'NONE', #20232, 1000.000000000000000 ) ;
#39107 = CARTESIAN_POINT ( 'NONE',  ( 111.8716296295247901, -4.863998795839590272, -8.388885654883775800 ) ) ;
#39108 = CARTESIAN_POINT ( 'NONE',  ( 114.2711548109119803, -9.988377603198976828, -10.36322818467138340 ) ) ;
#39109 = EDGE_CURVE ( 'NONE', #38271, #43772, #9842, .T. ) ;
#39110 = CARTESIAN_POINT ( 'NONE',  ( 117.2294421295247844, 1.035107641088057973, -5.059859068394715109 ) ) ;
#39111 = CARTESIAN_POINT ( 'NONE',  ( 116.2565881442453133, -0.8288870151387760510, -10.36305467784173118 ) ) ;
#39112 = DIRECTION ( 'NONE',  ( -0.000000000000000000, -0.9284778069183721172, -0.3713878862591650232 ) ) ;
#39113 = DIRECTION ( 'NONE',  ( -1.000000000000000000, 0.000000000000000000, -0.000000000000000000 ) ) ;
#39114 = CARTESIAN_POINT ( 'NONE',  ( 112.2188952545247531, -9.868328341294098749, -15.46607636864997204 ) ) ;
#39115 = MECHANICAL_DESIGN_GEOMETRIC_PRESENTATION_REPRESENTATION (  '', ( #18717 ), #23123 ) ;
#39116 = CARTESIAN_POINT ( 'NONE',  ( 122.1057533359170293, -2.311015703046761072, -18.04188382666269774 ) ) ;
#39117 = DIRECTION ( 'NONE',  ( 0.9609149988134843001, -0.1028163501681632064, 0.2570431154366505933 ) ) ;
#39118 = CARTESIAN_POINT ( 'NONE',  ( 123.9584548109119737, 1.449227268523328505, -18.30678586333412738 ) ) ;
#39120 = CARTESIAN_POINT ( 'NONE',  ( 120.3976348109119812, -1.834011780172310813, -8.268836392978581529 ) ) ;
#39119 = CARTESIAN_POINT ( 'NONE',  ( 65.58071483341541352, -14.25348465845825707, -9.659601953590369661 ) ) ;
#39121 = CARTESIAN_POINT ( 'NONE',  ( 118.1852948109119836, -4.153390946401325223, -8.397313243818185668 ) ) ;
#39122 = CARTESIAN_POINT ( 'NONE',  ( 111.4348214775786801, -3.505236298600246325, -18.68346056562440793 ) ) ;
#39123 = ORIENTED_EDGE ( 'NONE', *, *, #13627, .F. ) ;
#39124 = DIRECTION ( 'NONE',  ( 0.1352586133457950590, 0.9908103287288504424, 0.000000000000000000 ) ) ;
#39125 = CARTESIAN_POINT ( 'NONE',  ( 124.5954081442453116, -3.383040157471821630, -19.15922257007629170 ) ) ;
#39126 = CARTESIAN_POINT ( 'NONE',  ( 114.6497546295247929, -4.863998795839590272, -18.39754474579285315 ) ) ;
#39127 = CARTESIAN_POINT ( 'NONE',  ( 118.9794681442453026, -0.8288870151387760510, -10.36305467784173118 ) ) ;
#39128 = CARTESIAN_POINT ( 'NONE',  ( 116.8805814775786445, -3.505236298600246325, -18.68346056562440793 ) ) ;
#39129 = CARTESIAN_POINT ( 'NONE',  ( 86.22611448523406352, -26.68659777590136528, -8.453450719925958978 ) ) ;
#39130 = CARTESIAN_POINT ( 'NONE',  ( 109.8574890045247940, 0.8980012041604421569, -15.77991374673208469 ) ) ;
#39131 = CARTESIAN_POINT ( 'NONE',  ( 119.0361948109119652, -2.084020599724406786, -8.691656652584148546 ) ) ;
#39132 = CARTESIAN_POINT ( 'NONE',  ( 124.2550481442452792, -0.1624402480850797581, -16.17319339645315424 ) ) ;
#39133 = CARTESIAN_POINT ( 'NONE',  ( 114.2827848082056050, -0.1020945015694959546, -15.74893487844866691 ) ) ;
#39134 = CARTESIAN_POINT ( 'NONE',  ( 109.2294421266624767, -3.229083252145867444, -8.131417123785080747 ) ) ;
#39135 = EDGE_CURVE ( 'NONE', #37731, #17949, #42703, .T. ) ;
#39136 = CARTESIAN_POINT ( 'NONE',  ( 120.7157985609119635, -0.08252387247370887580, -11.91645802438286417 ) ) ;
#39137 = VECTOR ( 'NONE', #24496, 1000.000000000000000 ) ;
#39138 = CARTESIAN_POINT ( 'NONE',  ( 113.3301452545248083, 0.8980012041604421569, -11.00651665394454071 ) ) ;
#39139 = CARTESIAN_POINT ( 'NONE',  ( 69.69189222814998175, -41.76310523276723785, -24.39321520033831447 ) ) ;
#39140 = CARTESIAN_POINT ( 'NONE',  ( 83.36558916507954109, -33.11616680504563703, -22.91154035974133407 ) ) ;
#39141 = CARTESIAN_POINT ( 'NONE',  ( 119.3198281442452924, 0.5811942927096110934, -14.16772938898807510 ) ) ;
#39142 = CARTESIAN_POINT ( 'NONE',  ( 119.4900081442453086, -1.834011780172310813, -8.268836392978581529 ) ) ;
#39143 = CARTESIAN_POINT ( 'NONE',  ( 109.7185827545247889, -2.477300249445798297, -19.15521520033831138 ) ) ;
#39144 = CARTESIAN_POINT ( 'NONE',  ( 112.8529881442453302, -1.561330072975668060, -17.79121239304076596 ) ) ;
#39145 = ORIENTED_EDGE ( 'NONE', *, *, #27338, .F. ) ;
#39146 = CARTESIAN_POINT ( 'NONE',  ( 117.3320321015961412, -1.040089454026966287, -17.23633227186632766 ) ) ;
#39147 = CARTESIAN_POINT ( 'NONE',  ( 115.9729548109119861, -6.344957434206662583, -7.627207830600332805 ) ) ;
#39148 = CARTESIAN_POINT ( 'NONE',  ( 121.9859814775786333, -9.565557343593413364, -10.61323700422348004 ) ) ;
#39149 = PRODUCT_CONTEXT ( 'NONE', #13723, 'mechanical' ) ;
#39150 = CARTESIAN_POINT ( 'NONE',  ( 125.7299414775786346, 0.9020085738987339008, -11.91225656197089222 ) ) ;
#39151 = CARTESIAN_POINT ( 'NONE',  ( 120.6812681442452941, -10.30919188438810075, -12.61870101168855918 ) ) ;
#39152 = VECTOR ( 'NONE', #4458, 1000.000000000000000 ) ;
#39153 = CARTESIAN_POINT ( 'NONE',  ( 115.6220983795247861, -0.7896495226426338832, -9.318865927141430916 ) ) ;
#39154 = CARTESIAN_POINT ( 'NONE',  ( 117.1074881442453233, 0.4262465694468514643, -12.03445270309931736 ) ) ;
#39155 = CARTESIAN_POINT ( 'NONE',  ( 121.6186891859119896, -8.844754642576884152, -8.592115655440050404 ) ) ;
#39156 = CARTESIAN_POINT ( 'NONE',  ( 86.84453910206313765, -17.83168818462593919, -19.39321520033831447 ) ) ;
#39157 = ORIENTED_EDGE ( 'NONE', *, *, #43495, .T. ) ;
#39158 = CARTESIAN_POINT ( 'NONE',  ( 120.5074391859119913, -1.406689858478933353, -17.56299727309130887 ) ) ;
#39159 = CARTESIAN_POINT ( 'NONE',  ( 118.8660148109119774, -10.30919188438810075, -12.61870101168855918 ) ) ;
#39160 = VERTEX_POINT ( 'NONE', #5410 ) ;
#39161 = DIRECTION ( 'NONE',  ( -0.2768435750659241079, -0.3568721902840695792, 0.8921882507333129819 ) ) ;
#39162 = CARTESIAN_POINT ( 'NONE',  ( -13.73225313964263172, -3.820740757134447829, -8.430338879382498263 ) ) ;
#39164 = CARTESIAN_POINT ( 'NONE',  ( 74.66232006577804725, -2.500611837642884527, -16.89321520033831447 ) ) ;
#39163 = VECTOR ( 'NONE', #24995, 1000.000000000000000 ) ;
#39165 = CARTESIAN_POINT ( 'NONE',  ( 117.2209414775786485, -2.084020599724406786, -8.691656652584148546 ) ) ;
#39166 = CARTESIAN_POINT ( 'NONE',  ( 76.69189222814998175, -55.76602098829192755, -2.607500914624014232 ) ) ;
#39167 = CARTESIAN_POINT ( 'NONE',  ( 124.5062240513757246, -9.677281838892072940, -12.03958273341976337 ) ) ;
#39168 = CARTESIAN_POINT ( 'NONE',  ( 120.7379948109119709, 0.4262465694468514643, -12.03445270309931736 ) ) ;
#39169 = DIRECTION ( 'NONE',  ( -1.000000000000000000, 0.000000000000000000, 0.000000000000000000 ) ) ;
#39170 = CARTESIAN_POINT ( 'NONE',  ( 121.0216281442452981, -7.894159318335828068, -9.358103419637847864 ) ) ;
#39171 = CARTESIAN_POINT ( 'NONE',  ( 124.9009360172596530, -12.11729186176019013, -10.90492729001751293 ) ) ;
#39172 = CARTESIAN_POINT ( 'NONE',  ( 122.8368814775786291, -7.894159318335828068, -9.358103419637847864 ) ) ;
#39173 = CARTESIAN_POINT ( 'NONE',  ( 113.5904348109119866, -7.893985811506177619, -18.51759400769804742 ) ) ;
#39174 = CARTESIAN_POINT ( 'NONE',  ( 118.8660148109119774, -10.30919188438810075, -12.61870101168855918 ) ) ;
#39175 = CARTESIAN_POINT ( 'NONE',  ( 125.6732148109119862, -9.859900752359378018, -12.68260735090039759 ) ) ;
#39176 = DIRECTION ( 'NONE',  ( 0.000000000000000000, -0.9242245927363029745, -0.3818493186865929978 ) ) ;
#39177 = CARTESIAN_POINT ( 'NONE',  ( 119.4900081442453086, -7.643976991954077427, -18.09477374809248928 ) ) ;
#39178 = ORIENTED_EDGE ( 'NONE', *, *, #11621, .T. ) ;
#39179 = CARTESIAN_POINT ( 'NONE',  ( 121.9859814775786333, 0.2603800115204892296, -16.42320221600525088 ) ) ;
#39180 = CARTESIAN_POINT ( 'NONE',  ( 112.2188952545247531, -9.868328341294098749, -15.46607636864997204 ) ) ;
#39181 = CARTESIAN_POINT ( 'NONE',  ( 115.7460481442453215, -10.15424416112534267, -14.75197769757730804 ) ) ;
#39182 = CARTESIAN_POINT ( 'NONE',  ( 114.3719421295247827, -9.868328341294093420, -13.39321520033836244 ) ) ;
#39183 = DIRECTION ( 'NONE',  ( -0.000000000000000000, -0.9284778069183718952, -0.3713878862591649677 ) ) ;
#39184 = CARTESIAN_POINT ( 'NONE',  ( 125.6164881442453094, 0.2603800115204892296, -16.42320221600525088 ) ) ;
#39185 = EDGE_LOOP ( 'NONE', ( #42163, #25542, #14833, #26152 ) ) ;
#39186 = FACE_OUTER_BOUND ( 'NONE', #26599, .T. ) ;
#39187 = CARTESIAN_POINT ( 'NONE',  ( 120.1707281442453166, -9.565557343593413364, -10.61323700422348004 ) ) ;
#39188 = CARTESIAN_POINT ( 'NONE',  ( 59.58306117764126952, -13.63527223977064118, -19.38935169184939156 ) ) ;
#39189 = CARTESIAN_POINT ( 'NONE',  ( 75.95778847736481509, -3.256761025687722189, -8.143215200338314474 ) ) ;
#39190 = CARTESIAN_POINT ( 'NONE',  ( 76.19189222814999596, -49.76310523276725206, -29.87698278062875445 ) ) ;
#39191 = CARTESIAN_POINT ( 'NONE',  ( 107.3571765045248299, -2.791137627527939813, -8.388885654883777576 ) ) ;
#39192 = ORIENTED_EDGE ( 'NONE', *, *, #25875, .T. ) ;
#39193 = CARTESIAN_POINT ( 'NONE',  ( 115.3489614775786407, -9.261995988541697145, -16.69588392320189030 ) ) ;
#39194 = CARTESIAN_POINT ( 'NONE',  ( 113.3068014775786594, -8.166667518702817929, -8.995218007635859436 ) ) ;
#39195 = CARTESIAN_POINT ( 'NONE',  ( 88.29631842898217542, -11.60200380960594124, -13.43366796978234845 ) ) ;
#39196 = CARTESIAN_POINT ( 'NONE',  ( 120.7947214775786193, -0.8288870151387760510, -10.36305467784173118 ) ) ;
#39197 = VECTOR ( 'NONE', #215, 1000.000000000000000 ) ;
#39198 = CARTESIAN_POINT ( 'NONE',  ( 127.7429221096697489, -2.658770238890374227, -8.068785233703032134 ) ) ;
#39199 = SURFACE_SIDE_STYLE ('',( #4988 ) ) ;
#39200 = CARTESIAN_POINT ( 'NONE',  ( 122.0994348109119443, 0.9020085738987339008, -11.91225656197089222 ) ) ;
#39201 = CARTESIAN_POINT ( 'NONE',  ( 112.0588148109119828, -9.859900752359374465, -12.68260735090039404 ) ) ;
#39202 = DIRECTION ( 'NONE',  ( -1.000000000000000000, 0.000000000000000000, 0.000000000000000000 ) ) ;
#39203 = DIRECTION ( 'NONE',  ( 1.000000000000000000, 0.000000000000000000, -0.000000000000000000 ) ) ;
#39204 = CARTESIAN_POINT ( 'NONE',  ( 73.60369002873177635, -5.846784287000932778, -18.64321520033831803 ) ) ;
#39205 = ORIENTED_EDGE ( 'NONE', *, *, #26305, .F. ) ;
#39206 = ADVANCED_FACE ( 'NONE', ( #19327 ), #33213, .F. ) ;
#39207 = CARTESIAN_POINT ( 'NONE',  ( 86.34560043013698305, -9.320000780048239619, -18.64321520033831803 ) ) ;
#39208 = CARTESIAN_POINT ( 'NONE',  ( 121.8725281442453223, -3.383040157471821630, -19.15922257007629170 ) ) ;
#39209 = CARTESIAN_POINT ( 'NONE',  ( 137.4282737236245850, -9.220636156388909654, -16.02682550729275235 ) ) ;
#39210 = VERTEX_POINT ( 'NONE', #20237 ) ;
#39211 =( BOUNDED_SURFACE ( )  B_SPLINE_SURFACE ( 1, 2, ( 
 ( #23906, #41898, #37789, #17063, #385, #14297, #17283, #9997, #41458, #17942, #24125, #3364, #38451, #10883, #10661, #20480, #3792, #6794, #7439, #30956, #21360, #24781, #27546, #20703, #41680, #17491, #24565, #34360, #3142, #4020, #28434, #35243, #610, #34581, #14521, #44880, #38018, #13635, #10217, #31174, #10440, #24346, #38231, #31389, #7012, #34796, #159, #14075, #14749, #1282, #1055, #43010, #35930, #4697, #19677, #829, #25238, #39368, #14971, #15194, #25908, #38901, #29099, #32727, #7671 ),
 ( #35473, #9200, #18617, #40439, #36152, #8135, #23109, #4920, #21809, #18835, #1501, #28661, #15421, #28883, #32508, #11328, #36987, #11779, #21586, #11557, #39593, #12005, #39136, #25686, #33565, #16271, #29326, #8354, #5756, #22258, #32291, #43240, #7902, #42347, #25007, #35703, #2342, #4478, #22036, #42566, #18165, #11105, #18398, #42795, #4248, #25464, #32062, #41128, #16953, #9652, #12857, #41574, #23798, #34471, #9888, #24019, #23573, #9419, #37907, #30625, #34690, #37217, #5990, #30175, #3478 ) ),
 .UNSPECIFIED., .F., .F., .F. ) 
 B_SPLINE_SURFACE_WITH_KNOTS ( ( 2, 2 ),
 ( 3, 2, 2, 2, 2, 2, 2, 2, 2, 2, 2, 2, 2, 2, 2, 2, 2, 2, 2, 2, 2, 2, 2, 2, 2, 2, 2, 2, 2, 2, 2, 2, 3 ),
 ( 0.000000000000000000, 1.000000000000000000 ),
 ( 0.000000000000000000, 0.03125000000000000000, 0.06250000000000000000, 0.09375000000000000000, 0.1250000000000000000, 0.1562500000000000000, 0.1875000000000000000, 0.2187500000000000000, 0.2500000000000000000, 0.2812500000000000000, 0.3125000000000000000, 0.3437500000000000000, 0.3750000000000000000, 0.4062500000000000000, 0.4375000000000000000, 0.4687500000000000000, 0.5000000000000000000, 0.5312500000000000000, 0.5625000000000000000, 0.5937500000000000000, 0.6250000000000000000, 0.6562500000000000000, 0.6875000000000000000, 0.7187500000000000000, 0.7500000000000000000, 0.7812500000000000000, 0.8125000000000000000, 0.8437500000000000000, 0.8750000000000000000, 0.9062500000000000000, 0.9375000000000000000, 0.9687500000000000000, 1.000000000000000000 ),
 .UNSPECIFIED. ) 
 GEOMETRIC_REPRESENTATION_ITEM ( )  RATIONAL_B_SPLINE_SURFACE ( (
 ( 1.000000000000000000, 0.9238795325112869605, 1.000000000000000000, 0.9238795325112869605, 1.000000000000000000, 0.9238795325112869605, 1.000000000000000000, 0.9238795325112869605, 1.000000000000000000, 0.9238795325112869605, 1.000000000000000000, 0.9238795325112869605, 1.000000000000000000, 0.9238795325112869605, 1.000000000000000000, 0.9238795325112869605, 1.000000000000000000, 0.9238795325112869605, 1.000000000000000000, 0.9238795325112869605, 1.000000000000000000, 0.9238795325112869605, 1.000000000000000000, 0.9238795325112869605, 1.000000000000000000, 0.9238795325112869605, 1.000000000000000000, 0.9238795325112869605, 1.000000000000000000, 0.9238795325112869605, 1.000000000000000000, 0.9238795325112869605, 1.000000000000000000, 0.9238795325112869605, 1.000000000000000000, 0.9238795325112869605, 1.000000000000000000, 0.9238795325112869605, 1.000000000000000000, 0.9238795325112869605, 1.000000000000000000, 0.9238795325112869605, 1.000000000000000000, 0.9238795325112869605, 1.000000000000000000, 0.9238795325112869605, 1.000000000000000000, 0.9238795325112869605, 1.000000000000000000, 0.9238795325112869605, 1.000000000000000000, 0.9238795325112869605, 1.000000000000000000, 0.9238795325112869605, 1.000000000000000000, 0.9238795325112869605, 1.000000000000000000, 0.9238795325112869605, 1.000000000000000000, 0.9238795325112869605, 1.000000000000000000, 0.9238795325112869605, 1.000000000000000000, 0.9238795325112869605, 1.000000000000000000),
 ( 1.000000000000000000, 0.9238795325112869605, 1.000000000000000000, 0.9238795325112869605, 1.000000000000000000, 0.9238795325112869605, 1.000000000000000000, 0.9238795325112869605, 1.000000000000000000, 0.9238795325112869605, 1.000000000000000000, 0.9238795325112869605, 1.000000000000000000, 0.9238795325112869605, 1.000000000000000000, 0.9238795325112869605, 1.000000000000000000, 0.9238795325112869605, 1.000000000000000000, 0.9238795325112869605, 1.000000000000000000, 0.9238795325112869605, 1.000000000000000000, 0.9238795325112869605, 1.000000000000000000, 0.9238795325112869605, 1.000000000000000000, 0.9238795325112869605, 1.000000000000000000, 0.9238795325112869605, 1.000000000000000000, 0.9238795325112869605, 1.000000000000000000, 0.9238795325112869605, 1.000000000000000000, 0.9238795325112869605, 1.000000000000000000, 0.9238795325112869605, 1.000000000000000000, 0.9238795325112869605, 1.000000000000000000, 0.9238795325112869605, 1.000000000000000000, 0.9238795325112869605, 1.000000000000000000, 0.9238795325112869605, 1.000000000000000000, 0.9238795325112869605, 1.000000000000000000, 0.9238795325112869605, 1.000000000000000000, 0.9238795325112869605, 1.000000000000000000, 0.9238795325112869605, 1.000000000000000000, 0.9238795325112869605, 1.000000000000000000, 0.9238795325112869605, 1.000000000000000000, 0.9238795325112869605, 1.000000000000000000, 0.9238795325112869605, 1.000000000000000000, 0.9238795325112869605, 1.000000000000000000) ) ) 
 REPRESENTATION_ITEM ( '' )  SURFACE ( )  );
#39212 = CARTESIAN_POINT ( 'NONE',  ( 111.8319081442453182, -5.638512984488999180, -18.83840828888717311 ) ) ;
#39213 = B_SPLINE_CURVE_WITH_KNOTS ( 'NONE', 3,
 ( #31992, #7154, #14677, #42273, #10594, #754, #10813, #27700, #24938, #21064 ),
 .UNSPECIFIED., .F., .F.,
 ( 4, 3, 3, 4 ),
 ( 0.000000000000000000, 1.701546542203679946E-05, 3.403093084406070369E-05, 6.582972837196660498E-05 ),
 .UNSPECIFIED. ) ;
#39214 = CARTESIAN_POINT ( 'NONE',  ( 112.6828081442453282, -2.084020599724406786, -8.691656652584148546 ) ) ;
#39215 = CARTESIAN_POINT ( 'NONE',  ( 127.9806007748782690, -4.168156794478616867, -19.23317562329109265 ) ) ;
#39216 = CARTESIAN_POINT ( 'NONE',  ( 123.2906948109119867, -1.833838273342659697, -17.42832698103878286 ) ) ;
#39217 = VERTEX_POINT ( 'NONE', #45076 ) ;
#39218 = CARTESIAN_POINT ( 'NONE',  ( 117.1074881442453233, -10.63000616557722466, -14.87417383870573495 ) ) ;
#39219 = DIRECTION ( 'NONE',  ( 0.000000000000000000, 0.000000000000000000, 1.000000000000000000 ) ) ;
#39220 = LINE ( 'NONE', #38531, #25833 ) ;
#39221 = CARTESIAN_POINT ( 'NONE',  ( 137.2528433483945491, -4.978162001089776467, -8.133589847931153471 ) ) ;
#39222 = CARTESIAN_POINT ( 'NONE',  ( 111.3213681442453264, -7.643976991954077427, -18.09477374809248928 ) ) ;
#39223 = ADVANCED_FACE ( 'NONE', ( #27752 ), #34564, .T. ) ;
#39224 = CARTESIAN_POINT ( 'NONE',  ( 86.48169505875749508, -27.84333996136784961, -14.15691383771150136 ) ) ;
#39225 = DIRECTION ( 'NONE',  ( 0.5040994586965589219, 0.8636456077245088236, 0.000000000000000000 ) ) ;
#39226 = CARTESIAN_POINT ( 'NONE',  ( 121.8158014775786171, -5.638512984488999180, -18.83840828888717311 ) ) ;
#39227 = CARTESIAN_POINT ( 'NONE',  ( 123.1205148109119563, -7.643976991954077427, -18.09477374809248928 ) ) ;
#39228 = CARTESIAN_POINT ( 'NONE',  ( 116.6874845501451574, -8.042305857947342318, -17.38640671321973841 ) ) ;
#39229 = CARTESIAN_POINT ( 'NONE',  ( 124.0281414775786146, -7.643976991954077427, -18.09477374809248928 ) ) ;
#39230 = FACE_OUTER_BOUND ( 'NONE', #2013, .T. ) ;
#39231 = CARTESIAN_POINT ( 'NONE',  ( 119.6034614775786196, -6.344957434206665248, -7.627207830600338134 ) ) ;
#39232 = ADVANCED_FACE ( 'NONE', ( #16823 ), #34124, .T. ) ;
#39233 = ORIENTED_EDGE ( 'NONE', *, *, #36815, .T. ) ;
#39234 = CARTESIAN_POINT ( 'NONE',  ( 126.5041214912249217, -8.563610148337030381, -16.96555754258860205 ) ) ;
#39235 = EDGE_CURVE ( 'NONE', #10734, #35580, #22898, .T. ) ;
#39236 = CARTESIAN_POINT ( 'NONE',  ( 115.6915515045247531, -2.477300249445798297, -7.631215200338321125 ) ) ;
#39237 = CARTESIAN_POINT ( 'NONE',  ( 112.7745202545247878, 0.1403307496149616695, -11.32035403202665336 ) ) ;
#39238 = CARTESIAN_POINT ( 'NONE',  ( 114.9275671295247889, 0.1403307496149613920, -13.39321520033831447 ) ) ;
#39239 = CARTESIAN_POINT ( 'NONE',  ( 125.7866681442453256, -8.899110576539117190, -16.42337572283568647 ) ) ;
#39240 = CARTESIAN_POINT ( 'NONE',  ( 113.7038881442453402, -3.383040157471821630, -19.15922257007629170 ) ) ;
#39241 = ORIENTED_EDGE ( 'NONE', *, *, #2764, .T. ) ;
#39242 = CARTESIAN_POINT ( 'NONE',  ( 113.1933481442453058, -5.574606645277164318, -18.38911715685844683 ) ) ;
#39243 = DIRECTION ( 'NONE',  ( -0.6049664196031347974, 0.7962509850245486076, 0.000000000000000000 ) ) ;
#39244 = DIRECTION ( 'NONE',  ( 0.000000000000000000, 0.000000000000000000, 1.000000000000000000 ) ) ;
#39245 = CARTESIAN_POINT ( 'NONE',  ( 86.48169505875749508, -26.75858941326842810, -11.54476601486570964 ) ) ;
#39246 = CARTESIAN_POINT ( 'NONE',  ( 109.2295375745178490, -0.2444348417507766491, -15.53743370689154091 ) ) ;
#39247 = CARTESIAN_POINT ( 'NONE',  ( 87.44708369096657918, -29.99489077589588959, -12.39321520033834645 ) ) ;
#39248 = CARTESIAN_POINT ( 'NONE',  ( 116.5969481442453031, 0.5811942927096154232, -14.16772938898807155 ) ) ;
#39249 = ADVANCED_FACE ( 'NONE', ( #6320 ), #20463, .F. ) ;
#39250 = CARTESIAN_POINT ( 'NONE',  ( 114.3024890045248156, 0.8980012041604421569, -15.77991374673208469 ) ) ;
#39251 = CARTESIAN_POINT ( 'NONE',  ( 109.4407702545248355, 0.1403307496149616695, -11.32035403202665336 ) ) ;
#39252 = ORIENTED_EDGE ( 'NONE', *, *, #26706, .F. ) ;
#39253 = CARTESIAN_POINT ( 'NONE',  ( 126.2275303246277502, -7.775514682367814956, -9.322671934392364079 ) ) ;
#39254 = CARTESIAN_POINT ( 'NONE',  ( 118.3554748109119998, -9.565557343593413364, -10.61323700422348004 ) ) ;
#39255 = CARTESIAN_POINT ( 'NONE',  ( 115.1220548109119761, -8.166667518702817929, -8.995218007635861213 ) ) ;
#39256 = CARTESIAN_POINT ( 'NONE',  ( 70.19189222814998175, -41.58126682492877535, -29.83537093841426469 ) ) ;
#39257 = EDGE_CURVE ( 'NONE', #38752, #38575, #23035, .T. ) ;
#39258 = CARTESIAN_POINT ( 'NONE',  ( 125.5597614775786326, -7.894159318335828068, -9.358103419637847864 ) ) ;
#39259 = PRODUCT_DEFINITION_CONTEXT ( 'detailed design', #35525, 'design' ) ;
#39260 = CARTESIAN_POINT ( 'NONE',  ( 120.4543614775786295, -5.574606645277164318, -18.38911715685844683 ) ) ;
#39261 = CARTESIAN_POINT ( 'NONE',  ( 117.5613014775786525, -10.15424416112533912, -14.75197769757731336 ) ) ;
#39262 = ORIENTED_EDGE ( 'NONE', *, *, #9786, .F. ) ;
#39263 = ADVANCED_FACE ( 'NONE', ( #13402 ), #38317, .T. ) ;
#39264 = ADVANCED_FACE ( 'NONE', ( #34345 ), #24109, .F. ) ;
#39265 = CARTESIAN_POINT ( 'NONE',  ( 122.6604860609119640, -3.387241619883791355, -18.17469012370385073 ) ) ;
#39266 = AXIS2_PLACEMENT_3D ( 'NONE', #35940, #15658, #11789 ) ;
#39267 = CARTESIAN_POINT ( 'NONE',  ( 121.6508338206745066, -2.348512537728041583, -17.99195118506215962 ) ) ;
#39268 = CARTESIAN_POINT ( 'NONE',  ( 116.2565881442453133, -0.8288870151387760510, -10.36305467784173118 ) ) ;
#39269 = ORIENTED_EDGE ( 'NONE', *, *, #1035, .F. ) ;
#39270 = VECTOR ( 'NONE', #31993, 1000.000000000000227 ) ;
#39271 = CARTESIAN_POINT ( 'NONE',  ( 127.0066334552993084, -9.721555348279057540, -15.73849928315003410 ) ) ;
#39272 = CARTESIAN_POINT ( 'NONE',  ( 116.2565881442452991, -9.261995988541697145, -16.69588392320189030 ) ) ;
#39273 = CARTESIAN_POINT ( 'NONE',  ( 106.1070202545248407, 0.1403307496149616695, -11.32035403202665336 ) ) ;
#39274 = CARTESIAN_POINT ( 'NONE',  ( 112.7395348109119766, -4.153390946401321671, -8.397313243818183892 ) ) ;
#39275 = ORIENTED_EDGE ( 'NONE', *, *, #25596, .T. ) ;
#39276 = ORIENTED_EDGE ( 'NONE', *, *, #15956, .F. ) ;
#39277 = CARTESIAN_POINT ( 'NONE',  ( 122.4965214775786251, 0.1319031606808879209, -14.10382304977623669 ) ) ;
#39278 = CARTESIAN_POINT ( 'NONE',  ( 117.6180281442453150, -8.899110576539710493, -16.42337572283490132 ) ) ;
#39279 = CARTESIAN_POINT ( 'NONE',  ( 124.5716588232362625, -9.842409859139314321, -13.88118749700920418 ) ) ;
#39280 = CARTESIAN_POINT ( 'NONE',  ( 120.6463454359119822, -11.07370829466463569, -12.81314460846529002 ) ) ;
#39281 = ORIENTED_EDGE ( 'NONE', *, *, #12244, .T. ) ;
#39282 = CARTESIAN_POINT ( 'NONE',  ( 112.1243801106810167, -8.918668529216430940, -16.32041580884654053 ) ) ;
#39283 = CARTESIAN_POINT ( 'NONE',  ( 65.19189222814998175, -41.76310523276723785, -20.39321520033831447 ) ) ;
#39284 = CARTESIAN_POINT ( 'NONE',  ( 113.3301452545248083, 0.8980012041604421569, -11.00651665394454071 ) ) ;
#39285 = CARTESIAN_POINT ( 'NONE',  ( 117.1280733121688371, -11.26650585198349752, -21.76132083932495220 ) ) ;
#39286 = CARTESIAN_POINT ( 'NONE',  ( 125.7299414775786346, -10.15424416112533912, -14.75197769757731336 ) ) ;
#39287 = CARTESIAN_POINT ( 'NONE',  ( 121.4754414775786131, -1.833838273342659697, -17.42832698103878286 ) ) ;
#39288 = DIRECTION ( 'NONE',  ( 0.000000000000000000, -0.3818493186865927203, 0.9242245927363029745 ) ) ;
#39289 = EDGE_LOOP ( 'NONE', ( #25146, #22995, #2464, #22586 ) ) ;
#39290 = CARTESIAN_POINT ( 'NONE',  ( 121.4754414775786131, -1.833838273342659697, -17.42832698103878286 ) ) ;
#39291 = EDGE_CURVE ( 'NONE', #6072, #26433, #10404, .T. ) ;
#39292 = CARTESIAN_POINT ( 'NONE',  ( 116.5944421295247793, 0.8980012041604618078, -13.39321520033831447 ) ) ;
#39293 = CARTESIAN_POINT ( 'NONE',  ( 85.45605303719084134, -15.74807682313488222, -16.89321520033831447 ) ) ;
#39294 = CARTESIAN_POINT ( 'NONE',  ( 114.9970202545248412, -10.62599879583958717, -15.77991374673208469 ) ) ;
#39295 = VECTOR ( 'NONE', #4581, 1000.000000000000227 ) ;
#39296 = CARTESIAN_POINT ( 'NONE',  ( 115.9162281442453235, -4.089484607189486809, -7.948022111789456723 ) ) ;
#39297 = ORIENTED_EDGE ( 'NONE', *, *, #11637, .F. ) ;
#39298 = CARTESIAN_POINT ( 'NONE',  ( 118.0151148109119816, -10.63000616557722466, -14.87417383870573495 ) ) ;
#39299 = CARTESIAN_POINT ( 'NONE',  ( 62.66011239371932362, -37.43768621791543438, -5.179380419204645314 ) ) ;
#39300 = CARTESIAN_POINT ( 'NONE',  ( 111.3160046295247838, -4.863998795839590272, -7.631215200338315796 ) ) ;
#39301 = CARTESIAN_POINT ( 'NONE',  ( 116.7671281442453335, -1.834011780172310813, -8.268836392978581529 ) ) ;
#39302 = B_SPLINE_CURVE_WITH_KNOTS ( 'NONE', 3,
 ( #28468, #42375, #11136, #25039, #21616, #4277 ),
 .UNSPECIFIED., .F., .F.,
 ( 4, 2, 4 ),
 ( 0.000000000000000000, 0.5000000000000000000, 1.000000000000000000 ),
 .UNSPECIFIED. ) ;
#39303 = CARTESIAN_POINT ( 'NONE',  ( 118.3554748109119998, 0.2603800115204892296, -16.42320221600525088 ) ) ;
#39304 = CARTESIAN_POINT ( 'NONE',  ( 127.3669547543159979, -10.41873247251588452, -13.86088658824870556 ) ) ;
#39305 = CARTESIAN_POINT ( 'NONE',  ( 61.76166819790555707, -14.46743153019225048, -17.84642471321736679 ) ) ;
#39306 = FACE_OUTER_BOUND ( 'NONE', #36784, .T. ) ;
#39307 = ORIENTED_EDGE ( 'NONE', *, *, #3397, .T. ) ;
#39308 = DIRECTION ( 'NONE',  ( 0.000000000000000000, -0.4669533266896290225, -0.8842819633428516957 ) ) ;
#39309 = AXIS2_PLACEMENT_3D ( 'NONE', #42867, #14828, #42642 ) ;
#39310 = CARTESIAN_POINT ( 'NONE',  ( 109.2294423771211314, -10.02588119094734154, -11.04280315885711516 ) ) ;
#39311 = CARTESIAN_POINT ( 'NONE',  ( 121.5888948109119809, 0.1319031606808879209, -14.10382304977623669 ) ) ;
#39312 = CARTESIAN_POINT ( 'NONE',  ( 65.09033057751396711, -13.38310350479848054, -11.82419014234386268 ) ) ;
#39313 = CARTESIAN_POINT ( 'NONE',  ( 118.1285681442452926, -7.893985811506194494, -18.51759400769804031 ) ) ;
#39314 = CARTESIAN_POINT ( 'NONE',  ( 116.0388171295248014, 0.1403307496149613920, -13.39321520033831447 ) ) ;
#39315 = AXIS2_PLACEMENT_3D ( 'NONE', #5170, #19542, #9286 ) ;
#39316 = CARTESIAN_POINT ( 'NONE',  ( 121.7918886830089775, -1.087735405160626723, -17.17288456429612964 ) ) ;
#39317 = CARTESIAN_POINT ( 'NONE',  ( 112.9097148109120070, -9.565557343593413364, -10.61323700422348004 ) ) ;
#39318 = DIRECTION ( 'NONE',  ( 0.000000000000000000, 0.000000000000000000, 1.000000000000000000 ) ) ;
#39319 = CARTESIAN_POINT ( 'NONE',  ( 122.2696148109119889, -4.089484607189486809, -7.948022111789456723 ) ) ;
#39320 = CARTESIAN_POINT ( 'NONE',  ( 121.0783548109119749, 0.2603800115204892296, -16.42320221600525088 ) ) ;
#39321 = ORIENTED_EDGE ( 'NONE', *, *, #18686, .T. ) ;
#39322 = EDGE_CURVE ( 'NONE', #32138, #17073, #40758, .T. ) ;
#39323 = CARTESIAN_POINT ( 'NONE',  ( 119.9438214775786378, -2.084020599724406786, -8.691656652584148546 ) ) ;
#39324 = CYLINDRICAL_SURFACE ( 'NONE', #23289, 9.999999999999998224 ) ;
#39325 = CARTESIAN_POINT ( 'NONE',  ( 118.2987481442453088, -1.561330072975668504, -17.79121239304076951 ) ) ;
#39326 = CARTESIAN_POINT ( 'NONE',  ( 118.5256548109119876, -8.899110576539710493, -16.42337572283490132 ) ) ;
#39327 = ORIENTED_EDGE ( 'NONE', *, *, #37870, .F. ) ;
#39328 = EDGE_CURVE ( 'NONE', #10907, #44761, #40524, .T. ) ;
#39329 = CARTESIAN_POINT ( 'NONE',  ( 123.1772414775786189, -5.574606645277164318, -18.38911715685844683 ) ) ;
#39330 = CARTESIAN_POINT ( 'NONE',  ( 120.2274548109119934, 0.5811942927096110934, -14.16772938898807510 ) ) ;
#39331 = CIRCLE ( 'NONE', #30611, 0.8509999999999994236 ) ;
#39332 = CARTESIAN_POINT ( 'NONE',  ( 113.0798948109119948, -8.899110576539710493, -16.42337572283490132 ) ) ;
#39333 = CARTESIAN_POINT ( 'NONE',  ( 109.3018640045248304, -10.62599879583958717, -11.00651665394454604 ) ) ;
#39334 = CARTESIAN_POINT ( 'NONE',  ( 114.3077902067644516, -1.223627541775731631, -16.99192386690444323 ) ) ;
#39335 = DIRECTION ( 'NONE',  ( 0.000000000000000000, -0.3818493186865927203, 0.9242245927363029745 ) ) ;
#39336 = CARTESIAN_POINT ( 'NONE',  ( 115.2053796295247849, -4.863998795839590272, -8.388885654883775800 ) ) ;
#39337 = AXIS2_PLACEMENT_3D ( 'NONE', #7014, #30734, #3367 ) ;
#39338 = CARTESIAN_POINT ( 'NONE',  ( 119.0361948109119652, -7.893985811506177619, -18.51759400769804742 ) ) ;
#39339 = AXIS2_PLACEMENT_3D ( 'NONE', #25331, #32377, #7309 ) ;
#39340 = CARTESIAN_POINT ( 'NONE',  ( 137.5098831408899400, -9.795576067877142634, -12.56145304104146021 ) ) ;
#39341 = CARTESIAN_POINT ( 'NONE',  ( 117.2776681442452968, -4.153390946401321671, -8.397313243818183892 ) ) ;
#39342 = CARTESIAN_POINT ( 'NONE',  ( 111.6050014775786536, 0.1319031606808879209, -14.10382304977623669 ) ) ;
#39343 = DIRECTION ( 'NONE',  ( -0.000000000000000000, -0.9284778069183721172, -0.3713878862591650232 ) ) ;
#39344 = CARTESIAN_POINT ( 'NONE',  ( -13.78505786849281911, -3.796669023460694792, -8.893215200338314474 ) ) ;
#39345 = CARTESIAN_POINT ( 'NONE',  ( 110.5520202545248054, 0.1403307496149616695, -11.32035403202665336 ) ) ;
#39346 = CARTESIAN_POINT ( 'NONE',  ( 121.9883441868944658, -2.239543233855044946, -18.13706010537467606 ) ) ;
#39347 = CARTESIAN_POINT ( 'NONE',  ( 113.7414098793805408, -2.191907684172563986, -18.20049396185734025 ) ) ;
#39348 = CARTESIAN_POINT ( 'NONE',  ( 122.9476408503701492, -8.552676153439012552, -17.65880394779906837 ) ) ;
#39350 = CARTESIAN_POINT ( 'NONE',  ( 119.3765548109119834, 0.9020085738987339008, -11.91225656197089222 ) ) ;
#39349 = CARTESIAN_POINT ( 'NONE',  ( 61.95514858534045288, -14.46403247248995427, -7.783443800098010179 ) ) ;
#39351 = CARTESIAN_POINT ( 'NONE',  ( 118.8660148109119774, 0.1319031606808879209, -14.10382304977623669 ) ) ;
#39352 = CARTESIAN_POINT ( 'NONE',  ( 114.3846081442453197, 0.4262465694468514643, -12.03445270309931736 ) ) ;
#39353 = ORIENTED_EDGE ( 'NONE', *, *, #28729, .T. ) ;
#39354 = CARTESIAN_POINT ( 'NONE',  ( 84.77016061404391678, -25.38011337280982715, -14.88121679464376257 ) ) ;
#39355 = CARTESIAN_POINT ( 'NONE',  ( 124.2550481442452792, -9.988377603198980381, -10.36322818467138518 ) ) ;
#39356 = CARTESIAN_POINT ( 'NONE',  ( 114.1635827545248389, -6.936859964151250502, -8.388885654883777576 ) ) ;
#39357 = CARTESIAN_POINT ( 'NONE',  ( 119.9438214775786378, -2.084020599724406786, -8.691656652584148546 ) ) ;
#39358 = EDGE_CURVE ( 'NONE', #25347, #38119, #15748, .T. ) ;
#39359 = CARTESIAN_POINT ( 'NONE',  ( 121.4187148109119789, -3.505236298600246325, -18.68346056562440793 ) ) ;
#39360 = CARTESIAN_POINT ( 'NONE',  ( 118.1285681442453068, -2.084020599724406786, -8.691656652584148546 ) ) ;
#39361 = CARTESIAN_POINT ( 'NONE',  ( 85.26085842212216903, -29.02448141952688232, -9.765951594476932840 ) ) ;
#39362 = CARTESIAN_POINT ( 'NONE',  ( 107.1488171295247867, -10.62599879583958540, -13.39321520033831447 ) ) ;
#39363 = CARTESIAN_POINT ( 'NONE',  ( 124.3117748109119844, 0.1319031606808879209, -14.10382304977623669 ) ) ;
#39364 = CARTESIAN_POINT ( 'NONE',  ( 123.9146881442452894, -10.15424416112533912, -14.75197769757731336 ) ) ;
#39365 = CARTESIAN_POINT ( 'NONE',  ( 115.8523959279789892, 0.1843591316377651834, -14.64321520033831447 ) ) ;
#39366 = AXIS2_PLACEMENT_3D ( 'NONE', #38672, #6562, #27993 ) ;
#39367 = DIRECTION ( 'NONE',  ( 0.000000000000000000, 0.000000000000000000, -1.000000000000000000 ) ) ;
#39368 = CARTESIAN_POINT ( 'NONE',  ( 123.7022829359119811, -4.283928203966213211, -7.183505701512925334 ) ) ;
#39369 = CARTESIAN_POINT ( 'NONE',  ( 115.3442858795247759, -0.7896495226426338832, -17.46756447353520159 ) ) ;
#39370 = CARTESIAN_POINT ( 'NONE',  ( 117.0302221353151424, 1.731593677198245418, -21.24358807290060369 ) ) ;
#39371 = CARTESIAN_POINT ( 'NONE',  ( 116.5944421295247793, 0.8980012041604618078, -13.39321520033831447 ) ) ;
#39372 = CARTESIAN_POINT ( 'NONE',  ( 117.8449348109119938, -8.166667518702817929, -8.995218007635861213 ) ) ;
#39373 = CARTESIAN_POINT ( 'NONE',  ( 119.6601881442453106, -8.166667518702819706, -8.995218007635861213 ) ) ;
#39374 = CARTESIAN_POINT ( 'NONE',  ( 112.9134265045247645, -7.250697342233347165, -19.15521520033831138 ) ) ;
#39375 = CARTESIAN_POINT ( 'NONE',  ( 113.0798948109119948, -0.4660016031367893996, -10.09054647747474043 ) ) ;
#39376 = VERTEX_POINT ( 'NONE', #16593 ) ;
#39377 = CARTESIAN_POINT ( 'NONE',  ( 112.5186459279789801, 0.1843591316377651834, -14.64321520033832691 ) ) ;
#39378 = VECTOR ( 'NONE', #30458, 1000.000000000000000 ) ;
#39379 = CARTESIAN_POINT ( 'NONE',  ( 116.1431348109119881, -10.30919188438810075, -12.61870101168855918 ) ) ;
#39380 = ADVANCED_FACE ( 'NONE', ( #30486 ), #44407, .T. ) ;
#39381 = CARTESIAN_POINT ( 'NONE',  ( 121.3619881442452879, -5.574606645277164318, -18.38911715685844683 ) ) ;
#39382 = AXIS2_PLACEMENT_3D ( 'NONE', #28991, #42898, #11660 ) ;
#39383 = CARTESIAN_POINT ( 'NONE',  ( 115.2355081442453155, 0.1319031606808879209, -14.10382304977623669 ) ) ;
#39384 = CARTESIAN_POINT ( 'NONE',  ( 121.9859814775786333, 0.2603800115204892296, -16.42320221600525088 ) ) ;
#39385 = CARTESIAN_POINT ( 'NONE',  ( 111.8716296295247901, -4.863998795839590272, -19.15521520033831493 ) ) ;
#39386 = CARTESIAN_POINT ( 'NONE',  ( 116.2565881442453133, -0.8288870151387760510, -10.36305467784173118 ) ) ;
#39387 = CARTESIAN_POINT ( 'NONE',  ( 121.3408766859119794, -0.06289925094097943703, -9.412459353600674206 ) ) ;
#39388 = CARTESIAN_POINT ( 'NONE',  ( 94.99177781699742695, -25.99489077589524300, -13.39321520033831447 ) ) ;
#39389 = ORIENTED_EDGE ( 'NONE', *, *, #38650, .T. ) ;
#39390 = CARTESIAN_POINT ( 'NONE',  ( 120.2296266859119953, -9.033780868592240054, -16.85052413769862056 ) ) ;
#39391 = CARTESIAN_POINT ( 'NONE',  ( 120.0572748109119772, -3.383040157471821630, -19.15922257007629170 ) ) ;
#39392 = ORIENTED_EDGE ( 'NONE', *, *, #4513, .F. ) ;
#39393 = CARTESIAN_POINT ( 'NONE',  ( 60.19189222814998175, -75.31442247550837976, -37.94335727672635272 ) ) ;
#39394 = CARTESIAN_POINT ( 'NONE',  ( -13.32377113153209791, -5.100909530930222147, -8.593215200338315540 ) ) ;
#39395 = CIRCLE ( 'NONE', #76, 5.500000000000001776 ) ;
#39396 = CARTESIAN_POINT ( 'NONE',  ( 64.24243542014160369, -41.01918285936451269, -10.39321520033831625 ) ) ;
#39397 = CARTESIAN_POINT ( 'NONE',  ( 114.8384214775786489, -10.15424416112533912, -14.75197769757731336 ) ) ;
#39398 = CARTESIAN_POINT ( 'NONE',  ( 65.72288960572690542, -0.2187004563819841818, -16.39321520033831803 ) ) ;
#39399 = CARTESIAN_POINT ( 'NONE',  ( 64.43740640915127926, -35.20632691772231482, -5.871463680831255694 ) ) ;
#39400 = CARTESIAN_POINT ( 'NONE',  ( 124.9924948109119924, -5.574606645277164318, -18.38911715685844683 ) ) ;
#39401 = LINE ( 'NONE', #8166, #6915 ) ;
#39402 = CARTESIAN_POINT ( 'NONE',  ( 120.5678148109119832, -1.833838273342659253, -17.42832698103878286 ) ) ;
#39403 = VECTOR ( 'NONE', #12641, 1000.000000000000114 ) ;
#39404 = CARTESIAN_POINT ( 'NONE',  ( 117.2294421295247844, 0.6306099254434621715, -14.64321520033831447 ) ) ;
#39405 = CARTESIAN_POINT ( 'NONE',  ( 124.4819548109119722, -2.084020599724406786, -8.691656652584148546 ) ) ;
#39406 = CIRCLE ( 'NONE', #11747, 2.999999999999999556 ) ;
#39407 = CARTESIAN_POINT ( 'NONE',  ( 113.8740681442453138, 0.5811942927096154232, -14.16772938898807155 ) ) ;
#39408 = CARTESIAN_POINT ( 'NONE',  ( 120.2274548109119934, 0.5811942927096110934, -14.16772938898807510 ) ) ;
#39409 = CARTESIAN_POINT ( 'NONE',  ( 113.7038881442453402, -3.383040157471821630, -19.15922257007629170 ) ) ;
#39410 = CARTESIAN_POINT ( 'NONE',  ( 63.69189222814998175, -40.21211973637273474, -6.893215200338315363 ) ) ;
#39411 = CARTESIAN_POINT ( 'NONE',  ( 121.2485348109119769, -8.899110576539710493, -16.42337572283490132 ) ) ;
#39412 = ORIENTED_EDGE ( 'NONE', *, *, #4384, .T. ) ;
#39413 = CARTESIAN_POINT ( 'NONE',  ( 119.6034614775786196, -6.344957434206665248, -7.627207830600338134 ) ) ;
#39414 = CARTESIAN_POINT ( 'NONE',  ( 114.7886608795247696, -1.325403438956436419, -16.93181055722141792 ) ) ;
#39415 = LINE ( 'NONE', #18883, #11737 ) ;
#39416 = CARTESIAN_POINT ( 'NONE',  ( 112.7962614775786676, -6.222761293078241884, -8.102969835052219238 ) ) ;
#39417 = CARTESIAN_POINT ( 'NONE',  ( 137.9323468215654316, -2.878351188643373693, -17.28639180419563104 ) ) ;
#39418 = CARTESIAN_POINT ( 'NONE',  ( 59.75121349346655109, -13.58877957849837692, -7.404803486908546617 ) ) ;
#39419 = ORIENTED_EDGE ( 'NONE', *, *, #29229, .F. ) ;
#39420 = CARTESIAN_POINT ( 'NONE',  ( 120.0572748109119772, -6.222761293078241884, -8.102969835052219238 ) ) ;
#39421 = CARTESIAN_POINT ( 'NONE',  ( 119.9518141859119851, -0.8832429491016019485, -18.19431474523657855 ) ) ;
#39422 = CARTESIAN_POINT ( 'NONE',  ( 62.22090115686911815, -14.48605130139344332, -18.92121278399942952 ) ) ;
#39423 = CARTESIAN_POINT ( 'NONE',  ( 67.84197459855160162, -59.22556289356354142, -37.62220087706567284 ) ) ;
#39424 = CARTESIAN_POINT ( 'NONE',  ( 108.3295202545248657, 0.1403307496149616695, -11.32035403202665336 ) ) ;
#39425 = ORIENTED_EDGE ( 'NONE', *, *, #19177, .F. ) ;
#39426 = CARTESIAN_POINT ( 'NONE',  ( 116.1998614775786507, -10.63000616557722466, -14.87417383870573495 ) ) ;
#39427 = CARTESIAN_POINT ( 'NONE',  ( 125.9001214775786224, -4.089484607189486809, -7.948022111789456723 ) ) ;
#39428 = VECTOR ( 'NONE', #8802, 1000.000000000000000 ) ;
#39429 = CARTESIAN_POINT ( 'NONE',  ( 121.8725281442453223, -6.222761293078241884, -8.102969835052219238 ) ) ;
#39430 = EDGE_CURVE ( 'NONE', #38098, #15917, #18679, .T. ) ;
#39431 = CARTESIAN_POINT ( 'NONE',  ( 112.7395348109119766, -4.153390946401321671, -8.397313243818183892 ) ) ;
#39432 = B_SPLINE_CURVE_WITH_KNOTS ( 'NONE', 3,
 ( #42097, #17261, #31815, #11081, #10861, #24983, #14054, #805, #24756, #35222 ),
 .UNSPECIFIED., .F., .F.,
 ( 4, 3, 3, 4 ),
 ( 0.000000000000000000, 0.0002476486447139030302, 0.0004952972925464440039, 0.0009604418836934600166 ),
 .UNSPECIFIED. ) ;
#39433 = SURFACE_STYLE_USAGE ( .BOTH. , #39199 ) ;
#39434 = CARTESIAN_POINT ( 'NONE',  ( 119.7434548109119703, -8.523281198020143279, -6.279169073056789507 ) ) ;
#39435 = LINE ( 'NONE', #11177, #7005 ) ;
#39436 = CARTESIAN_POINT ( 'NONE',  ( 63.06909581425561129, -64.46843347564573889, -46.33544452488994381 ) ) ;
#39437 = CARTESIAN_POINT ( 'NONE',  ( 111.7184548109119788, -9.261995988541697145, -16.69588392320189030 ) ) ;
#39438 = VERTEX_POINT ( 'NONE', #25219 ) ;
#39439 = CARTESIAN_POINT ( 'NONE',  ( 116.3860827545247787, -6.936859964151250502, -8.388885654883777576 ) ) ;
#39440 = VECTOR ( 'NONE', #9825, 1000.000000000000000 ) ;
#39441 = CARTESIAN_POINT ( 'NONE',  ( 122.2128881442453263, -1.834011780172310813, -8.268836392978581529 ) ) ;
#39442 = DIRECTION ( 'NONE',  ( 0.000000000000000000, 0.000000000000000000, 1.000000000000000000 ) ) ;
#39443 = EDGE_LOOP ( 'NONE', ( #6163, #35495, #44901, #1818 ) ) ;
#39444 = PRODUCT_DEFINITION_SHAPE ( 'NONE', 'NONE',  #45154 ) ;
#39445 = CARTESIAN_POINT ( 'NONE',  ( 136.8340972670101507, 0.2256513543513796738, -11.12430961515349814 ) ) ;
#39446 = CARTESIAN_POINT ( 'NONE',  ( 124.3117748109119844, -10.30919188438810075, -12.61870101168855918 ) ) ;
#39447 = CARTESIAN_POINT ( 'NONE',  ( 123.9584548109119737, -3.874292970208447873, -21.33175929725637587 ) ) ;
#39448 = CARTESIAN_POINT ( 'NONE',  ( 122.5532481442453019, 0.4262465694468514643, -12.03445270309931736 ) ) ;
#39449 = VERTEX_POINT ( 'NONE', #38652 ) ;
#39450 = CARTESIAN_POINT ( 'NONE',  ( 117.9583881442453048, -10.30919188438810075, -12.61870101168855918 ) ) ;
#39451 = DIRECTION ( 'NONE',  ( 1.000000000000000000, 0.000000000000000000, -0.000000000000000000 ) ) ;
#39452 = CARTESIAN_POINT ( 'NONE',  ( 116.5817225628257177, -2.263366209404225504, -18.10533625161308180 ) ) ;
#39453 = CARTESIAN_POINT ( 'NONE',  ( 112.6764896192402432, -1.111561923218668646, -17.14115599315433869 ) ) ;
#39454 = DIRECTION ( 'NONE',  ( 0.7871354856660198740, 0.4483307682966886643, 0.4235767337848242442 ) ) ;
#39455 = CARTESIAN_POINT ( 'NONE',  ( 124.9357681442453014, -1.834011780172310813, -8.268836392978581529 ) ) ;
#39456 = CARTESIAN_POINT ( 'NONE',  ( -12.61278219666105649, -4.053125158562568942, -17.89321520033831447 ) ) ;
#39457 = DIRECTION ( 'NONE',  ( 0.000000000000000000, -0.6004852223388320587, 0.7996358532186281787 ) ) ;
#39458 = CARTESIAN_POINT ( 'NONE',  ( 111.2646414775786496, -8.899110576539710493, -16.42337572283490132 ) ) ;
#39459 = CARTESIAN_POINT ( 'NONE',  ( 125.6732148109119862, -9.859900752359378018, -12.68260735090039759 ) ) ;
#39460 = CARTESIAN_POINT ( 'NONE',  ( 116.6728924761787880, -8.584822191178330897, -16.85008389185930966 ) ) ;
#39461 = CARTESIAN_POINT ( 'NONE',  ( 123.7445081442452874, -7.894159318335828068, -9.358103419637847864 ) ) ;
#39462 = CARTESIAN_POINT ( 'NONE',  ( 112.6828081442453282, -2.084020599724406786, -8.691656652584148546 ) ) ;
#39463 = CARTESIAN_POINT ( 'NONE',  ( 119.8303681442453126, -10.63000616557722466, -14.87417383870573495 ) ) ;
#39464 = EDGE_LOOP ( 'NONE', ( #20942, #40182, #30367, #31086, #8430, #37860 ) ) ;
#39465 = CARTESIAN_POINT ( 'NONE',  ( 127.0400190879709612, -8.468517614608312982, -17.42856087967522782 ) ) ;
#39466 = DIRECTION ( 'NONE',  ( 0.5735764363510499342, 0.3127926500124801890, -0.7570804645221008711 ) ) ;
#39467 = CARTESIAN_POINT ( 'NONE',  ( 110.3436608795247764, -1.325403438956436419, -16.93181055722141792 ) ) ;
#39468 = CARTESIAN_POINT ( 'NONE',  ( 114.5803015045248117, -6.936859964151250502, -18.39754474579286025 ) ) ;
#39469 = CARTESIAN_POINT ( 'NONE',  ( 125.8328548109119964, -8.862178061931794915, -16.39564131203325559 ) ) ;
#39470 = CARTESIAN_POINT ( 'NONE',  ( 114.8384214775786489, 0.9020085738987339008, -11.91225656197089222 ) ) ;
#39471 = ORIENTED_EDGE ( 'NONE', *, *, #17680, .T. ) ;
#39472 = CARTESIAN_POINT ( 'NONE',  ( 116.9940348109119839, -0.1624402480850797581, -16.17319339645315424 ) ) ;
#39473 = CARTESIAN_POINT ( 'NONE',  ( 108.6073327545248048, -2.477300249445798297, -19.15521520033831138 ) ) ;
#39474 = CARTESIAN_POINT ( 'NONE',  ( 135.3184548109119874, -1.889072916127989776, -18.60376373290417362 ) ) ;
#39475 = DIRECTION ( 'NONE',  ( 1.000000000000000000, 0.000000000000000000, -0.000000000000000000 ) ) ;
#39476 = CARTESIAN_POINT ( 'NONE',  ( 109.2295988934735504, -0.1244266206082473986, -15.29196534783836370 ) ) ;
#39477 = CARTESIAN_POINT ( 'NONE',  ( 135.3184548109119874, -4.863998795839242995, -13.39321520033831447 ) ) ;
#39478 = CARTESIAN_POINT ( 'NONE',  ( 116.8805814775786445, -6.344957434206662583, -7.627207830600332805 ) ) ;
#39479 = CARTESIAN_POINT ( 'NONE',  ( 110.5520202545248054, -10.62599879583958717, -15.77991374673208469 ) ) ;
#39480 = CARTESIAN_POINT ( 'NONE',  ( 112.1494421295248003, -9.868328341294093420, -13.39321520033831447 ) ) ;
#39481 = EDGE_LOOP ( 'NONE', ( #28393, #10077 ) ) ;
#39482 = CARTESIAN_POINT ( 'NONE',  ( 127.0066334553006158, -7.209282878650888016, -8.535658647897701456 ) ) ;
#39483 = CARTESIAN_POINT ( 'NONE',  ( 118.1852948109119836, -4.153390946401325223, -8.397313243818185668 ) ) ;
#39484 = CARTESIAN_POINT ( 'NONE',  ( 114.6115148109119986, -3.383040157471821630, -19.15922257007629170 ) ) ;
#39485 = CARTESIAN_POINT ( 'NONE',  ( 112.9097148109120070, 0.2603800115204892296, -16.42320221600525088 ) ) ;
#39486 = CARTESIAN_POINT ( 'NONE',  ( 124.5386814775786206, -4.153390946401325223, -8.397313243818185668 ) ) ;
#39487 = CARTESIAN_POINT ( 'NONE',  ( 124.1983214775786166, -1.833838273342659697, -17.42832698103878286 ) ) ;
#39488 = CARTESIAN_POINT ( 'NONE',  ( 115.8027748109119841, -8.899110576539710493, -16.42337572283490132 ) ) ;
#39489 = VERTEX_POINT ( 'NONE', #3564 ) ;
#39490 = AXIS2_PLACEMENT_3D ( 'NONE', #25353, #35813, #35358 ) ;
#39491 = EDGE_CURVE ( 'NONE', #41326, #44000, #10678, .T. ) ;
#39492 = CARTESIAN_POINT ( 'NONE',  ( 123.6328298109119714, -7.200787124940443817, -17.81845355600750835 ) ) ;
#39493 = VECTOR ( 'NONE', #20697, 1000.000000000000114 ) ;
#39494 = DIRECTION ( 'NONE',  ( 1.000000000000000000, 0.000000000000000000, 0.000000000000000000 ) ) ;
#39495 = CARTESIAN_POINT ( 'NONE',  ( 117.6747548109119919, -7.643976991954077427, -18.09477374809248928 ) ) ;
#39496 = ORIENTED_EDGE ( 'NONE', *, *, #24773, .T. ) ;
#39497 = CARTESIAN_POINT ( 'NONE',  ( 110.5740408578216858, 0.04929351793716424401, -12.14321520033834467 ) ) ;
#39498 = CARTESIAN_POINT ( 'NONE',  ( 114.2144281442453178, -8.166667518702817929, -8.995218007635859436 ) ) ;
#39499 = EDGE_CURVE ( 'NONE', #19198, #13545, #4229, .T. ) ;
#39500 = CARTESIAN_POINT ( 'NONE',  ( 116.5944421295247793, 0.8980012041604618078, -13.39321520033831447 ) ) ;
#39501 = CARTESIAN_POINT ( 'NONE',  ( 112.3424481442453384, -3.505236298600246325, -18.68346056562440793 ) ) ;
#39502 = ORIENTED_EDGE ( 'NONE', *, *, #2511, .T. ) ;
#39503 = AXIS2_PLACEMENT_3D ( 'NONE', #7757, #21665, #18246 ) ;
#39504 = ORIENTED_EDGE ( 'NONE', *, *, #19090, .T. ) ;
#39505 = CARTESIAN_POINT ( 'NONE',  ( 123.9714148109119805, -8.899110576539710493, -16.42337572283490132 ) ) ;
#39506 = CARTESIAN_POINT ( 'NONE',  ( 118.6958348109119754, -3.505236298600246325, -18.68346056562440793 ) ) ;
#39507 = CARTESIAN_POINT ( 'NONE',  ( 124.5900975541519244, -9.759545612246029123, -14.42929304450613159 ) ) ;
#39508 = CARTESIAN_POINT ( 'NONE',  ( 116.5402214775786405, -9.565557343593393824, -10.61323700422345340 ) ) ;
#39509 = ORIENTED_EDGE ( 'NONE', *, *, #16701, .F. ) ;
#39510 = DIRECTION ( 'NONE',  ( -0.5735764363510450492, -0.3127926500124816878, 0.7570804645221038687 ) ) ;
#39511 = CARTESIAN_POINT ( 'NONE',  ( 69.48815586033239811, -68.74046964786722924, -38.06815038123374251 ) ) ;
#39512 = CARTESIAN_POINT ( 'NONE',  ( 112.7745202545247878, -10.62599879583958717, -15.77991374673208469 ) ) ;
#39513 = CARTESIAN_POINT ( 'NONE',  ( 115.6325948109119821, 0.2603800115204892296, -16.42320221600525088 ) ) ;
#39514 = EDGE_CURVE ( 'NONE', #28262, #38150, #14279, .T. ) ;
#39515 = CARTESIAN_POINT ( 'NONE',  ( 126.4673881442452910, -7.894159318335828068, -9.358103419637847864 ) ) ;
#39516 = CARTESIAN_POINT ( 'NONE',  ( 122.2128881442453263, -7.643976991954077427, -18.09477374809248928 ) ) ;
#39517 = DIRECTION ( 'NONE',  ( 1.000000000000000000, 0.000000000000000000, -0.000000000000000000 ) ) ;
#39518 = EDGE_CURVE ( 'NONE', #4027, #2361, #33201, .T. ) ;
#39519 = ADVANCED_FACE ( 'NONE', ( #3775 ), #4460, .T. ) ;
#39520 = EDGE_LOOP ( 'NONE', ( #30111, #34489, #27481, #23228, #2048, #35210, #42354, #20037, #1173, #5880, #11597, #24826 ) ) ;
#39521 = CARTESIAN_POINT ( 'NONE',  ( 121.4187148109119789, -3.505236298600246325, -18.68346056562440793 ) ) ;
#39522 = CIRCLE ( 'NONE', #16229, 2.000000000000000000 ) ;
#39523 = CYLINDRICAL_SURFACE ( 'NONE', #27001, 3.000000000000001776 ) ;
#39524 = AXIS2_PLACEMENT_3D ( 'NONE', #19913, #14126, #31666 ) ;
#39525 = CARTESIAN_POINT ( 'NONE',  ( -1.637506834317598026, -6.775152287193681566, -17.89321520033831447 ) ) ;
#39526 = CARTESIAN_POINT ( 'NONE',  ( 117.2294421295247844, 0.6306099254434621715, -12.14321520033831625 ) ) ;
#39527 = CARTESIAN_POINT ( 'NONE',  ( 118.4122014775786340, 0.5811942927096110934, -14.16772938898807510 ) ) ;
#39528 = B_SPLINE_CURVE_WITH_KNOTS ( 'NONE', 3,
 ( #3337, #44626, #27063, #3111, #13607, #41208, #2884, #23650, #38206, #20676 ),
 .UNSPECIFIED., .F., .F.,
 ( 4, 3, 3, 4 ),
 ( 0.000000000000000000, 0.0002476486447138765215, 0.0004952972925464020452, 0.0009604418836934619681 ),
 .UNSPECIFIED. ) ;
#39529 = ORIENTED_EDGE ( 'NONE', *, *, #31987, .F. ) ;
#39530 = CARTESIAN_POINT ( 'NONE',  ( 117.4478481442453131, 0.2603800115204892296, -16.42320221600525088 ) ) ;
#39531 = CARTESIAN_POINT ( 'NONE',  ( 62.54698291256610787, -37.31319233293334037, -5.252116654659598538 ) ) ;
#39532 = CARTESIAN_POINT ( 'NONE',  ( 108.6767858795247861, -0.7896495226426338832, -17.46756447353520159 ) ) ;
#39533 = CARTESIAN_POINT ( 'NONE',  ( 116.8238548109119819, -4.089484607189486809, -7.948022111789456723 ) ) ;
#39534 = CARTESIAN_POINT ( 'NONE',  ( 118.4689281442453392, 0.9020085738987339008, -11.91225656197089222 ) ) ;
#39535 = FACE_OUTER_BOUND ( 'NONE', #26059, .T. ) ;
#39536 = CARTESIAN_POINT ( 'NONE',  ( 116.2659068881580708, -12.01880880694303855, -6.893215200338315363 ) ) ;
#39537 = CARTESIAN_POINT ( 'NONE',  ( 106.5931921295248372, -9.868328341294093420, -13.39321520033831447 ) ) ;
#39538 = ORIENTED_EDGE ( 'NONE', *, *, #18790, .T. ) ;
#39539 = AXIS2_PLACEMENT_3D ( 'NONE', #6766, #23649, #30476 ) ;
#39540 = CARTESIAN_POINT ( 'NONE',  ( 116.4555358795247884, -0.7896495226426338832, -17.46756447353520159 ) ) ;
#39541 = CARTESIAN_POINT ( 'NONE',  ( 109.2294421560451809, -10.06481071435802832, -15.15239973608284885 ) ) ;
#39542 = CARTESIAN_POINT ( 'NONE',  ( 121.8725281442453223, -6.222761293078241884, -8.102969835052219238 ) ) ;
#39543 = CARTESIAN_POINT ( 'NONE',  ( 111.3160046295247838, -4.863998795839590272, -18.39754474579285315 ) ) ;
#39544 = CARTESIAN_POINT ( 'NONE',  ( 115.4831921295247952, -9.868328341294093420, -13.39321520033831447 ) ) ;
#39545 = CARTESIAN_POINT ( 'NONE',  ( 115.5758681442453053, -7.894159318335828068, -9.358103419637847864 ) ) ;
#39546 = CARTESIAN_POINT ( 'NONE',  ( 82.42994493343583429, -31.76310523276723430, -22.89321520033831803 ) ) ;
#39547 = CARTESIAN_POINT ( 'NONE',  ( 114.0442481442453300, -7.643976991954077427, -18.09477374809248928 ) ) ;
#39548 = CARTESIAN_POINT ( 'NONE',  ( 121.7023481442452777, -9.261995988541697145, -16.69588392320189030 ) ) ;
#39549 = VERTEX_POINT ( 'NONE', #14953 ) ;
#39550 = EDGE_CURVE ( 'NONE', #32144, #40625, #42548, .T. ) ;
#39551 = CARTESIAN_POINT ( 'NONE',  ( 119.8870948109119752, -0.8288870151387760510, -10.36305467784173118 ) ) ;
#39552 = CARTESIAN_POINT ( 'NONE',  ( 113.9875214775786532, -0.4660016031367893996, -10.09054647747474043 ) ) ;
#39553 = CARTESIAN_POINT ( 'NONE',  ( 120.6245414775786458, -9.988377603198976828, -10.36322818467138340 ) ) ;
#39554 = CARTESIAN_POINT ( 'NONE',  ( 118.3554748109119998, -9.565557343593413364, -10.61323700422348004 ) ) ;
#39555 = ORIENTED_EDGE ( 'NONE', *, *, #18308, .T. ) ;
#39556 = DIRECTION ( 'NONE',  ( 0.000000000000000000, 0.000000000000000000, -1.000000000000000000 ) ) ;
#39557 = AXIS2_PLACEMENT_3D ( 'NONE', #41029, #44219, #12980 ) ;
#39558 = EDGE_CURVE ( 'NONE', #21031, #35460, #37014, .T. ) ;
#39559 = CARTESIAN_POINT ( 'NONE',  ( 120.3409081442453044, -0.4660016031367893996, -10.09054647747474043 ) ) ;
#39560 = CARTESIAN_POINT ( 'NONE',  ( 124.3741441133358876, -5.860671235867299877, -5.499845748860171746 ) ) ;
#39561 = FACE_OUTER_BOUND ( 'NONE', #10062, .T. ) ;
#39562 = FACE_OUTER_BOUND ( 'NONE', #4983, .T. ) ;
#39563 = CARTESIAN_POINT ( 'NONE',  ( 112.7745202545247878, 0.1403307496149616695, -11.32035403202665336 ) ) ;
#39564 = AXIS2_PLACEMENT_3D ( 'NONE', #26881, #33703, #15948 ) ;
#39565 = DIRECTION ( 'NONE',  ( 1.000000000000000000, 0.000000000000000000, -0.000000000000000000 ) ) ;
#39566 = CARTESIAN_POINT ( 'NONE',  ( 116.9940348109119839, -0.1624402480850797581, -16.17319339645315424 ) ) ;
#39567 = CARTESIAN_POINT ( 'NONE',  ( 111.2646414775786496, -8.899110576539710493, -16.42337572283490132 ) ) ;
#39568 = DIRECTION ( 'NONE',  ( 0.000000000000000000, -1.000000000000000000, 0.000000000000000000 ) ) ;
#39569 = EDGE_CURVE ( 'NONE', #25709, #22099, #28415, .T. ) ;
#39570 = CARTESIAN_POINT ( 'NONE',  ( 86.34560043013698305, -9.320000780048239619, -8.143215200338314474 ) ) ;
#39571 = CARTESIAN_POINT ( 'NONE',  ( 109.0935046295247872, -4.863998795839590272, -18.39754474579285315 ) ) ;
#39572 = CARTESIAN_POINT ( 'NONE',  ( 113.5337081442453240, -0.8288870151387760510, -10.36305467784173118 ) ) ;
#39573 = DIRECTION ( 'NONE',  ( 0.000000000000000000, 0.000000000000000000, -1.000000000000000000 ) ) ;
#39574 = CARTESIAN_POINT ( 'NONE',  ( -1.667125815598008209, -6.784308745172333843, -18.25434776483827193 ) ) ;
#39576 = CARTESIAN_POINT ( 'NONE',  ( 120.1707281442453166, 0.2603800115204892296, -16.42320221600525088 ) ) ;
#39575 = CARTESIAN_POINT ( 'NONE',  ( 63.19922959105626603, -13.42641530295352403, -8.168935231742574743 ) ) ;
#39577 = CARTESIAN_POINT ( 'NONE',  ( 124.5386814775786206, -4.153390946401325223, -8.397313243818185668 ) ) ;
#39578 = ORIENTED_EDGE ( 'NONE', *, *, #3077, .F. ) ;
#39579 = CARTESIAN_POINT ( 'NONE',  ( 136.7741008876033391, -9.164476617390489466, -9.793428787663129853 ) ) ;
#39580 = ADVANCED_FACE ( 'NONE', ( #35455, #7204 ), #21117, .F. ) ;
#39581 = CARTESIAN_POINT ( 'NONE',  ( 126.2333338125966833, 0.07078918107596827991, -14.24356987566622479 ) ) ;
#39582 = CARTESIAN_POINT ( 'NONE',  ( 109.2324108795247923, -1.325403438956436419, -16.93181055722141792 ) ) ;
#39583 = CARTESIAN_POINT ( 'NONE',  ( 118.8092881442453290, -0.1624402480850797581, -16.17319339645315424 ) ) ;
#39584 = CARTESIAN_POINT ( 'NONE',  ( 122.7234281442452755, -4.153390946401325223, -8.397313243818185668 ) ) ;
#39586 = CARTESIAN_POINT ( 'NONE',  ( 115.1787814775786387, -0.1624402480850797581, -16.17319339645315424 ) ) ;
#39585 = AXIS2_PLACEMENT_3D ( 'NONE', #15203, #22266, #4929 ) ;
#39587 = CARTESIAN_POINT ( 'NONE',  ( 120.8451296192402253, -1.111561923218658210, -17.14115599315433158 ) ) ;
#39588 = CARTESIAN_POINT ( 'NONE',  ( 109.0240515045248202, -2.477300249445798297, -7.631215200338321125 ) ) ;
#39589 = CARTESIAN_POINT ( 'NONE',  ( 123.4041481442452834, 0.1319031606808879209, -14.10382304977623669 ) ) ;
#39590 = CARTESIAN_POINT ( 'NONE',  ( 125.0492214775786266, -3.505236298600246325, -18.68346056562440793 ) ) ;
#39591 = DIRECTION ( 'NONE',  ( 0.000000000000000000, 1.000000000000000000, -1.195183497228115774E-16 ) ) ;
#39592 = CARTESIAN_POINT ( 'NONE',  ( 71.02242295334774269, -99.02728775972636299, -55.91838671430374319 ) ) ;
#39593 = CARTESIAN_POINT ( 'NONE',  ( 120.5768923109119868, -0.4387604401700512802, -15.73000352943951619 ) ) ;
#39594 = CARTESIAN_POINT ( 'NONE',  ( 106.3153796295248412, -4.863998795839590272, -8.388885654883775800 ) ) ;
#39595 = CARTESIAN_POINT ( 'NONE',  ( -13.43397602290982462, -4.955858912465142652, -18.16431974193844923 ) ) ;
#39596 = CARTESIAN_POINT ( 'NONE',  ( 82.53488078675573547, -31.62014037238083830, -22.36964567811433469 ) ) ;
#39597 = CARTESIAN_POINT ( 'NONE',  ( 122.5532481442453019, -10.63000616557722466, -14.87417383870573495 ) ) ;
#39598 = CARTESIAN_POINT ( 'NONE',  ( 116.9940348109119839, -9.988377603198976828, -10.36322818467138340 ) ) ;
#39599 = CARTESIAN_POINT ( 'NONE',  ( 106.1070202545248407, -10.62599879583958717, -15.77991374673208469 ) ) ;
#39600 = CARTESIAN_POINT ( 'NONE',  ( 112.0020881442453344, 0.2603800115204892296, -16.42320221600525088 ) ) ;
#39601 = CARTESIAN_POINT ( 'NONE',  ( 138.2184548109119930, -10.81584935473217080, -14.15181583611863303 ) ) ;
#39602 = EDGE_LOOP ( 'NONE', ( #25027, #15026, #26074, #10238, #1082, #16847 ) ) ;
#39603 = CARTESIAN_POINT ( 'NONE',  ( 70.19189222814998175, -66.16203077818754252, -36.43649583506466882 ) ) ;
#39604 = AXIS2_PLACEMENT_3D ( 'NONE', #5840, #19764, #23417 ) ;
#39605 = CARTESIAN_POINT ( 'NONE',  ( 117.2209414775786485, -7.893985811506177619, -18.51759400769804742 ) ) ;
#39606 = CARTESIAN_POINT ( 'NONE',  ( 124.0848681442452772, -5.574606645277164318, -18.38911715685844683 ) ) ;
#39607 = APPLICATION_PROTOCOL_DEFINITION ( 'draft international standard', 'automotive_design', 1998, #13723 ) ;
#39608 = CARTESIAN_POINT ( 'NONE',  ( 115.3489614775786407, -0.8288870151387760510, -10.36305467784173118 ) ) ;
#39609 = CARTESIAN_POINT ( 'NONE',  ( 120.3976348109119812, -1.834011780172310813, -8.268836392978581529 ) ) ;
#39610 = CARTESIAN_POINT ( 'NONE',  ( 112.2883483795247770, -0.7896495226426338832, -9.318865927141430916 ) ) ;
#39611 = CARTESIAN_POINT ( 'NONE',  ( 118.9794681442453026, -0.8288870151387760510, -10.36305467784173118 ) ) ;
#39612 = CARTESIAN_POINT ( 'NONE',  ( 83.14922721495791791, -33.70571089342944049, -22.39321520033831092 ) ) ;
#39613 = DIRECTION ( 'NONE',  ( 1.000000000000000000, 0.000000000000000000, -0.000000000000000000 ) ) ;
#39614 = ORIENTED_EDGE ( 'NONE', *, *, #27807, .T. ) ;
#39615 = EDGE_CURVE ( 'NONE', #34606, #32113, #36228, .T. ) ;
#39616 = CLOSED_SHELL ( 'NONE', ( #11418, #30216, #29753, #28395, #13390, #33361, #40606, #18054, #8746, #18364, #31034, #7238, #22403, #38991, #21688, #21684, #6823, #30973, #12223, #21703, #10111, #33658, #25048, #21193, #44721, #11021, #19161, #30341, #34204, #42399, #35643, #30327, #17052, #11983, #21259, #12816, #38527, #44438, #51, #9706, #1850, #41229, #42144, #33943, #32307, #43980, #38851, #7755, #43490, #3993, #12417, #6699, #18336, #2446, #14196, #33928, #42850, #2864, #43247, #40962, #33055, #17608, #27948, #36214, #25355, #23981, #26110, #8049, #27114, #239, #8073, #22076, #10851, #15114, #32803, #22519, #31424, #5757, #13805, #2765, #4659, #2731, #10356, #10548, #5204, #21772, #43289, #12933, #1179, #12213, #28452, #8201, #9151, #13127, #1863, #31590, #33686, #10298, #4274, #6358, #8605, #34230, #39807, #18922, #22247, #2930, #13613, #13168, #29846, #35264, #13448, #16993, #6930, #19731 ) ) ;
#39617 = CARTESIAN_POINT ( 'NONE',  ( 122.4521266859119635, -0.06289925094097943703, -9.412459353600674206 ) ) ;
#39618 = CARTESIAN_POINT ( 'NONE',  ( 120.2841814775786276, 0.9020085738987339008, -11.91225656197089222 ) ) ;
#39619 = ORIENTED_EDGE ( 'NONE', *, *, #28009, .F. ) ;
#39620 = CARTESIAN_POINT ( 'NONE',  ( 122.2771248871816141, -6.188980713775695364, -18.62212668298318619 ) ) ;
#39621 = DIRECTION ( 'NONE',  ( 0.000000000000000000, -0.3818493186865927203, 0.9242245927363029745 ) ) ;
#39622 = DIRECTION ( 'NONE',  ( -0.1352586133457952255, -0.9908103287288504424, 0.000000000000000000 ) ) ;
#39623 = CARTESIAN_POINT ( 'NONE',  ( 119.8870948109119752, -0.8288870151387760510, -10.36305467784173118 ) ) ;
#39624 = CARTESIAN_POINT ( 'NONE',  ( 67.12658297191856605, -0.09863003671598137567, -16.39321520033831447 ) ) ;
#39625 = CARTESIAN_POINT ( 'NONE',  ( 124.5059548109119731, -9.675232987814487373, -12.03232374619203249 ) ) ;
#39626 = CARTESIAN_POINT ( 'NONE',  ( 123.8012348109119642, -9.565557343593413364, -10.61323700422348004 ) ) ;
#39627 = CARTESIAN_POINT ( 'NONE',  ( 73.07463722459043254, -51.06865355621575731, -32.73578466827673594 ) ) ;
#39628 = CARTESIAN_POINT ( 'NONE',  ( 123.5743281442453139, -2.084020599724406786, -8.691656652584148546 ) ) ;
#39629 = CARTESIAN_POINT ( 'NONE',  ( 125.3240071284520951, -11.78859274923427947, -15.05733176109422544 ) ) ;
#39630 = EDGE_CURVE ( 'NONE', #31933, #20305, #14730, .T. ) ;
#39631 = CARTESIAN_POINT ( 'NONE',  ( 117.5613014775786525, -10.15424416112533912, -14.75197769757731336 ) ) ;
#39632 = CARTESIAN_POINT ( 'NONE',  ( 123.1772414775786189, -5.574606645277164318, -18.38911715685844683 ) ) ;
#39633 = CARTESIAN_POINT ( 'NONE',  ( 114.6682414775786469, -1.561330072975668060, -17.79121239304076596 ) ) ;
#39634 = CARTESIAN_POINT ( 'NONE',  ( 119.7169148109119874, -9.988377603198976828, -10.36322818467138340 ) ) ;
#39635 = CARTESIAN_POINT ( 'NONE',  ( 114.4980614775786592, -7.893985811506177619, -18.51759400769804742 ) ) ;
#39636 = DIRECTION ( 'NONE',  ( 0.000000000000000000, 0.000000000000000000, -1.000000000000000000 ) ) ;
#39637 = CARTESIAN_POINT ( 'NONE',  ( 123.9146881442452894, -10.15424416112533912, -14.75197769757731336 ) ) ;
#39638 = ORIENTED_EDGE ( 'NONE', *, *, #22472, .T. ) ;
#39639 = CARTESIAN_POINT ( 'NONE',  ( 119.7736414775786358, -10.30919188438810075, -12.61870101168855918 ) ) ;
#39640 = CARTESIAN_POINT ( 'NONE',  ( 113.8163171295247764, -10.62599879583958540, -13.39321520033831447 ) ) ;
#39641 = CARTESIAN_POINT ( 'NONE',  ( 113.7468640045248236, 0.1403307496149616695, -15.46607636864997204 ) ) ;
#39642 = CARTESIAN_POINT ( 'NONE',  ( 138.2184548109119930, -9.067395352211066850, -7.795764227807919333 ) ) ;
#39643 = CIRCLE ( 'NONE', #44772, 5.000000000000000000 ) ;
#39644 = CARTESIAN_POINT ( 'NONE',  ( 112.6260814775786514, -0.8288870151387760510, -10.36305467784173118 ) ) ;
#39645 = CARTESIAN_POINT ( 'NONE',  ( 120.5768923109119868, -9.959231468620755479, -10.70263013195267199 ) ) ;
#39646 = CARTESIAN_POINT ( 'NONE',  ( 125.5597614775786326, -1.561330072975669392, -17.79121239304076951 ) ) ;
#39647 = EDGE_LOOP ( 'NONE', ( #304, #21817, #9719, #42068 ) ) ;
#39648 = CARTESIAN_POINT ( 'NONE',  ( 122.7801548109119665, -6.222761293078241884, -8.102969835052219238 ) ) ;
#39649 = CARTESIAN_POINT ( 'NONE',  ( -13.50731098778515538, -4.859336136776158277, -18.09677371840150784 ) ) ;
#39650 = CARTESIAN_POINT ( 'NONE',  ( 123.3550173109119612, 0.2312338769422704887, -16.08380026872395874 ) ) ;
#39651 = DIRECTION ( 'NONE',  ( -0.000000000000000000, -0.9284778069183718952, -0.3713878862591649677 ) ) ;
#39652 = CARTESIAN_POINT ( 'NONE',  ( 106.1070202545248407, 0.1403307496149616695, -11.32035403202665336 ) ) ;
#39653 = VERTEX_POINT ( 'NONE', #4001 ) ;
#39654 = CARTESIAN_POINT ( 'NONE',  ( 116.4834948109119779, -1.561330072975668504, -17.79121239304076951 ) ) ;
#39655 = DIRECTION ( 'NONE',  ( -0.000000000000000000, -0.9284778069183721172, -0.3713878862591650232 ) ) ;
#39656 = CARTESIAN_POINT ( 'NONE',  ( 119.8870948109119752, -0.8288870151387760510, -10.36305467784173118 ) ) ;
#39657 = DIRECTION ( 'NONE',  ( 0.000000000000000000, -0.5905882410490338463, -0.8069730661766898461 ) ) ;
#39658 =( NAMED_UNIT ( * ) PLANE_ANGLE_UNIT ( ) SI_UNIT ( $, .RADIAN. ) );
#39659 = LINE ( 'NONE', #43531, #41711 ) ;
#39660 = CARTESIAN_POINT ( 'NONE',  ( 114.6881864975817820, -2.215723800389698184, -18.16877924232191788 ) ) ;
#39661 = CARTESIAN_POINT ( 'NONE',  ( 70.19189222814998175, -70.34019061884472990, -41.33884020749756871 ) ) ;
#39662 = VERTEX_POINT ( 'NONE', #39118 ) ;
#39663 = CARTESIAN_POINT ( 'NONE',  ( 114.4413952545248350, -9.868328341294098749, -15.46607636864997204 ) ) ;
#39664 = B_SPLINE_CURVE_WITH_KNOTS ( 'NONE', 3,
 ( #13780, #33831, #37718, #20627, #38160, #20179, #13558, #27916, #41826, #45022 ),
 .UNSPECIFIED., .F., .F.,
 ( 4, 3, 3, 4 ),
 ( 0.000000000000000000, 0.0001671877548681254834, 0.0003343755096277620112, 0.0006463528481650629171 ),
 .UNSPECIFIED. ) ;
#39665 = CARTESIAN_POINT ( 'NONE',  ( 121.7590748109119687, -7.893985811506177619, -18.51759400769804742 ) ) ;
#39666 = CARTESIAN_POINT ( 'NONE',  ( 136.3568202015718782, -10.23338508054624718, -15.60949798484924322 ) ) ;
#39667 = ORIENTED_EDGE ( 'NONE', *, *, #21711, .F. ) ;
#39668 = CARTESIAN_POINT ( 'NONE',  ( 115.6893214775786447, 0.5811942927096154232, -14.16772938898807155 ) ) ;
#39669 = CARTESIAN_POINT ( 'NONE',  ( 111.6617281442453304, 0.4262465694468514643, -12.03445270309931736 ) ) ;
#39670 = DIRECTION ( 'NONE',  ( 0.000000000000000000, 0.000000000000000000, -1.000000000000000000 ) ) ;
#39671 = CARTESIAN_POINT ( 'NONE',  ( 122.6099748109119929, -0.8288870151387760510, -10.36305467784173118 ) ) ;
#39672 = EDGE_LOOP ( 'NONE', ( #3219, #6527, #31032, #17547, #18512 ) ) ;
#39673 = CARTESIAN_POINT ( 'NONE',  ( 119.7169148109119874, -9.988377603198976828, -10.36322818467138340 ) ) ;
#39674 = CARTESIAN_POINT ( 'NONE',  ( 92.26512299712632625, -23.76310523276723785, -20.89321520033831447 ) ) ;
#39675 = CARTESIAN_POINT ( 'NONE',  ( 116.9163235773848726, -2.467220198592778413, -17.83387418641524391 ) ) ;
#39676 = CARTESIAN_POINT ( 'NONE',  ( 124.0578213371693721, -1.204740764657090679, -20.50723739579558824 ) ) ;
#39677 = CARTESIAN_POINT ( 'NONE',  ( 136.3514896075899969, -5.513217599145076697, -7.616394449054343596 ) ) ;
#39678 = AXIS2_PLACEMENT_3D ( 'NONE', #42827, #15226, #35508 ) ;
#39679 = CARTESIAN_POINT ( 'NONE',  ( 114.9518748109119883, -7.643976991954077427, -18.09477374809248928 ) ) ;
#39680 = CARTESIAN_POINT ( 'NONE',  ( 70.19189222814998175, -49.76310523276723785, -36.33917278160906505 ) ) ;
#39681 = EDGE_CURVE ( 'NONE', #10759, #42482, #18044, .T. ) ;
#39682 = CARTESIAN_POINT ( 'NONE',  ( 124.5036465538288581, -3.850231221856767139, -21.22756876946701254 ) ) ;
#39683 = CARTESIAN_POINT ( 'NONE',  ( 113.3635281442453504, -0.1624402480850797581, -16.17319339645315424 ) ) ;
#39684 = CARTESIAN_POINT ( 'NONE',  ( 125.8433948109119456, -7.643976991954077427, -18.09477374809248928 ) ) ;
#39685 = CARTESIAN_POINT ( 'NONE',  ( 120.8547048109119686, -2.527210466738041728, -8.967976844669124148 ) ) ;
#39686 = CARTESIAN_POINT ( 'NONE',  ( 124.1415948109119540, -3.505236298600246325, -18.68346056562440793 ) ) ;
#39687 = CARTESIAN_POINT ( 'NONE',  ( 65.41257106814472877, -15.47412461924279725, -16.39321520033831447 ) ) ;
#39688 = CARTESIAN_POINT ( 'NONE',  ( 119.7736414775786358, -10.30919188438810075, -12.61870101168855918 ) ) ;
#39689 = VERTEX_POINT ( 'NONE', #11087 ) ;
#39690 = CARTESIAN_POINT ( 'NONE',  ( 127.1653849502246629, -8.462563953427153507, -17.51752121746688573 ) ) ;
#39691 = CARTESIAN_POINT ( 'NONE',  ( 114.5803015045248117, -2.477300249445798297, -7.631215200338321125 ) ) ;
#39692 = CARTESIAN_POINT ( 'NONE',  ( 108.6073327545248048, -6.936859964151250502, -8.388885654883777576 ) ) ;
#39693 = CARTESIAN_POINT ( 'NONE',  ( 108.3295202545248657, 0.1403307496149616695, -11.32035403202665336 ) ) ;
#39694 = DIRECTION ( 'NONE',  ( 1.000000000000000000, 0.000000000000000000, -0.000000000000000000 ) ) ;
#39695 = CIRCLE ( 'NONE', #41183, 6.500000000000003553 ) ;
#39696 = CARTESIAN_POINT ( 'NONE',  ( 113.7606148109119886, -1.561330072975668060, -17.79121239304076596 ) ) ;
#39697 = ORIENTED_EDGE ( 'NONE', *, *, #23358, .F. ) ;
#39698 = CARTESIAN_POINT ( 'NONE',  ( 109.3018640045248304, -10.62599879583958717, -11.00651665394454604 ) ) ;
#39699 = DIRECTION ( 'NONE',  ( 0.000000000000000000, 0.000000000000000000, -1.000000000000000000 ) ) ;
#39700 = CARTESIAN_POINT ( 'NONE',  ( 120.2957407289968330, -6.032552146994436981, -18.32589373581284420 ) ) ;
#39701 = CARTESIAN_POINT ( 'NONE',  ( 122.7801548109119665, -6.222761293078217903, -8.102969835052215686 ) ) ;
#39702 = CARTESIAN_POINT ( 'NONE',  ( 112.3991748109119868, -8.166667518702817929, -8.995218007635859436 ) ) ;
#39703 = CARTESIAN_POINT ( 'NONE',  ( 121.0216281442452981, -1.561330072975668948, -17.79121239304076951 ) ) ;
#39704 = CARTESIAN_POINT ( 'NONE',  ( 110.9687390045248350, 0.8980012041604421569, -15.77991374673208469 ) ) ;
#39705 = CARTESIAN_POINT ( 'NONE',  ( 110.8298327545248299, -6.936859964151250502, -8.388885654883777576 ) ) ;
#39706 = AXIS2_PLACEMENT_3D ( 'NONE', #1580, #43322, #25996 ) ;
#39707 = ORIENTED_EDGE ( 'NONE', *, *, #41658, .F. ) ;
#39708 = CARTESIAN_POINT ( 'NONE',  ( 65.82164714941100669, 4.169909004287361221, -19.39321520033831447 ) ) ;
#39709 = CARTESIAN_POINT ( 'NONE',  ( 117.3911214775786505, -7.894159318335828068, -9.358103419637847864 ) ) ;
#39710 = CARTESIAN_POINT ( 'NONE',  ( 117.5045748109119756, 0.5811942927096110934, -14.16772938898807510 ) ) ;
#39711 = CARTESIAN_POINT ( 'NONE',  ( 112.4559014775786494, -9.988377603198976828, -10.36322818467138340 ) ) ;
#39712 = CARTESIAN_POINT ( 'NONE',  ( 124.4819548109119722, -2.084020599724406786, -8.691656652584148546 ) ) ;
#39713 = CARTESIAN_POINT ( 'NONE',  ( 125.1626748109119802, -0.1624402480850797581, -16.17319339645315424 ) ) ;
#39714 = CARTESIAN_POINT ( 'NONE',  ( 116.7671281442453335, -7.643976991954077427, -18.09477374809248928 ) ) ;
#39715 = VERTEX_POINT ( 'NONE', #24988 ) ;
#39716 = CARTESIAN_POINT ( 'NONE',  ( 121.2714235609119697, 0.6414057260225851653, -11.69287257290600657 ) ) ;
#39717 = CARTESIAN_POINT ( 'NONE',  ( 121.6901161498677055, -2.324775150319219108, -18.02356106541841996 ) ) ;
#39718 = CARTESIAN_POINT ( 'NONE',  ( 116.1998614775786507, 0.4262465694468514643, -12.03445270309931736 ) ) ;
#39719 = ORIENTED_EDGE ( 'NONE', *, *, #44253, .F. ) ;
#39720 = CARTESIAN_POINT ( 'NONE',  ( 41.72636039845269096, -11.37347657059392070, -16.39321520033831447 ) ) ;
#39721 = CARTESIAN_POINT ( 'NONE',  ( 113.9307948109119906, 0.9020085738987339008, -11.91225656197089222 ) ) ;
#39722 = CARTESIAN_POINT ( 'NONE',  ( 107.0099108795247815, -1.325403438956436419, -16.93181055722141792 ) ) ;
#39723 = CARTESIAN_POINT ( 'NONE',  ( 125.6164881442453094, -9.565557343593413364, -10.61323700422348004 ) ) ;
#39724 = ORIENTED_EDGE ( 'NONE', *, *, #25630, .T. ) ;
#39725 = EDGE_LOOP ( 'NONE', ( #28536, #20388, #43844, #3708 ) ) ;
#39726 = CARTESIAN_POINT ( 'NONE',  ( 120.6245414775786458, -0.1624402480850797581, -16.17319339645315424 ) ) ;
#39727 = CARTESIAN_POINT ( 'NONE',  ( 116.2565881442453133, -0.8288870151387760510, -10.36305467784173118 ) ) ;
#39728 = ORIENTED_EDGE ( 'NONE', *, *, #24371, .T. ) ;
#39729 = CARTESIAN_POINT ( 'NONE',  ( 83.44708369096697709, -26.60966817898065884, -11.90521360603286816 ) ) ;
#39730 = CARTESIAN_POINT ( 'NONE',  ( 62.15098047326635111, -65.30822568471278089, -44.85084686348432825 ) ) ;
#39731 = CARTESIAN_POINT ( 'NONE',  ( 109.7880358795247986, -0.7896495226426338832, -17.46756447353520159 ) ) ;
#39732 = CARTESIAN_POINT ( 'NONE',  ( 115.4624148109119943, -5.638512984488999180, -18.83840828888717311 ) ) ;
#39734 = CARTESIAN_POINT ( 'NONE',  ( 117.2209414775786485, -2.084020599724406786, -8.691656652584148546 ) ) ;
#39733 = CARTESIAN_POINT ( 'NONE',  ( 114.8951481442453115, -0.4660016031367893996, -10.09054647747474043 ) ) ;
#39735 = CARTESIAN_POINT ( 'NONE',  ( 119.8303681442453126, 0.4262465694468514643, -12.03445270309931736 ) ) ;
#39736 = CARTESIAN_POINT ( 'NONE',  ( 66.06194382436763135, -14.97931106434683635, -4.893215200338314474 ) ) ;
#39737 = ORIENTED_EDGE ( 'NONE', *, *, #2130, .T. ) ;
#39738 = AXIS2_PLACEMENT_3D ( 'NONE', #13105, #37938, #20623 ) ;
#39739 = CARTESIAN_POINT ( 'NONE',  ( 119.0361948109119652, -2.084020599724406786, -8.691656652584148546 ) ) ;
#39740 = CARTESIAN_POINT ( 'NONE',  ( 124.4252281442452812, -0.8288870151387760510, -10.36305467784173118 ) ) ;
#39741 = CARTESIAN_POINT ( 'NONE',  ( 112.4272546295247821, -4.863998795839590272, -7.631215200338315796 ) ) ;
#39742 = CARTESIAN_POINT ( 'NONE',  ( 116.0388171295248014, 0.1403307496149613920, -13.39321520033831447 ) ) ;
#39743 = CARTESIAN_POINT ( 'NONE',  ( 112.3578015045248861, -2.477300249445798297, -7.631215200338321125 ) ) ;
#39744 = VECTOR ( 'NONE', #28731, 1000.000000000000000 ) ;
#39745 = CARTESIAN_POINT ( 'NONE',  ( 118.5256548109119876, -0.4660016031367893996, -10.09054647747474043 ) ) ;
#39746 = ORIENTED_EDGE ( 'NONE', *, *, #23651, .F. ) ;
#39747 = CARTESIAN_POINT ( 'NONE',  ( 122.0994348109119443, 0.9020085738987339008, -11.91225656197089222 ) ) ;
#39748 = CARTESIAN_POINT ( 'NONE',  ( 62.72729074377712521, -37.49987598507249942, -5.141182161264383765 ) ) ;
#39749 = CARTESIAN_POINT ( 'NONE',  ( 108.0517077545248696, -7.250697342233347165, -7.631215200338321125 ) ) ;
#39750 = CARTESIAN_POINT ( 'NONE',  ( 116.1998614775786507, -10.63000616557722466, -14.87417383870573495 ) ) ;
#39751 = CARTESIAN_POINT ( 'NONE',  ( 116.5402214775786405, 0.2603800115204892296, -16.42320221600525088 ) ) ;
#39752 = CARTESIAN_POINT ( 'NONE',  ( 126.4536383592486999, -9.979787239928239018, -13.25019936256093089 ) ) ;
#39753 = CARTESIAN_POINT ( 'NONE',  ( 120.5194882662982963, -6.118135741080345191, -18.48796566952144005 ) ) ;
#39754 = ORIENTED_EDGE ( 'NONE', *, *, #3333, .T. ) ;
#39755 = LINE ( 'NONE', #9421, #36845 ) ;
#39756 = CARTESIAN_POINT ( 'NONE',  ( 109.2294485933674935, -10.43672253586468557, -13.07966451788000128 ) ) ;
#39757 = CARTESIAN_POINT ( 'NONE',  ( 118.8660148109119774, 0.1319031606808879209, -14.10382304977623669 ) ) ;
#39758 = CARTESIAN_POINT ( 'NONE',  ( 113.8857702545248003, 0.1403307496149616695, -11.32035403202665336 ) ) ;
#39759 = CARTESIAN_POINT ( 'NONE',  ( 106.9404577545248145, -7.250697342233347165, -7.631215200338321125 ) ) ;
#39760 = CARTESIAN_POINT ( 'NONE',  ( 115.6893214775786447, -9.859900752359374465, -12.68260735090039404 ) ) ;
#39761 = CARTESIAN_POINT ( 'NONE',  ( 143.3676850761856940, -69.76310523276724496, -16.89321520033831447 ) ) ;
#39762 = CARTESIAN_POINT ( 'NONE',  ( 69.23472380947923455, -25.80888859862148621, -5.871751884747615335 ) ) ;
#39763 = CARTESIAN_POINT ( 'NONE',  ( 113.0798948109119948, -8.899110576539710493, -16.42337572283490132 ) ) ;
#39764 = CARTESIAN_POINT ( 'NONE',  ( 120.7379948109119709, -10.63000616557722466, -14.87417383870573495 ) ) ;
#39765 = VERTEX_POINT ( 'NONE', #38883 ) ;
#39766 = CARTESIAN_POINT ( 'NONE',  ( 117.7882081442453170, -3.505236298600246325, -18.68346056562440793 ) ) ;
#39767 = CARTESIAN_POINT ( 'NONE',  ( 116.2565881442452991, -9.261995988541697145, -16.69588392320189030 ) ) ;
#39768 = CARTESIAN_POINT ( 'NONE',  ( 120.9081748109119872, -5.638512984488999180, -18.83840828888717311 ) ) ;
#39769 = CARTESIAN_POINT ( 'NONE',  ( 119.2063748109119814, -7.894159318335828068, -9.358103419637847864 ) ) ;
#39770 = VERTEX_POINT ( 'NONE', #21568 ) ;
#39771 = CARTESIAN_POINT ( 'NONE',  ( 123.4608748109119745, 0.4262465694468514643, -12.03445270309931736 ) ) ;
#39772 = EDGE_CURVE ( 'NONE', #44361, #9168, #8116, .T. ) ;
#39773 = VECTOR ( 'NONE', #21428, 1000.000000000000000 ) ;
#39774 = CARTESIAN_POINT ( 'NONE',  ( 118.9227414775786400, -10.63000616557722466, -14.87417383870573495 ) ) ;
#39775 = CARTESIAN_POINT ( 'NONE',  ( 112.2857214775786474, -5.574606645277164318, -18.38911715685844683 ) ) ;
#39776 = CARTESIAN_POINT ( 'NONE',  ( 121.9859814775786333, 0.2603800115204892296, -16.42320221600525088 ) ) ;
#39777 = CARTESIAN_POINT ( 'NONE',  ( 105.5513952545248060, 0.8980012041604421569, -11.00651665394454071 ) ) ;
#39778 = DIRECTION ( 'NONE',  ( 1.000000000000000000, 0.000000000000000000, -0.000000000000000000 ) ) ;
#39779 = CARTESIAN_POINT ( 'NONE',  ( 127.9597256070077975, -3.007186152783901445, -14.61697626063841149 ) ) ;
#39780 = CARTESIAN_POINT ( 'NONE',  ( 115.1359265045248605, -2.791137627527939813, -8.388885654883777576 ) ) ;
#39781 = CIRCLE ( 'NONE', #12862, 2.000000000000000444 ) ;
#39782 = LINE ( 'NONE', #40471, #14659 ) ;
#39783 = CARTESIAN_POINT ( 'NONE',  ( 137.3802547664365363, -9.825762579687179255, -12.05248962777355715 ) ) ;
#39784 = CARTESIAN_POINT ( 'NONE',  ( 115.8027748109119841, -8.899110576539710493, -16.42337572283490132 ) ) ;
#39785 = CARTESIAN_POINT ( 'NONE',  ( 125.7866681442452688, -0.4660016031367893996, -10.09054647747474043 ) ) ;
#39786 = CARTESIAN_POINT ( 'NONE',  ( 64.35925685210249014, -13.02253225675024240, -15.66181482168427586 ) ) ;
#39787 = CARTESIAN_POINT ( 'NONE',  ( 112.1234697116520920, -8.918491192341182483, -16.31914947962552631 ) ) ;
#39788 = CARTESIAN_POINT ( 'NONE',  ( 111.5938171295247940, 0.1403307496149613920, -13.39321520033831447 ) ) ;
#39789 = CARTESIAN_POINT ( 'NONE',  ( 116.9940348109119839, -0.1624402480850797581, -16.17319339645315424 ) ) ;
#39790 = CARTESIAN_POINT ( 'NONE',  ( 88.22708560785949317, -3.622631779710408395, -18.64321520033831803 ) ) ;
#39791 = EDGE_CURVE ( 'NONE', #1762, #44794, #4171, .T. ) ;
#39792 = CONICAL_SURFACE ( 'NONE', #21567, 2.000000000000000444, 0.9599310885968830309 ) ;
#39793 = DIRECTION ( 'NONE',  ( -0.8636456077245092677, 0.5040994586965584778, 0.000000000000000000 ) ) ;
#39794 = CARTESIAN_POINT ( 'NONE',  ( -2.049502439613130278, -6.899408072110920997, -18.94416755177243061 ) ) ;
#39796 = CARTESIAN_POINT ( 'NONE',  ( 117.9016614775786280, -9.988377603198976828, -10.36322818467138340 ) ) ;
#39795 = CARTESIAN_POINT ( 'NONE',  ( 62.23965954364707898, -13.31694178448660004, -7.820742382077911614 ) ) ;
#39797 = CARTESIAN_POINT ( 'NONE',  ( 122.4397948109119767, -0.1624402480850797581, -16.17319339645315424 ) ) ;
#39798 = ORIENTED_EDGE ( 'NONE', *, *, #11680, .F. ) ;
#39799 = CARTESIAN_POINT ( 'NONE',  ( 114.7411459279789909, 0.1843591316377651834, -14.64321520033831447 ) ) ;
#39800 = CARTESIAN_POINT ( 'NONE',  ( 124.8223148109119762, 0.9020085738987339008, -11.91225656197089222 ) ) ;
#39801 = CARTESIAN_POINT ( 'NONE',  ( 108.7462390045248242, -9.868328341294098749, -11.32035403202665869 ) ) ;
#39802 = CARTESIAN_POINT ( 'NONE',  ( 123.8012348109119642, -9.565557343593413364, -10.61323700422348004 ) ) ;
#39803 = EDGE_CURVE ( 'NONE', #23418, #28617, #15120, .T. ) ;
#39804 = CARTESIAN_POINT ( 'NONE',  ( 122.2696148109119889, -5.574606645277164318, -18.38911715685844683 ) ) ;
#39805 = AXIS2_PLACEMENT_3D ( 'NONE', #5004, #2031, #15957 ) ;
#39806 = CARTESIAN_POINT ( 'NONE',  ( 115.1220548109119761, -1.833838273342658809, -17.42832698103878286 ) ) ;
#39807 = ADVANCED_FACE ( 'NONE', ( #35911 ), #28241, .T. ) ;
#39808 = CARTESIAN_POINT ( 'NONE',  ( 120.9625387682627746, -1.040089454026966287, -17.23633227186632766 ) ) ;
#39809 = CARTESIAN_POINT ( 'NONE',  ( 109.0935046295247872, -4.863998795839590272, -7.631215200338315796 ) ) ;
#39810 = CARTESIAN_POINT ( 'NONE',  ( 125.4463081442452932, -4.153390946401325223, -8.397313243818185668 ) ) ;
#39811 = CARTESIAN_POINT ( 'NONE',  ( 125.4463081442452932, -4.153390946401325223, -8.397313243818185668 ) ) ;
#39812 = DIRECTION ( 'NONE',  ( 0.9848077530122080203, -0.1736481776669309973, 0.000000000000000000 ) ) ;
#39813 = CARTESIAN_POINT ( 'NONE',  ( 87.44708369096657918, -21.99489077589588604, -18.39321520033831803 ) ) ;
#39814 = CARTESIAN_POINT ( 'NONE',  ( 114.5803015045248117, -2.477300249445798297, -7.631215200338321125 ) ) ;
#39815 = CARTESIAN_POINT ( 'NONE',  ( -13.75549929796900273, -4.532673069121776699, -18.69989194241940922 ) ) ;
#39816 = CARTESIAN_POINT ( 'NONE',  ( 78.69189222814998175, -59.80879295971297438, 0.4535904759388441621 ) ) ;
#39817 = CARTESIAN_POINT ( 'NONE',  ( 122.8368814775786291, -1.561330072975668948, -17.79121239304076951 ) ) ;
#39818 = CARTESIAN_POINT ( 'NONE',  ( 116.7671281442453335, -1.834011780172310813, -8.268836392978581529 ) ) ;
#39819 = CARTESIAN_POINT ( 'NONE',  ( 108.7462390045248242, 0.8980012041604421569, -15.77991374673208469 ) ) ;
#39820 = CARTESIAN_POINT ( 'NONE',  ( 115.9729548109119861, -6.344957434206662583, -7.627207830600332805 ) ) ;
#39821 = DIRECTION ( 'NONE',  ( 0.000000000000000000, -0.3818493186865927203, 0.9242245927363029745 ) ) ;
#39822 = ORIENTED_EDGE ( 'NONE', *, *, #42726, .F. ) ;
#39823 = FACE_OUTER_BOUND ( 'NONE', #5273, .T. ) ;
#39824 = EDGE_CURVE ( 'NONE', #30249, #36383, #22915, .T. ) ;
#39825 = CARTESIAN_POINT ( 'NONE',  ( 119.0361948109119652, -7.893985811506177619, -18.51759400769804742 ) ) ;
#39826 = CARTESIAN_POINT ( 'NONE',  ( 124.3117748109119844, 0.1319031606808879209, -14.10382304977623669 ) ) ;
#39827 = VECTOR ( 'NONE', #36713, 1000.000000000000000 ) ;
#39828 = CARTESIAN_POINT ( 'NONE',  ( 0.000000000000000000, 0.000000000000000000, 0.000000000000000000 ) ) ;
#39829 = EDGE_CURVE ( 'NONE', #25860, #2614, #12585, .T. ) ;
#39830 = CARTESIAN_POINT ( 'NONE',  ( 113.9307948109119764, -10.15424416112533912, -14.75197769757731336 ) ) ;
#39831 = CARTESIAN_POINT ( 'NONE',  ( 124.5386814775786206, -5.638512984488999180, -18.83840828888717311 ) ) ;
#39832 = EDGE_CURVE ( 'NONE', #42647, #4044, #25089, .T. ) ;
#39833 = EDGE_CURVE ( 'NONE', #16121, #18545, #4677, .T. ) ;
#39834 = CIRCLE ( 'NONE', #4106, 4.999999999999998224 ) ;
#39835 = CARTESIAN_POINT ( 'NONE',  ( 107.5655358795247736, -0.7896495226426338832, -17.46756447353520159 ) ) ;
#39836 = CARTESIAN_POINT ( 'NONE',  ( 120.5110881442453206, -3.505236298600246325, -18.68346056562440793 ) ) ;
#39837 = DIRECTION ( 'NONE',  ( -0.000000000000000000, -0.9284778069183721172, -0.3713878862591650232 ) ) ;
#39838 = LINE ( 'NONE', #19314, #38097 ) ;
#39839 = ORIENTED_EDGE ( 'NONE', *, *, #25298, .T. ) ;
#39840 = MECHANICAL_DESIGN_GEOMETRIC_PRESENTATION_REPRESENTATION (  '', ( #7091 ), #3451 ) ;
#39841 = CARTESIAN_POINT ( 'NONE',  ( 94.20708369096698220, -25.17209684859101415, -13.61049647700816401 ) ) ;
#39842 = CARTESIAN_POINT ( 'NONE',  ( 121.2485348109119769, -0.4660016031367893996, -10.09054647747474043 ) ) ;
#39843 = CARTESIAN_POINT ( 'NONE',  ( 125.7299414775786346, -10.15424416112533912, -14.75197769757731336 ) ) ;
#39844 = CARTESIAN_POINT ( 'NONE',  ( 111.3214083975491775, -7.642508564524847614, -18.09498261449271084 ) ) ;
#39845 = SURFACE_SIDE_STYLE ('',( #25937 ) ) ;
#39846 = CARTESIAN_POINT ( 'NONE',  ( 117.9016614775786280, -0.1624402480850797581, -16.17319339645315424 ) ) ;
#39847 = CARTESIAN_POINT ( 'NONE',  ( 85.84150097144041069, -10.18364638777274855, -8.143215200338314474 ) ) ;
#39848 = CARTESIAN_POINT ( 'NONE',  ( 64.28107022230250323, -36.18796843822551779, -5.721420406450495655 ) ) ;
#39849 = CARTESIAN_POINT ( 'NONE',  ( 122.3263414775786373, -3.505236298600246325, -18.68346056562440793 ) ) ;
#39850 = CARTESIAN_POINT ( 'NONE',  ( 121.5492360609119800, -6.564341423271553566, -7.887810678476492754 ) ) ;
#39851 = CARTESIAN_POINT ( 'NONE',  ( 123.6877814775786533, -6.222761293078241884, -8.102969835052219238 ) ) ;
#39852 = CARTESIAN_POINT ( 'NONE',  ( 123.9584548109119737, -11.97804492312075553, -17.05249760251923163 ) ) ;
#39854 = CARTESIAN_POINT ( 'NONE',  ( 124.3117748109119844, -10.30919188438810075, -12.61870101168855918 ) ) ;
#39853 = AXIS2_PLACEMENT_3D ( 'NONE', #24259, #28568, #38811 ) ;
#39855 = CARTESIAN_POINT ( 'NONE',  ( 118.5823814775786360, -7.643976991954077427, -18.09477374809248928 ) ) ;
#39856 = CARTESIAN_POINT ( 'NONE',  ( 124.0848681442452772, -5.574606645277164318, -18.38911715685844683 ) ) ;
#39857 = CARTESIAN_POINT ( 'NONE',  ( 118.0151148109119816, -10.63000616557722466, -14.87417383870573495 ) ) ;
#39858 = CARTESIAN_POINT ( 'NONE',  ( 114.1009748109119784, -4.089484607189486809, -7.948022111789456723 ) ) ;
#39859 = CARTESIAN_POINT ( 'NONE',  ( 113.0523327545247838, -6.936859964151250502, -8.388885654883777576 ) ) ;
#39860 = CARTESIAN_POINT ( 'NONE',  ( 124.4819548109119722, -2.084020599724406786, -8.691656652584148546 ) ) ;
#39861 = ORIENTED_EDGE ( 'NONE', *, *, #8323, .F. ) ;
#39862 = CARTESIAN_POINT ( 'NONE',  ( 121.1918081442452859, 0.9020085738987339008, -11.91225656197089222 ) ) ;
#39863 = CARTESIAN_POINT ( 'NONE',  ( 116.2471765045247594, -7.250697342233347165, -19.15521520033831138 ) ) ;
#39864 = CARTESIAN_POINT ( 'NONE',  ( 108.2600671295247992, 0.1403307496149613920, -13.39321520033831447 ) ) ;
#39865 = CARTESIAN_POINT ( 'NONE',  ( 75.95778847736481509, -3.256761025687722189, -18.64321520033831803 ) ) ;
#39866 = CARTESIAN_POINT ( 'NONE',  ( 46.47434218039879283, -17.93412427487546523, -18.19321520033831519 ) ) ;
#39867 = DIRECTION ( 'NONE',  ( 0.9609149988134837450, -0.1028163501681639419, 0.2570431154366518145 ) ) ;
#39868 = CARTESIAN_POINT ( 'NONE',  ( 116.6638952545248031, -9.868328341294098749, -15.46607636864997204 ) ) ;
#39869 = ORIENTED_EDGE ( 'NONE', *, *, #15015, .F. ) ;
#39870 = CARTESIAN_POINT ( 'NONE',  ( 112.0588148109119828, 0.5811942927096154232, -14.16772938898807155 ) ) ;
#39871 = CARTESIAN_POINT ( 'NONE',  ( 122.1048610609119720, -3.163656168406935087, -18.89861972220014508 ) ) ;
#39872 = CARTESIAN_POINT ( 'NONE',  ( 122.3132204359119868, 1.345710702986147034, -13.97328579221134426 ) ) ;
#39873 = DIRECTION ( 'NONE',  ( -1.000000000000000000, 0.000000000000000000, 0.000000000000000000 ) ) ;
#39874 = CARTESIAN_POINT ( 'NONE',  ( 109.4407702545248355, 0.1403307496149616695, -11.32035403202665336 ) ) ;
#39875 = EDGE_CURVE ( 'NONE', #31353, #32925, #4902, .T. ) ;
#39876 = ORIENTED_EDGE ( 'NONE', *, *, #12758, .T. ) ;
#39877 = CARTESIAN_POINT ( 'NONE',  ( 113.8173414775786512, 0.2603800115204892296, -16.42320221600525088 ) ) ;
#39878 = CARTESIAN_POINT ( 'NONE',  ( 88.88468749803642766, -10.91782331763674385, -14.14321520033831625 ) ) ;
#39879 = CARTESIAN_POINT ( 'NONE',  ( 125.6164881442453094, -9.565557343593413364, -10.61323700422348004 ) ) ;
#39880 = CARTESIAN_POINT ( 'NONE',  ( 114.4413348109119823, -0.8288870151387760510, -10.36305467784173118 ) ) ;
#39881 = SURFACE_STYLE_USAGE ( .BOTH. , #15038 ) ;
#39882 = CARTESIAN_POINT ( 'NONE',  ( 86.34560043013698305, -9.320000780048239619, -9.893215200338316251 ) ) ;
#39883 =( BOUNDED_CURVE ( )  B_SPLINE_CURVE ( 2, ( #16410, #40123, #12767, #26667, #18919, #36239, #33714, #9566, #15501, #15731, #16185, #5005, #9113, #43548, #1579, #22562, #44235 ),
 .UNSPECIFIED., .F., .T. ) 
 B_SPLINE_CURVE_WITH_KNOTS ( ( 3, 2, 2, 2, 2, 2, 2, 2, 3 ),
 ( 0.5040431156034950178, 0.5124999999999999556, 0.5250000000000000222, 0.5374999999999999778, 0.5500000000000000444, 0.5625000000000000000, 0.5749999999999999556, 0.5875000000000000222, 0.5959568843965060703 ),
 .UNSPECIFIED. ) 
 CURVE ( )  GEOMETRIC_REPRESENTATION_ITEM ( )  RATIONAL_B_SPLINE_CURVE ( ( 0.9666851417651740608, 0.9485006404992010198, 1.000000000000000000, 0.9238795325112869605, 1.000000000000000000, 0.9238795325112869605, 1.000000000000000000, 0.9238795325112869605, 1.000000000000000000, 0.9238795325112869605, 1.000000000000000000, 0.9238795325112869605, 1.000000000000000000, 0.9238795325112869605, 1.000000000000000000, 0.9485006404991980222, 0.9666851417651760592 ) ) 
 REPRESENTATION_ITEM ( '' )  );
#39884 = CARTESIAN_POINT ( 'NONE',  ( 124.4252281442452812, -9.261995988541709579, -16.69588392320187253 ) ) ;
#39885 = CARTESIAN_POINT ( 'NONE',  ( 115.5758681442453053, -1.561330072975668060, -17.79121239304076951 ) ) ;
#39886 = CARTESIAN_POINT ( 'NONE',  ( 109.7880358795247986, -8.402594152722688392, -9.854619843455216355 ) ) ;
#39887 = AXIS2_PLACEMENT_3D ( 'NONE', #31090, #38153, #20832 ) ;
#39888 = CARTESIAN_POINT ( 'NONE',  ( 123.4608748109119745, -10.63000616557722466, -14.87417383870573495 ) ) ;
#39889 = CARTESIAN_POINT ( 'NONE',  ( 136.7036351579049267, -10.04987633766737076, -15.63786568088821483 ) ) ;
#39890 = VERTEX_POINT ( 'NONE', #42992 ) ;
#39891 = EDGE_CURVE ( 'NONE', #40192, #4744, #3828, .T. ) ;
#39892 = CARTESIAN_POINT ( 'NONE',  ( 113.9307948109119906, 0.9020085738987339008, -11.91225656197089222 ) ) ;
#39893 = CARTESIAN_POINT ( 'NONE',  ( 125.6732148109119862, 0.5811942927096110934, -14.16772938898807510 ) ) ;
#39894 = CARTESIAN_POINT ( 'NONE',  ( 111.1076452545248259, -9.868328341294102302, -15.46607636865001645 ) ) ;
#39895 = CARTESIAN_POINT ( 'NONE',  ( 126.5241148109119393, -9.565557343593413364, -10.61323700422348004 ) ) ;
#39896 = ORIENTED_EDGE ( 'NONE', *, *, #13019, .T. ) ;
#39897 = CARTESIAN_POINT ( 'NONE',  ( 119.4332814775786318, -0.4660016031367893996, -10.09054647747474043 ) ) ;
#39898 = DIRECTION ( 'NONE',  ( 0.000000000000000000, 0.000000000000000000, 1.000000000000000000 ) ) ;
#39899 = DIRECTION ( 'NONE',  ( 0.000000000000000000, 0.000000000000000000, 1.000000000000000000 ) ) ;
#39900 = CARTESIAN_POINT ( 'NONE',  ( 84.86020291624612355, -30.49489077589588604, -12.39321520033835000 ) ) ;
#39901 = CARTESIAN_POINT ( 'NONE',  ( 137.5082292857710513, -4.434782517277369607, -8.403026514009534154 ) ) ;
#39902 = CARTESIAN_POINT ( 'NONE',  ( 114.4413348109119823, -0.8288870151387760510, -10.36305467784173118 ) ) ;
#39903 = DIRECTION ( 'NONE',  ( 1.000000000000000000, 0.000000000000000000, -0.000000000000000000 ) ) ;
#39904 = CARTESIAN_POINT ( 'NONE',  ( 70.19189222814998175, -60.40547808481815650, -37.36498982452450690 ) ) ;
#39905 = B_SPLINE_CURVE_WITH_KNOTS ( 'NONE', 3,
 ( #15169, #18375, #32263, #8109, #1031, #28859, #42771, #22010, #4671, #32484, #29076, #42987, #44577, #23603, #13111, #19713, #27246, #6023, #16762, #23369, #2833, #30206, #37721, #40241, #29977, #33834, #33599, #30659, #13342, #34291 ),
 .UNSPECIFIED., .F., .F.,
 ( 4, 2, 2, 1, 2, 2, 2, 1, 1, 2, 2, 2, 1, 1, 1, 2, 2, 4 ),
 ( 0.000000000000000000, 0.03124999999996751210, 0.06249999999993502420, 0.09374999999990253630, 0.1093749999998813865, 0.1249999999998602229, 0.1874999999997779832, 0.2187499999997450095, 0.2343749999997195577, 0.2421874999997072619, 0.2499999999996949385, 0.3749999999996284639, 0.4374999999996059818, 0.4687499999995839439, 0.4843749999995833888, 0.4921874999995830557, 0.4999999999995827782, 1.000000000000000000 ),
 .UNSPECIFIED. ) ;
#39906 = CARTESIAN_POINT ( 'NONE',  ( 113.8173414775786512, -9.565557343593413364, -10.61323700422348004 ) ) ;
#39907 = CARTESIAN_POINT ( 'NONE',  ( 113.1933481442453058, -4.089484607189486809, -7.948022111789456723 ) ) ;
#39908 = CARTESIAN_POINT ( 'NONE',  ( 116.6781481986166824, -8.393872295391240357, -17.05164434167983956 ) ) ;
#39909 = CARTESIAN_POINT ( 'NONE',  ( 123.3474214775786209, -0.1624402480850797581, -16.17319339645315424 ) ) ;
#39910 = DIRECTION ( 'NONE',  ( 0.9387755102040806765, -0.3445294493088623122, 0.000000000000000000 ) ) ;
#39911 = CARTESIAN_POINT ( 'NONE',  ( 118.1852948109119836, -5.638512984488999180, -18.83840828888717311 ) ) ;
#39912 = CARTESIAN_POINT ( 'NONE',  ( 120.5110881442453206, -6.344957434206665248, -7.627207830600338134 ) ) ;
#39913 = VERTEX_POINT ( 'NONE', #5801 ) ;
#39914 = CARTESIAN_POINT ( 'NONE',  ( 126.3671785243095940, -8.628592065323934079, -16.79579074909501202 ) ) ;
#39915 = CARTESIAN_POINT ( 'NONE',  ( 110.8298327545248299, -2.477300249445798297, -19.15521520033831138 ) ) ;
#39916 = CARTESIAN_POINT ( 'NONE',  ( 110.6909265045248247, -2.791137627527939813, -8.388885654883777576 ) ) ;
#39917 = CARTESIAN_POINT ( 'NONE',  ( 108.4684265045248424, -2.791137627527939813, -8.388885654883777576 ) ) ;
#39918 = AXIS2_PLACEMENT_3D ( 'NONE', #25060, #14797, #4063 ) ;
#39919 = CARTESIAN_POINT ( 'NONE',  ( 127.3434826498009755, -10.05615397309841441, -11.38986721830345061 ) ) ;
#39920 = CARTESIAN_POINT ( 'NONE',  ( 114.1009748109119784, -4.089484607189486809, -7.948022111789456723 ) ) ;
#39921 = ORIENTED_EDGE ( 'NONE', *, *, #14170, .F. ) ;
#39922 = CARTESIAN_POINT ( 'NONE',  ( 107.4266296295248821, -4.863998795839590272, -19.15521520033831493 ) ) ;
#39923 = CARTESIAN_POINT ( 'NONE',  ( 69.69189222814998175, -41.76310523276723785, -20.39321520033831447 ) ) ;
#39924 = CARTESIAN_POINT ( 'NONE',  ( 113.8740681442453138, -9.859900752359374465, -12.68260735090039404 ) ) ;
#39925 = EDGE_CURVE ( 'NONE', #43568, #35835, #13667, .T. ) ;
#39926 = CARTESIAN_POINT ( 'NONE',  ( 112.9664414775786412, 0.5811942927096154232, -14.16772938898807155 ) ) ;
#39927 = CARTESIAN_POINT ( 'NONE',  ( 119.6601881442453106, -8.166667518702819706, -8.995218007635861213 ) ) ;
#39928 = CARTESIAN_POINT ( 'NONE',  ( 109.5796765045248122, -7.250697342233347165, -19.15521520033831138 ) ) ;
#39929 = CARTESIAN_POINT ( 'NONE',  ( 119.5668260817262336, -2.423081321603731908, -17.89265170041263175 ) ) ;
#39930 = ORIENTED_EDGE ( 'NONE', *, *, #19476, .F. ) ;
#39931 = CARTESIAN_POINT ( 'NONE',  ( 110.7585566399283863, 0.4261359969231631739, -14.64321520033831447 ) ) ;
#39932 = CARTESIAN_POINT ( 'NONE',  ( 119.8303681442453126, 0.4262465694468514643, -12.03445270309931736 ) ) ;
#39933 = CARTESIAN_POINT ( 'NONE',  ( 114.4980614775786592, -7.893985811506177619, -18.51759400769804742 ) ) ;
#39934 = CARTESIAN_POINT ( 'NONE',  ( 114.8384214775786489, 0.9020085738987339008, -11.91225656197089222 ) ) ;
#39935 = CARTESIAN_POINT ( 'NONE',  ( 118.3179530757767566, -0.9924539043446216624, -17.29976612834909133 ) ) ;
#39936 = CARTESIAN_POINT ( 'NONE',  ( 121.6456214775786293, 0.4262465694468514643, -12.03445270309931736 ) ) ;
#39937 = CARTESIAN_POINT ( 'NONE',  ( 119.2631014775786298, -9.565557343593413364, -10.61323700422348004 ) ) ;
#39938 = ORIENTED_EDGE ( 'NONE', *, *, #17211, .F. ) ;
#39939 = CARTESIAN_POINT ( 'NONE',  ( 123.9106423109119675, -0.4387604401700512802, -15.73000352943951619 ) ) ;
#39940 = ADVANCED_FACE ( 'NONE', ( #6497, #23150, #6268 ), #12899, .F. ) ;
#39941 = CARTESIAN_POINT ( 'NONE',  ( 113.4769814775786330, -10.63000616557722466, -14.87417383870573495 ) ) ;
#39942 = CARTESIAN_POINT ( 'NONE',  ( 118.2987481442453088, -7.894159318335828068, -9.358103419637847864 ) ) ;
#39943 = EDGE_LOOP ( 'NONE', ( #36210, #27910, #30614, #25015 ) ) ;
#39944 = CARTESIAN_POINT ( 'NONE',  ( 110.8996837908067761, 0.5115630086001619059, -12.14321520033833224 ) ) ;
#39945 = CARTESIAN_POINT ( 'NONE',  ( 115.1787814775786387, -9.988377603198976828, -10.36322818467138340 ) ) ;
#39946 = CARTESIAN_POINT ( 'NONE',  ( 116.0388171295248014, -10.62599879583958540, -13.39321520033831447 ) ) ;
#39947 = CARTESIAN_POINT ( 'NONE',  ( 113.6471614775786492, -4.153390946401321671, -8.397313243818183892 ) ) ;
#39948 = ORIENTED_EDGE ( 'NONE', *, *, #22817, .T. ) ;
#39949 = VERTEX_POINT ( 'NONE', #23840 ) ;
#39950 = CARTESIAN_POINT ( 'NONE',  ( 123.1772414775786189, -5.574606645277164318, -18.38911715685844683 ) ) ;
#39951 = CARTESIAN_POINT ( 'NONE',  ( 122.7234281442452755, -4.153390946401325223, -8.397313243818185668 ) ) ;
#39952 = ORIENTED_EDGE ( 'NONE', *, *, #26730, .T. ) ;
#39953 = CARTESIAN_POINT ( 'NONE',  ( 74.66232006577804725, -2.500611837642884527, -7.993215200338315007 ) ) ;
#39954 = CARTESIAN_POINT ( 'NONE',  ( 62.13589673425203586, -65.32615175216918146, -44.81351878150378809 ) ) ;
#39955 = CARTESIAN_POINT ( 'NONE',  ( 108.5378796295247810, -4.863998795839590272, -19.15521520033831493 ) ) ;
#39956 = ADVANCED_FACE ( 'NONE', ( #10149 ), #37495, .T. ) ;
#39957 =( BOUNDED_SURFACE ( )  B_SPLINE_SURFACE ( 3, 2, ( 
 ( #41616, #3512, #25169 ),
 ( #7837, #21291, #31770 ),
 ( #39067, #21743, #24708 ),
 ( #38834, #42055, #31322 ),
 ( #6946, #38598, #41834 ),
 ( #35174, #7602, #20850 ),
 ( #21517, #96, #4179 ),
 ( #35632, #542, #14454 ),
 ( #31104, #31548, #3952 ),
 ( #17429, #45029, #13787 ) ),
 .UNSPECIFIED., .F., .F., .F. ) 
 B_SPLINE_SURFACE_WITH_KNOTS ( ( 4, 2, 2, 2, 4 ),
 ( 3, 3 ),
 ( 3.141592653589795336, 3.534291735288519920, 3.926990816987240063, 4.319689898685965090, 4.712388980384689674 ),
 ( 0.000000000000000000, 1.000000000000000000 ),
 .UNSPECIFIED. ) 
 GEOMETRIC_REPRESENTATION_ITEM ( )  RATIONAL_B_SPLINE_SURFACE ( (
 ( 1.000000000000000000, 0.8199175108841310067, 1.000000000000000000),
 ( 1.000000000000000000, 0.8199255829187760414, 1.000000000000000000),
 ( 1.000000000000000000, 0.8171960459197700199, 1.000000000000000000),
 ( 1.000000000000000000, 0.8065673029484310419, 1.000000000000000000),
 ( 1.000000000000000000, 0.7986592547571330636, 1.000000000000000000),
 ( 1.000000000000000000, 0.7784387827311890495, 1.000000000000000000),
 ( 1.000000000000000000, 0.7661249975918460464, 1.000000000000000000),
 ( 1.000000000000000000, 0.7384318888118330815, 1.000000000000000000),
 ( 1.000000000000000000, 0.7230611114418840080, 1.000000000000000000),
 ( 1.000000000000000000, 0.7071067811865480168, 1.000000000000000000) ) ) 
 REPRESENTATION_ITEM ( '' )  SURFACE ( )  );
#39958 = CARTESIAN_POINT ( 'NONE',  ( 115.1787814775786387, -9.988377603198976828, -10.36322818467138340 ) ) ;
#39960 = CARTESIAN_POINT ( 'NONE',  ( 115.5758681442453053, -7.894159318335828068, -9.358103419637847864 ) ) ;
#39959 = CARTESIAN_POINT ( 'NONE',  ( 113.9307948109119906, 0.9020085738987339008, -11.91225656197089222 ) ) ;
#39961 = CARTESIAN_POINT ( 'NONE',  ( 120.5110881442453206, -3.505236298600246325, -18.68346056562440793 ) ) ;
#39962 = FACE_BOUND ( 'NONE', #40208, .T. ) ;
#39963 = VERTEX_POINT ( 'NONE', #16542 ) ;
#39964 = CARTESIAN_POINT ( 'NONE',  ( 118.4689281442453392, -10.15424416112533912, -14.75197769757731336 ) ) ;
#39965 = DIRECTION ( 'NONE',  ( -1.000000000000000000, 0.000000000000000000, 0.000000000000000000 ) ) ;
#39966 = CARTESIAN_POINT ( 'NONE',  ( 114.0941296295247867, -4.863998795839590272, -19.15521520033831493 ) ) ;
#39967 = CARTESIAN_POINT ( 'NONE',  ( 113.9997534719562395, -1.125321370491267237, -17.12283323191015327 ) ) ;
#39968 = CARTESIAN_POINT ( 'NONE',  ( 112.4967077545247633, -7.250697342233347165, -7.631215200338321125 ) ) ;
#39969 = CARTESIAN_POINT ( 'NONE',  ( 117.2209414775786485, -7.893985811506177619, -18.51759400769804742 ) ) ;
#39970 = ORIENTED_EDGE ( 'NONE', *, *, #26137, .T. ) ;
#39971 = CARTESIAN_POINT ( 'NONE',  ( 122.0427081442452817, 0.5811942927096110934, -14.16772938898807510 ) ) ;
#39972 = DIRECTION ( 'NONE',  ( 0.5735764363510498232, -0.3127926500124802445, 0.7570804645221007600 ) ) ;
#39973 = CARTESIAN_POINT ( 'NONE',  ( 109.5102233795247884, -8.938348069036489818, -17.46756447353520159 ) ) ;
#39974 = CARTESIAN_POINT ( 'NONE',  ( 115.6893214775786447, 0.5811942927096154232, -14.16772938898807155 ) ) ;
#39975 = CARTESIAN_POINT ( 'NONE',  ( 117.2209414775786485, -7.893985811506177619, -18.51759400769804742 ) ) ;
#39976 = FACE_OUTER_BOUND ( 'NONE', #5883, .T. ) ;
#39977 = CARTESIAN_POINT ( 'NONE',  ( 116.7592683588497096, -11.76435134077275890, -6.215002696414487993 ) ) ;
#39978 = VERTEX_POINT ( 'NONE', #3069 ) ;
#39979 = CARTESIAN_POINT ( 'NONE',  ( -2.543030055175557802, -7.047612661366984277, -7.499921549712347257 ) ) ;
#39980 = CARTESIAN_POINT ( 'NONE',  ( 109.4154010812577837, -0.01829820670803256055, -12.14321520033831625 ) ) ;
#39981 = CARTESIAN_POINT ( 'NONE',  ( 119.0361948109119652, -2.084020599724406786, -8.691656652584148546 ) ) ;
#39982 = CARTESIAN_POINT ( 'NONE',  ( 110.1353015045248469, -6.936859964151250502, -18.39754474579286025 ) ) ;
#39983 = CARTESIAN_POINT ( 'NONE',  ( 105.8986608795248401, -8.938348069036489818, -9.318865927141430916 ) ) ;
#39984 = CARTESIAN_POINT ( 'NONE',  ( 118.7525614775786380, -1.833838273342659253, -17.42832698103878286 ) ) ;
#39985 = DIRECTION ( 'NONE',  ( 1.000000000000000000, 0.000000000000000000, -0.000000000000000000 ) ) ;
#39986 = CARTESIAN_POINT ( 'NONE',  ( 71.41205933791314919, -25.41584841807908646, -5.221760208415934024 ) ) ;
#39987 = CARTESIAN_POINT ( 'NONE',  ( 111.7184548109119788, -0.8288870151387760510, -10.36305467784173118 ) ) ;
#39988 = CARTESIAN_POINT ( 'NONE',  ( 119.1496481442453046, -3.383040157471821630, -19.15922257007629170 ) ) ;
#39989 = ORIENTED_EDGE ( 'NONE', *, *, #5533, .T. ) ;
#39990 = CARTESIAN_POINT ( 'NONE',  ( 120.2841814775786276, -10.15424416112533912, -14.75197769757731336 ) ) ;
#39991 = CARTESIAN_POINT ( 'NONE',  ( 116.1431348109119881, -10.30919188438810075, -12.61870101168855918 ) ) ;
#39992 = CARTESIAN_POINT ( 'NONE',  ( 121.3052614775786111, -1.834011780172310813, -8.268836392978581529 ) ) ;
#39993 = EDGE_CURVE ( 'NONE', #40407, #31774, #9241, .T. ) ;
#39994 = CARTESIAN_POINT ( 'NONE',  ( 119.4332814775786318, -8.899110576539710493, -16.42337572283490132 ) ) ;
#39995 = EDGE_LOOP ( 'NONE', ( #30802, #2029, #39047, #31796 ) ) ;
#39996 = CARTESIAN_POINT ( 'NONE',  ( 125.7866681442452688, -8.899110576539710493, -16.42337572283490132 ) ) ;
#39997 = CARTESIAN_POINT ( 'NONE',  ( 118.9794681442453026, -9.261995988541697145, -16.69588392320189030 ) ) ;
#39998 = CARTESIAN_POINT ( 'NONE',  ( 124.9063227527197313, -5.965318915412476386, -5.805585508435772368 ) ) ;
#39999 = B_SPLINE_CURVE_WITH_KNOTS ( 'NONE', 3,
 ( #25492, #19319, #19089, #33204, #36402, #8384, #22066, #5621, #36184, #28912 ),
 .UNSPECIFIED., .F., .F.,
 ( 4, 3, 3, 4 ),
 ( 0.000000000000000000, 0.0002476487219222714723, 0.0004952974148303440237, 0.0009534114850261710648 ),
 .UNSPECIFIED. ) ;
#40000 = CARTESIAN_POINT ( 'NONE',  ( 122.7801548109119665, -3.383040157471821630, -19.15922257007629170 ) ) ;
#40001 = CARTESIAN_POINT ( 'NONE',  ( 117.4110664975817713, -2.215723800389698184, -18.16877924232191788 ) ) ;
#40002 = CARTESIAN_POINT ( 'NONE',  ( 120.5074391859119913, -1.406689858478933353, -17.56299727309130887 ) ) ;
#40003 = CARTESIAN_POINT ( 'NONE',  ( 67.30914723170953096, -54.16566668288025710, -35.76359490593331003 ) ) ;
#40004 = CARTESIAN_POINT ( 'NONE',  ( 107.3571765045248299, -2.791137627527939813, -8.388885654883777576 ) ) ;
#40005 = VECTOR ( 'NONE', #14480, 1000.000000000000000 ) ;
#40006 = CARTESIAN_POINT ( 'NONE',  ( 64.61935771200890599, -37.86087448816891765, -4.893215200338314474 ) ) ;
#40007 = AXIS2_PLACEMENT_3D ( 'NONE', #6456, #12850, #9194 ) ;
#40008 = LINE ( 'NONE', #25660, #31685 ) ;
#40009 = CARTESIAN_POINT ( 'NONE',  ( 119.3198281442452924, -9.859900752359374465, -12.68260735090039404 ) ) ;
#40010 = CARTESIAN_POINT ( 'NONE',  ( 125.5597614775786326, -1.561330072975669392, -17.79121239304076951 ) ) ;
#40011 = CARTESIAN_POINT ( 'NONE',  ( 84.38170309240724976, -26.75858941326842810, -11.54476601486570964 ) ) ;
#40012 = ORIENTED_EDGE ( 'NONE', *, *, #9982, .F. ) ;
#40013 = CARTESIAN_POINT ( 'NONE',  ( 117.1532421295247843, 0.1360012041604560795, -13.39321520033831447 ) ) ;
#40014 = CARTESIAN_POINT ( 'NONE',  ( 110.9687390045248350, -9.868328341294098749, -11.32035403202665869 ) ) ;
#40015 = CARTESIAN_POINT ( 'NONE',  ( 115.5758681442453053, -7.894159318335828068, -9.358103419637847864 ) ) ;
#40016 = CARTESIAN_POINT ( 'NONE',  ( 115.0252186403692320, -1.196538596002799215, -17.02799684832027083 ) ) ;
#40017 = CARTESIAN_POINT ( 'NONE',  ( 65.88020736227775842, -0.1838173346746251047, -10.39321520033831625 ) ) ;
#40018 = CARTESIAN_POINT ( 'NONE',  ( -2.398579840503125560, -7.004315730407527418, -19.21681588960016640 ) ) ;
#40020 = CARTESIAN_POINT ( 'NONE',  ( 122.7234281442452755, -5.638512984488999180, -18.83840828888717311 ) ) ;
#40019 = CARTESIAN_POINT ( 'NONE',  ( 66.31928500851137187, -14.71576354012722021, -10.39321520033831625 ) ) ;
#40021 = CARTESIAN_POINT ( 'NONE',  ( 123.9146881442452894, -10.15424416112533912, -14.75197769757731336 ) ) ;
#40022 = ORIENTED_EDGE ( 'NONE', *, *, #38936, .F. ) ;
#40023 = CARTESIAN_POINT ( 'NONE',  ( 111.7184548109119788, -9.261995988541697145, -16.69588392320189030 ) ) ;
#40024 = CARTESIAN_POINT ( 'NONE',  ( 125.1626748109119802, -9.988377603198980381, -10.36322818467138518 ) ) ;
#40025 = B_SPLINE_CURVE_WITH_KNOTS ( 'NONE', 3,
 ( #18056, #14409, #28319, #42231, #28551, #24896, #38789, #4359, #18279, #9772, #23684, #37339, #6568, #6343, #9539 ),
 .UNSPECIFIED., .F., .F.,
 ( 4, 2, 2, 1, 1, 1, 2, 2, 4 ),
 ( 0.000000000000000000, 0.2500000000001662559, 0.3750000000002411404, 0.4375000000002858269, 0.4687500000003081979, 0.4843750000003191891, 0.4921875000003183565, 0.5000000000003175238, 1.000000000000000000 ),
 .UNSPECIFIED. ) ;
#40026 = CARTESIAN_POINT ( 'NONE',  ( 111.9410827545248708, -6.936859964151250502, -8.388885654883777576 ) ) ;
#40027 = CARTESIAN_POINT ( 'NONE',  ( 122.6099748109119929, -0.8288870151387760510, -10.36305467784173118 ) ) ;
#40028 = CARTESIAN_POINT ( 'NONE',  ( 118.8660148109119774, 0.1319031606808879209, -14.10382304977623669 ) ) ;
#40029 = CARTESIAN_POINT ( 'NONE',  ( 121.0408330757767459, -0.9924539043446216624, -17.29976612834909133 ) ) ;
#40030 = CARTESIAN_POINT ( 'NONE',  ( 106.3848327545248651, -2.477300249445798297, -19.15521520033831138 ) ) ;
#40031 = DIRECTION ( 'NONE',  ( -1.000000000000000000, 0.000000000000000000, 0.000000000000000000 ) ) ;
#40032 = CARTESIAN_POINT ( 'NONE',  ( 63.31042565271481948, -20.21815917793063733, -0.8932152003383146965 ) ) ;
#40033 = DIRECTION ( 'NONE',  ( 0.000000000000000000, 0.6004852223388321697, -0.7996358532186279566 ) ) ;
#40034 = CARTESIAN_POINT ( 'NONE',  ( 111.0381921295247878, 0.8980012041604618078, -13.39321520033831447 ) ) ;
#40035 = CARTESIAN_POINT ( 'NONE',  ( 116.4429452033932932, 2.229392703617450788, -20.41770221837591137 ) ) ;
#40036 = CARTESIAN_POINT ( 'NONE',  ( 83.86179762071230925, -31.76409560463467585, -23.03138878092153519 ) ) ;
#40037 = CARTESIAN_POINT ( 'NONE',  ( 122.8936081442453059, 0.2603800115204892296, -16.42320221600525088 ) ) ;
#40038 = CARTESIAN_POINT ( 'NONE',  ( 117.9583881442453048, -10.30919188438810075, -12.61870101168855918 ) ) ;
#40039 = CARTESIAN_POINT ( 'NONE',  ( 106.0375671295248310, -10.62599879583958540, -13.39321520033831447 ) ) ;
#40040 = CARTESIAN_POINT ( 'NONE',  ( 114.8951481442453115, -0.4660016031367893996, -10.09054647747474043 ) ) ;
#40041 = CARTESIAN_POINT ( 'NONE',  ( 123.7184548109119788, -4.683672500039349984, -14.88233656108870662 ) ) ;
#40042 = ORIENTED_EDGE ( 'NONE', *, *, #35289, .F. ) ;
#40043 = CARTESIAN_POINT ( 'NONE',  ( 116.4587108795247730, -8.399532701772287169, -9.857681294405580275 ) ) ;
#40044 = CARTESIAN_POINT ( 'NONE',  ( 124.2550481442452792, -9.988377603198980381, -10.36322818467138518 ) ) ;
#40045 = CARTESIAN_POINT ( 'NONE',  ( 120.5678148109119832, -8.166667518702819706, -8.995218007635861213 ) ) ;
#40046 = CIRCLE ( 'NONE', #28397, 3.000000000000003997 ) ;
#40047 = CARTESIAN_POINT ( 'NONE',  ( 124.4252281442452812, -0.8288870151387760510, -10.36305467784173118 ) ) ;
#40048 = CARTESIAN_POINT ( 'NONE',  ( 112.9097148109120070, -9.565557343593413364, -10.61323700422348004 ) ) ;
#40049 = CARTESIAN_POINT ( 'NONE',  ( 112.2289948109119848, -7.643976991954077427, -18.09477374809248928 ) ) ;
#40050 = ADVANCED_FACE ( 'NONE', ( #37951 ), #32089, .T. ) ;
#40051 = CARTESIAN_POINT ( 'NONE',  ( 108.9545983795247821, -0.7896495226426338832, -9.318865927141430916 ) ) ;
#40052 = AXIS2_PLACEMENT_3D ( 'NONE', #38453, #4480, #10665 ) ;
#40053 = CARTESIAN_POINT ( 'NONE',  ( 118.9227414775786542, 0.4262465694468514643, -12.03445270309931736 ) ) ;
#40054 = CARTESIAN_POINT ( 'NONE',  ( 124.9868051361382868, -12.36944789948101331, -14.53642012793133986 ) ) ;
#40055 = FACE_OUTER_BOUND ( 'NONE', #40457, .T. ) ;
#40056 = VERTEX_POINT ( 'NONE', #28359 ) ;
#40057 = AXIS2_PLACEMENT_3D ( 'NONE', #40294, #36851, #5619 ) ;
#40058 = EDGE_CURVE ( 'NONE', #32113, #37411, #43536, .T. ) ;
#40059 = DIRECTION ( 'NONE',  ( -1.000000000000000000, 0.000000000000000000, -0.000000000000000000 ) ) ;
#40060 = EDGE_CURVE ( 'NONE', #40384, #38773, #6598, .T. ) ;
#40061 = CARTESIAN_POINT ( 'NONE',  ( 123.3474214775786209, -9.988377603198976828, -10.36322818467138340 ) ) ;
#40062 = CARTESIAN_POINT ( 'NONE',  ( 122.0955187714537828, -6.306599966548167124, -18.84486539759072699 ) ) ;
#40063 = CARTESIAN_POINT ( 'NONE',  ( 61.69189222814998175, -49.76310523276723785, -24.89321520033831447 ) ) ;
#40064 = CARTESIAN_POINT ( 'NONE',  ( 117.7314814775786260, -5.574606645277164318, -18.38911715685844683 ) ) ;
#40065 = CARTESIAN_POINT ( 'NONE',  ( 67.01977926936005758, -0.08205263468559398365, -16.39321520033831092 ) ) ;
#40066 = LINE ( 'NONE', #12267, #1967 ) ;
#40067 = CARTESIAN_POINT ( 'NONE',  ( 122.8368814775786291, -7.894159318335828068, -9.358103419637847864 ) ) ;
#40068 = B_SPLINE_CURVE_WITH_KNOTS ( 'NONE', 3,
 ( #9115, #44458, #33949, #19149, #33032, #9342, #40583, #12318, #23018, #23251, #1806, #30536, #40127, #26450, #37133, #8891, #22789, #5909, #19829, #27123, #2717, #13224, #36683 ),
 .UNSPECIFIED., .F., .F.,
 ( 4, 2, 2, 1, 1, 2, 2, 2, 1, 1, 1, 2, 2, 4 ),
 ( 0.000000000000000000, 0.1249999999999793499, 0.1874999999999680811, 0.2187499999999644451, 0.2343749999999615308, 0.2421874999999592548, 0.2499999999999569511, 0.3749999999999196754, 0.4374999999999041322, 0.4687499999998942513, 0.4843749999998913647, 0.4921874999998912537, 0.4999999999998911981, 1.000000000000000000 ),
 .UNSPECIFIED. ) ;
#40069 = CARTESIAN_POINT ( 'NONE',  ( 109.6956031537514917, 0.4930828106259610433, -14.64321520033831447 ) ) ;
#40070 = EDGE_CURVE ( 'NONE', #39689, #44717, #39213, .T. ) ;
#40071 = CYLINDRICAL_SURFACE ( 'NONE', #28940, 3.000000000000001332 ) ;
#40072 = CIRCLE ( 'NONE', #42264, 2.000000000000000444 ) ;
#40073 = CARTESIAN_POINT ( 'NONE',  ( 124.6793944118516464, -11.84801880692714704, -16.90254992618838514 ) ) ;
#40074 = CARTESIAN_POINT ( 'NONE',  ( 123.2906948109119867, -8.166667518702819706, -8.995218007635861213 ) ) ;
#40075 = CARTESIAN_POINT ( 'NONE',  ( 116.8238548109119819, -5.574606645277164318, -18.38911715685844683 ) ) ;
#40076 = CARTESIAN_POINT ( 'NONE',  ( 122.5532481442453019, 0.4262465694468514643, -12.03445270309931736 ) ) ;
#40077 = ADVANCED_FACE ( 'NONE', ( #28591 ), #39957, .F. ) ;
#40078 = VERTEX_POINT ( 'NONE', #10372 ) ;
#40079 = CARTESIAN_POINT ( 'NONE',  ( 123.8579614775786126, 0.5811942927096110934, -14.16772938898807510 ) ) ;
#40080 = CARTESIAN_POINT ( 'NONE',  ( 114.2711548109119803, -9.988377603198976828, -10.36322818467138340 ) ) ;
#40081 = CARTESIAN_POINT ( 'NONE',  ( 116.5944421295247793, -9.868328341294093420, -13.39321520033831447 ) ) ;
#40082 = CARTESIAN_POINT ( 'NONE',  ( 138.2184548109119930, -4.863998795839242995, -13.39321520033831447 ) ) ;
#40083 = EDGE_CURVE ( 'NONE', #20305, #3693, #316, .T. ) ;
#40084 = EDGE_CURVE ( 'NONE', #10139, #25112, #14400, .T. ) ;
#40085 = CARTESIAN_POINT ( 'NONE',  ( 123.2339681442453241, -3.505236298600246325, -18.68346056562440793 ) ) ;
#40086 = CARTESIAN_POINT ( 'NONE',  ( 121.1350814775786233, 0.5811942927096110934, -14.16772938898807510 ) ) ;
#40087 = CARTESIAN_POINT ( 'NONE',  ( 114.5108483795247878, -0.7896495226426338832, -9.318865927141430916 ) ) ;
#40088 = CARTESIAN_POINT ( 'NONE',  ( 107.6349890045248401, -9.868328341294098749, -11.32035403202665869 ) ) ;
#40089 = CARTESIAN_POINT ( 'NONE',  ( 89.12784890491134604, -25.99489077589524300, -13.39321520033831625 ) ) ;
#40090 = CARTESIAN_POINT ( 'NONE',  ( 113.5904348109119866, -2.084020599724406786, -8.691656652584148546 ) ) ;
#40091 = VECTOR ( 'NONE', #17673, 1000.000000000000000 ) ;
#40092 = CARTESIAN_POINT ( 'NONE',  ( 122.2437673109119629, -9.289237151508428880, -11.05642687123710388 ) ) ;
#40093 = CARTESIAN_POINT ( 'NONE',  ( 114.8581140045248361, 0.1403307496149616695, -15.46607636864997204 ) ) ;
#40094 = ORIENTED_EDGE ( 'NONE', *, *, #24720, .F. ) ;
#40095 = CIRCLE ( 'NONE', #15323, 2.000000000000000444 ) ;
#40096 = CARTESIAN_POINT ( 'NONE',  ( 125.1059481442452750, -1.833838273342660141, -17.42832698103878286 ) ) ;
#40097 = CARTESIAN_POINT ( 'NONE',  ( 122.7993923109119692, -9.959231468620755479, -10.70263013195267199 ) ) ;
#40098 = CARTESIAN_POINT ( 'NONE',  ( 120.5074391859119913, -8.844754642576884152, -8.592115655440050404 ) ) ;
#40099 = DIRECTION ( 'NONE',  ( 0.000000000000000000, 0.000000000000000000, 1.000000000000000000 ) ) ;
#40100 = CARTESIAN_POINT ( 'NONE',  ( 107.7044421295247929, -9.868328341294093420, -13.39321520033831447 ) ) ;
#40101 = ORIENTED_EDGE ( 'NONE', *, *, #36464, .T. ) ;
#40102 = CARTESIAN_POINT ( 'NONE',  ( 119.7736414775786358, -10.30919188438810075, -12.61870101168855918 ) ) ;
#40103 = CARTESIAN_POINT ( 'NONE',  ( 112.9204024739652112, 0.3208234527006389447, -15.99825685930876595 ) ) ;
#40104 = CARTESIAN_POINT ( 'NONE',  ( 122.6099748109119929, -0.8288870151387760510, -10.36305467784173118 ) ) ;
#40105 = CARTESIAN_POINT ( 'NONE',  ( 114.1577014775786552, -3.505236298600246325, -18.68346056562440793 ) ) ;
#40106 = CARTESIAN_POINT ( 'NONE',  ( 70.89841814381148311, -68.89136543047671069, -37.69090763720760151 ) ) ;
#40107 = CARTESIAN_POINT ( 'NONE',  ( 123.9714148109119805, -0.4660016031367668621, -10.09054647747477063 ) ) ;
#40108 = CARTESIAN_POINT ( 'NONE',  ( 113.7606148109119886, -1.561330072975668060, -17.79121239304076596 ) ) ;
#40109 = CARTESIAN_POINT ( 'NONE',  ( 112.4967077545247633, -2.791137627527939813, -18.39754474579286025 ) ) ;
#40110 = CIRCLE ( 'NONE', #15380, 2.000000000000000444 ) ;
#40111 = CARTESIAN_POINT ( 'NONE',  ( 125.9001214775786224, -4.089484607189486809, -7.948022111789456723 ) ) ;
#40112 = CARTESIAN_POINT ( 'NONE',  ( 70.19189222814998175, -67.83330054016514055, -40.33609291459782753 ) ) ;
#40113 = VERTEX_POINT ( 'NONE', #17874 ) ;
#40114 = CARTESIAN_POINT ( 'NONE',  ( 115.9729548109119861, -6.344957434206662583, -7.627207830600332805 ) ) ;
#40115 = CARTESIAN_POINT ( 'NONE',  ( 114.3278814775786429, 0.1319031606808879209, -14.10382304977623669 ) ) ;
#40116 = CARTESIAN_POINT ( 'NONE',  ( 74.66232006577804725, -2.500611837642884527, -7.993215200338315007 ) ) ;
#40117 = EDGE_CURVE ( 'NONE', #17200, #452, #8206, .T. ) ;
#40118 = CARTESIAN_POINT ( 'NONE',  ( 113.7606148109119886, -1.561330072975668060, -17.79121239304076596 ) ) ;
#40119 = ORIENTED_EDGE ( 'NONE', *, *, #1608, .T. ) ;
#40120 = AXIS2_PLACEMENT_3D ( 'NONE', #11957, #32462, #11729 ) ;
#40121 = CARTESIAN_POINT ( 'NONE',  ( 122.4965214775786251, -10.30919188438810075, -12.61870101168855918 ) ) ;
#40122 = CARTESIAN_POINT ( 'NONE',  ( 59.92022724782403742, -14.76985616374063248, -8.596615087808567424 ) ) ;
#40123 = CARTESIAN_POINT ( 'NONE',  ( 110.3894297178593575, -0.3595008806742686081, -15.96590799893916213 ) ) ;
#40124 = AXIS2_PLACEMENT_3D ( 'NONE', #26239, #13416, #20479 ) ;
#40125 = CARTESIAN_POINT ( 'NONE',  ( 111.8886348109120092, -6.222761293078232114, -8.102969835052212133 ) ) ;
#40126 = EDGE_CURVE ( 'NONE', #11850, #42225, #1283, .T. ) ;
#40127 = CARTESIAN_POINT ( 'NONE',  ( 123.5612461215935554, -4.267240530208148641, -15.43691621075543452 ) ) ;
#40128 = CARTESIAN_POINT ( 'NONE',  ( 115.1787814775786387, -0.1624402480850797581, -16.17319339645315424 ) ) ;
#40129 = DIRECTION ( 'NONE',  ( -1.224775218828352108E-16, 0.9242245927363028635, 0.3818493186865928313 ) ) ;
#40130 = CARTESIAN_POINT ( 'NONE',  ( 125.0820341042009858, -1.685509051457968921, -20.18185560315022187 ) ) ;
#40131 = CARTESIAN_POINT ( 'NONE',  ( 125.6164881442453094, 0.2603800115204892296, -16.42320221600525088 ) ) ;
#40132 = CARTESIAN_POINT ( 'NONE',  ( 112.3991748109119868, -8.166667518702817929, -8.995218007635859436 ) ) ;
#40133 = CARTESIAN_POINT ( 'NONE',  ( 123.9800954359119771, 0.5291689781388270175, -13.89700978578772705 ) ) ;
#40134 = CARTESIAN_POINT ( 'NONE',  ( 111.8319081442453182, -5.638512984488999180, -18.83840828888717311 ) ) ;
#40135 = CARTESIAN_POINT ( 'NONE',  ( 114.3278814775786429, 0.1319031606808879209, -14.10382304977623669 ) ) ;
#40136 = CARTESIAN_POINT ( 'NONE',  ( 122.0994348109119443, 0.9020085738987339008, -11.91225656197089222 ) ) ;
#40137 = ADVANCED_FACE ( 'NONE', ( #26289 ), #26781, .T. ) ;
#40138 = CARTESIAN_POINT ( 'NONE',  ( 122.8368814775786291, -1.561330072975668948, -17.79121239304076951 ) ) ;
#40139 = VERTEX_POINT ( 'NONE', #29703 ) ;
#40140 = CARTESIAN_POINT ( 'NONE',  ( 127.0915067942439691, -8.465631742269270177, -17.46559197649120776 ) ) ;
#40141 = CARTESIAN_POINT ( 'NONE',  ( 112.4272546295247821, -4.863998795839590272, -7.631215200338315796 ) ) ;
#40142 = CARTESIAN_POINT ( 'NONE',  ( 109.9963952545248134, -9.868328341294098749, -15.46607636864997204 ) ) ;
#40143 = CARTESIAN_POINT ( 'NONE',  ( 107.2182702545248105, 0.1403307496149616695, -11.32035403202665336 ) ) ;
#40144 = AXIS2_PLACEMENT_3D ( 'NONE', #19266, #33596, #2372 ) ;
#40145 = CARTESIAN_POINT ( 'NONE',  ( 125.5492214775786550, -6.210324830719740064, -8.151390318758597431 ) ) ;
#40146 = CARTESIAN_POINT ( 'NONE',  ( 116.2565881442452991, -9.261995988541697145, -16.69588392320189030 ) ) ;
#40147 = ORIENTED_EDGE ( 'NONE', *, *, #45087, .T. ) ;
#40148 = CARTESIAN_POINT ( 'NONE',  ( 124.9924948109119924, -4.089484607189486809, -7.948022111789456723 ) ) ;
#40149 = CARTESIAN_POINT ( 'NONE',  ( 124.5308374810065430, -10.18911555409675707, -12.76055059223490318 ) ) ;
#40150 = CARTESIAN_POINT ( 'NONE',  ( 84.86020291624612355, -30.49489077589588604, -18.39321520033831803 ) ) ;
#40151 = EDGE_CURVE ( 'NONE', #37757, #38164, #22414, .T. ) ;
#40152 = CARTESIAN_POINT ( 'NONE',  ( 113.6471614775786492, -4.153390946401321671, -8.397313243818183892 ) ) ;
#40153 =( BOUNDED_SURFACE ( )  B_SPLINE_SURFACE ( 1, 2, ( 
 ( #25694, #11112, #28891, #32515, #14527, #39600, #11564, #14978, #28441, #391, #8361, #7678, #28668, #24788, #32298, #836, #17948, #4485, #4254, #1063, #39144, #7909, #22265, #18406, #39375, #35710, #18172, #36159, #21816, #38680, #21366, #35937, #7446, #14755, #25471, #29106, #25014, #8143, #4928, #18843, #22044, #4705, #14304, #18625, #35480, #1290, #38907, #28222, #42572, #42129, #35249, #21593, #4026, #31847, #617, #11335, #40040, #36381, #33399, #33179, #40272, #43689, #19522, #8806, #9039, #5599, #43248, #37053, #12465, #26590, #12239, #12013, #40503, #1955, #37284, #39820, #8587, #32734, #6052, #23175, #22710, #16332, #22936, #2173, #15881, #25915, #15428, #5824, #44156, #19300, #29778, #36829, #26365, #22487, #30006, #29556, #1508, #16103, #29333, #19744, #43922, #5152, #33628, #19069, #32953, #40729, #1730, #15655, #9264, #36608, #12691, #43473, #2404, #30234, #12921, #26136, #5383, #26817, #9485, #23398, #13371, #34095, #20210, #2862, #13812, #17236, #6289, #38191, #27723, #3534, #27275, #10394, #3092, #27045, #16792, #20434, #37516, #2632, #10174, #24519, #38406, #23863, #20875, #41639, #17018, #30688, #9949, #37749, #24304, #41189, #24080, #27499, #44607, #40963, #6749, #6519, #6967, #34752, #34318, #19974, #37973, #30910, #17450, #44832, #31345, #13589, #27946, #16564, #33862, #41419, #9717, #41856, #31127, #45052, #119, #3314, #20659, #14032, #10617, #30459, #34535, #44379, #13142, #23630, #25418, #4432, #39319, #4649, #779, #35427, #38621, #1012, #18571, #28839, #8087, #7398, #566, #28615, #18121, #42524, #3975, #11285, #18349, #339, #21989, #4203, #10837, #35879, #34964, #24962, #14701, #14252, #25193, #39091, #28169, #32463, #7860, #1238, #14928, #32016, #15150, #42749, #31794, #11514, #29056, #21316, #7626, #42964, #21540, #35200, #11730, #21766, #17674, #25644, #35660, #3752, #7177, #31570, #21086, #42078, #32241, #24733, #17897, #11059, #14476, #28385, #42297, #38858, #12411, #33347, #29723, #43416, #16283, #1896, #4877, #15374, #29956 ),
 ( #2121, #5328, #36997, #16050, #19013, #43871, #12643, #25858, #39987, #5768, #8753, #8533, #19689, #33127, #18795, #30185, #19244, #36106, #26539, #32684, #40449, #9211, #15824, #22658, #36554, #22435, #12182, #1454, #43637, #11959, #32899, #36328, #39763, #5098, #23120, #36776, #1675, #33576, #2351, #44103, #15598, #12868, #26311, #29278, #29501, #40219, #26083, #22210, #8984, #39547, #8309, #22882, #43194, #5547, #19464, #44330, #16739, #30634, #34481, #2810, #16963, #34267, #26988, #33809, #13539, #44550, #3260, #13762, #13314, #66, #30857, #37698, #17185, #23810, #31075, #20381, #34700, #23342, #26768, #6470, #2580, #3487, #24029, #37919, #45002, #10125, #44780, #20821, #27671, #41586, #27221, #31292, #10343, #41138, #24248, #6695, #38140, #6912, #3041, #9898, #13090, #20606, #17403, #40677, #9429, #6000, #37226, #27447, #19923, #16510, #30409, #40908, #9662, #23581, #34042, #37464, #41369, #6237, #20159, #7128, #41806, #32185, #25364, #509, #11007, #21485, #14420, #21039, #11231, #10784, #27892, #31957, #10564, #4371, #24906, #34912, #14873, #13978, #287, #21931, #28115, #42020, #21712, #21263, #35370, #24460, #42468, #24681, #42691, #3703, #11460, #35599, #31515, #38568, #31740, #7572, #14646, #38352, #17622, #8024, #32409, #28785, #39260, #7346, #25139, #957, #35144, #35823, #39033, #28561, #3923, #14198, #4597, #17843, #42242, #28330, #723, #38802, #4148, #18066, #7804, #18290, #18518, #39936, #23059, #19189, #40164, #36502, #5044, #36945, #8697, #11676, #22158, #36720, #25585, #15539, #43584, #15995, #43132, #5271, #5715, #19633, #22828, #22602, #43817, #33068, #36277, #1840, #29225, #1182, #1618, #33296, #15769, #8477, #26031, #18742, #36052, #15096, #22381, #4819, #29672, #29444, #12354, #12128, #26254, #18959, #8926, #5489, #39487, #19409, #2072, #29901, #25803, #12582, #26487, #11902, #40391, #29005, #42914, #9153, #8252, #32633, #1399, #32849, #15315, #39713, #43359, #23522, #44725, #30572, #44276, #33984, #23285, #26709, #3206, #30351, #9376 ) ),
 .UNSPECIFIED., .F., .F., .T. ) 
 B_SPLINE_SURFACE_WITH_KNOTS ( ( 2, 2 ),
 ( 3, 2, 2, 2, 2, 2, 2, 2, 2, 2, 2, 2, 2, 2, 2, 2, 2, 2, 2, 2, 2, 2, 2, 2, 2, 2, 2, 2, 2, 2, 2, 2, 2, 2, 2, 2, 2, 2, 2, 2, 2, 2, 2, 2, 2, 2, 2, 2, 2, 2, 2, 2, 2, 2, 2, 2, 2, 2, 2, 2, 2, 2, 2, 2, 2, 2, 2, 2, 2, 2, 2, 2, 2, 2, 2, 2, 2, 2, 2, 2, 2, 2, 2, 2, 2, 2, 2, 2, 2, 2, 2, 2, 2, 2, 2, 2, 2, 2, 2, 2, 2, 2, 2, 2, 2, 2, 2, 2, 2, 2, 2, 2, 2, 2, 2, 2, 2, 2, 2, 2, 2, 2, 2, 2, 2, 2, 2, 2, 3 ),
 ( 0.000000000000000000, 1.000000000000000000 ),
 ( 0.000000000000000000, 0.007812500000000000000, 0.01562500000000000000, 0.02343750000000000000, 0.03125000000000000000, 0.03906250000000000000, 0.04687500000000000000, 0.05468750000000000000, 0.06250000000000000000, 0.07031250000000000000, 0.07812500000000000000, 0.08593750000000000000, 0.09375000000000000000, 0.1015625000000000000, 0.1093750000000000000, 0.1171875000000000000, 0.1250000000000000000, 0.1328125000000000000, 0.1406250000000000000, 0.1484375000000000000, 0.1562500000000000000, 0.1640625000000000000, 0.1718750000000000000, 0.1796875000000000000, 0.1875000000000000000, 0.1953125000000000000, 0.2031250000000000000, 0.2109375000000000000, 0.2187500000000000000, 0.2265625000000000000, 0.2343750000000000000, 0.2421875000000000000, 0.2500000000000000000, 0.2578125000000000000, 0.2656250000000000000, 0.2734375000000000000, 0.2812500000000000000, 0.2890625000000000000, 0.2968750000000000000, 0.3046875000000000000, 0.3125000000000000000, 0.3203125000000000000, 0.3281250000000000000, 0.3359375000000000000, 0.3437500000000000000, 0.3515625000000000000, 0.3593750000000000000, 0.3671875000000000000, 0.3750000000000000000, 0.3828125000000000000, 0.3906250000000000000, 0.3984375000000000000, 0.4062500000000000000, 0.4140625000000000000, 0.4218750000000000000, 0.4296875000000000000, 0.4375000000000000000, 0.4453125000000000000, 0.4531250000000000000, 0.4609375000000000000, 0.4687500000000000000, 0.4765625000000000000, 0.4843750000000000000, 0.4921875000000000000, 0.5000000000000000000, 0.5078125000000000000, 0.5156250000000000000, 0.5234375000000000000, 0.5312500000000000000, 0.5390625000000000000, 0.5468750000000000000, 0.5546875000000000000, 0.5625000000000000000, 0.5703125000000000000, 0.5781250000000000000, 0.5859375000000000000, 0.5937500000000000000, 0.6015625000000000000, 0.6093750000000000000, 0.6171875000000000000, 0.6250000000000000000, 0.6328125000000000000, 0.6406250000000000000, 0.6484375000000000000, 0.6562500000000000000, 0.6640625000000000000, 0.6718750000000000000, 0.6796875000000000000, 0.6875000000000000000, 0.6953125000000000000, 0.7031250000000000000, 0.7109375000000000000, 0.7187500000000000000, 0.7265625000000000000, 0.7343750000000000000, 0.7421875000000000000, 0.7500000000000000000, 0.7578125000000000000, 0.7656250000000000000, 0.7734375000000000000, 0.7812500000000000000, 0.7890625000000000000, 0.7968750000000000000, 0.8046875000000000000, 0.8125000000000000000, 0.8203125000000000000, 0.8281250000000000000, 0.8359375000000000000, 0.8437500000000000000, 0.8515625000000000000, 0.8593750000000000000, 0.8671875000000000000, 0.8750000000000000000, 0.8828125000000000000, 0.8906250000000000000, 0.8984375000000000000, 0.9062500000000000000, 0.9140625000000000000, 0.9218750000000000000, 0.9296875000000000000, 0.9375000000000000000, 0.9453125000000000000, 0.9531250000000000000, 0.9609375000000000000, 0.9687500000000000000, 0.9765625000000000000, 0.9843750000000000000, 0.9921875000000000000, 1.000000000000000000 ),
 .UNSPECIFIED. ) 
 GEOMETRIC_REPRESENTATION_ITEM ( )  RATIONAL_B_SPLINE_SURFACE ( (
 ( 1.000000000000000000, 0.9238795325112869605, 1.000000000000000000, 0.9238795325112869605, 1.000000000000000000, 0.9238795325112869605, 1.000000000000000000, 0.9238795325112869605, 1.000000000000000000, 0.9238795325112869605, 1.000000000000000000, 0.9238795325112869605, 1.000000000000000000, 0.9238795325112869605, 1.000000000000000000, 0.9238795325112869605, 1.000000000000000000, 0.9238795325112869605, 1.000000000000000000, 0.9238795325112869605, 1.000000000000000000, 0.9238795325112869605, 1.000000000000000000, 0.9238795325112869605, 1.000000000000000000, 0.9238795325112869605, 1.000000000000000000, 0.9238795325112869605, 1.000000000000000000, 0.9238795325112869605, 1.000000000000000000, 0.9238795325112869605, 1.000000000000000000, 0.9238795325112869605, 1.000000000000000000, 0.9238795325112869605, 1.000000000000000000, 0.9238795325112869605, 1.000000000000000000, 0.9238795325112869605, 1.000000000000000000, 0.9238795325112869605, 1.000000000000000000, 0.9238795325112869605, 1.000000000000000000, 0.9238795325112869605, 1.000000000000000000, 0.9238795325112869605, 1.000000000000000000, 0.9238795325112869605, 1.000000000000000000, 0.9238795325112869605, 1.000000000000000000, 0.9238795325112869605, 1.000000000000000000, 0.9238795325112869605, 1.000000000000000000, 0.9238795325112869605, 1.000000000000000000, 0.9238795325112869605, 1.000000000000000000, 0.9238795325112869605, 1.000000000000000000, 0.9238795325112869605, 1.000000000000000000, 0.9238795325112869605, 1.000000000000000000, 0.9238795325112869605, 1.000000000000000000, 0.9238795325112869605, 1.000000000000000000, 0.9238795325112869605, 1.000000000000000000, 0.9238795325112869605, 1.000000000000000000, 0.9238795325112869605, 1.000000000000000000, 0.9238795325112869605, 1.000000000000000000, 0.9238795325112869605, 1.000000000000000000, 0.9238795325112869605, 1.000000000000000000, 0.9238795325112869605, 1.000000000000000000, 0.9238795325112869605, 1.000000000000000000, 0.9238795325112869605, 1.000000000000000000, 0.9238795325112869605, 1.000000000000000000, 0.9238795325112869605, 1.000000000000000000, 0.9238795325112869605, 1.000000000000000000, 0.9238795325112869605, 1.000000000000000000, 0.9238795325112869605, 1.000000000000000000, 0.9238795325112869605, 1.000000000000000000, 0.9238795325112869605, 1.000000000000000000, 0.9238795325112869605, 1.000000000000000000, 0.9238795325112869605, 1.000000000000000000, 0.9238795325112869605, 1.000000000000000000, 0.9238795325112869605, 1.000000000000000000, 0.9238795325112869605, 1.000000000000000000, 0.9238795325112869605, 1.000000000000000000, 0.9238795325112869605, 1.000000000000000000, 0.9238795325112869605, 1.000000000000000000, 0.9238795325112869605, 1.000000000000000000, 0.9238795325112869605, 1.000000000000000000, 0.9238795325112869605, 1.000000000000000000, 0.9238795325112869605, 1.000000000000000000, 0.9238795325112869605, 1.000000000000000000, 0.9238795325112869605, 1.000000000000000000, 0.9238795325112869605, 1.000000000000000000, 0.9238795325112869605, 1.000000000000000000, 0.9238795325112869605, 1.000000000000000000, 0.9238795325112869605, 1.000000000000000000, 0.9238795325112869605, 1.000000000000000000, 0.9238795325112869605, 1.000000000000000000, 0.9238795325112869605, 1.000000000000000000, 0.9238795325112869605, 1.000000000000000000, 0.9238795325112869605, 1.000000000000000000, 0.9238795325112869605, 1.000000000000000000, 0.9238795325112869605, 1.000000000000000000, 0.9238795325112869605, 1.000000000000000000, 0.9238795325112869605, 1.000000000000000000, 0.9238795325112869605, 1.000000000000000000, 0.9238795325112869605, 1.000000000000000000, 0.9238795325112869605, 1.000000000000000000, 0.9238795325112869605, 1.000000000000000000, 0.9238795325112869605, 1.000000000000000000, 0.9238795325112869605, 1.000000000000000000, 0.9238795325112869605, 1.000000000000000000, 0.9238795325112869605, 1.000000000000000000, 0.9238795325112869605, 1.000000000000000000, 0.9238795325112869605, 1.000000000000000000, 0.9238795325112869605, 1.000000000000000000, 0.9238795325112869605, 1.000000000000000000, 0.9238795325112869605, 1.000000000000000000, 0.9238795325112869605, 1.000000000000000000, 0.9238795325112869605, 1.000000000000000000, 0.9238795325112869605, 1.000000000000000000, 0.9238795325112869605, 1.000000000000000000, 0.9238795325112869605, 1.000000000000000000, 0.9238795325112869605, 1.000000000000000000, 0.9238795325112869605, 1.000000000000000000, 0.9238795325112869605, 1.000000000000000000, 0.9238795325112869605, 1.000000000000000000, 0.9238795325112869605, 1.000000000000000000, 0.9238795325112869605, 1.000000000000000000, 0.9238795325112869605, 1.000000000000000000, 0.9238795325112869605, 1.000000000000000000, 0.9238795325112869605, 1.000000000000000000, 0.9238795325112869605, 1.000000000000000000, 0.9238795325112869605, 1.000000000000000000, 0.9238795325112869605, 1.000000000000000000, 0.9238795325112869605, 1.000000000000000000, 0.9238795325112869605, 1.000000000000000000, 0.9238795325112869605, 1.000000000000000000, 0.9238795325112869605, 1.000000000000000000, 0.9238795325112869605, 1.000000000000000000, 0.9238795325112869605, 1.000000000000000000, 0.9238795325112869605, 1.000000000000000000, 0.9238795325112869605, 1.000000000000000000, 0.9238795325112869605, 1.000000000000000000, 0.9238795325112869605, 1.000000000000000000, 0.9238795325112869605, 1.000000000000000000, 0.9238795325112869605, 1.000000000000000000, 0.9238795325112869605, 1.000000000000000000, 0.9238795325112869605, 1.000000000000000000, 0.9238795325112869605, 1.000000000000000000, 0.9238795325112869605, 1.000000000000000000, 0.9238795325112869605, 1.000000000000000000, 0.9238795325112869605, 1.000000000000000000, 0.9238795325112869605, 1.000000000000000000, 0.9238795325112869605, 1.000000000000000000),
 ( 1.000000000000000000, 0.9238795325112869605, 1.000000000000000000, 0.9238795325112869605, 1.000000000000000000, 0.9238795325112869605, 1.000000000000000000, 0.9238795325112869605, 1.000000000000000000, 0.9238795325112869605, 1.000000000000000000, 0.9238795325112869605, 1.000000000000000000, 0.9238795325112869605, 1.000000000000000000, 0.9238795325112869605, 1.000000000000000000, 0.9238795325112869605, 1.000000000000000000, 0.9238795325112869605, 1.000000000000000000, 0.9238795325112869605, 1.000000000000000000, 0.9238795325112869605, 1.000000000000000000, 0.9238795325112869605, 1.000000000000000000, 0.9238795325112869605, 1.000000000000000000, 0.9238795325112869605, 1.000000000000000000, 0.9238795325112869605, 1.000000000000000000, 0.9238795325112869605, 1.000000000000000000, 0.9238795325112869605, 1.000000000000000000, 0.9238795325112869605, 1.000000000000000000, 0.9238795325112869605, 1.000000000000000000, 0.9238795325112869605, 1.000000000000000000, 0.9238795325112869605, 1.000000000000000000, 0.9238795325112869605, 1.000000000000000000, 0.9238795325112869605, 1.000000000000000000, 0.9238795325112869605, 1.000000000000000000, 0.9238795325112869605, 1.000000000000000000, 0.9238795325112869605, 1.000000000000000000, 0.9238795325112869605, 1.000000000000000000, 0.9238795325112869605, 1.000000000000000000, 0.9238795325112869605, 1.000000000000000000, 0.9238795325112869605, 1.000000000000000000, 0.9238795325112869605, 1.000000000000000000, 0.9238795325112869605, 1.000000000000000000, 0.9238795325112869605, 1.000000000000000000, 0.9238795325112869605, 1.000000000000000000, 0.9238795325112869605, 1.000000000000000000, 0.9238795325112869605, 1.000000000000000000, 0.9238795325112869605, 1.000000000000000000, 0.9238795325112869605, 1.000000000000000000, 0.9238795325112869605, 1.000000000000000000, 0.9238795325112869605, 1.000000000000000000, 0.9238795325112869605, 1.000000000000000000, 0.9238795325112869605, 1.000000000000000000, 0.9238795325112869605, 1.000000000000000000, 0.9238795325112869605, 1.000000000000000000, 0.9238795325112869605, 1.000000000000000000, 0.9238795325112869605, 1.000000000000000000, 0.9238795325112869605, 1.000000000000000000, 0.9238795325112869605, 1.000000000000000000, 0.9238795325112869605, 1.000000000000000000, 0.9238795325112869605, 1.000000000000000000, 0.9238795325112869605, 1.000000000000000000, 0.9238795325112869605, 1.000000000000000000, 0.9238795325112869605, 1.000000000000000000, 0.9238795325112869605, 1.000000000000000000, 0.9238795325112869605, 1.000000000000000000, 0.9238795325112869605, 1.000000000000000000, 0.9238795325112869605, 1.000000000000000000, 0.9238795325112869605, 1.000000000000000000, 0.9238795325112869605, 1.000000000000000000, 0.9238795325112869605, 1.000000000000000000, 0.9238795325112869605, 1.000000000000000000, 0.9238795325112869605, 1.000000000000000000, 0.9238795325112869605, 1.000000000000000000, 0.9238795325112869605, 1.000000000000000000, 0.9238795325112869605, 1.000000000000000000, 0.9238795325112869605, 1.000000000000000000, 0.9238795325112869605, 1.000000000000000000, 0.9238795325112869605, 1.000000000000000000, 0.9238795325112869605, 1.000000000000000000, 0.9238795325112869605, 1.000000000000000000, 0.9238795325112869605, 1.000000000000000000, 0.9238795325112869605, 1.000000000000000000, 0.9238795325112869605, 1.000000000000000000, 0.9238795325112869605, 1.000000000000000000, 0.9238795325112869605, 1.000000000000000000, 0.9238795325112869605, 1.000000000000000000, 0.9238795325112869605, 1.000000000000000000, 0.9238795325112869605, 1.000000000000000000, 0.9238795325112869605, 1.000000000000000000, 0.9238795325112869605, 1.000000000000000000, 0.9238795325112869605, 1.000000000000000000, 0.9238795325112869605, 1.000000000000000000, 0.9238795325112869605, 1.000000000000000000, 0.9238795325112869605, 1.000000000000000000, 0.9238795325112869605, 1.000000000000000000, 0.9238795325112869605, 1.000000000000000000, 0.9238795325112869605, 1.000000000000000000, 0.9238795325112869605, 1.000000000000000000, 0.9238795325112869605, 1.000000000000000000, 0.9238795325112869605, 1.000000000000000000, 0.9238795325112869605, 1.000000000000000000, 0.9238795325112869605, 1.000000000000000000, 0.9238795325112869605, 1.000000000000000000, 0.9238795325112869605, 1.000000000000000000, 0.9238795325112869605, 1.000000000000000000, 0.9238795325112869605, 1.000000000000000000, 0.9238795325112869605, 1.000000000000000000, 0.9238795325112869605, 1.000000000000000000, 0.9238795325112869605, 1.000000000000000000, 0.9238795325112869605, 1.000000000000000000, 0.9238795325112869605, 1.000000000000000000, 0.9238795325112869605, 1.000000000000000000, 0.9238795325112869605, 1.000000000000000000, 0.9238795325112869605, 1.000000000000000000, 0.9238795325112869605, 1.000000000000000000, 0.9238795325112869605, 1.000000000000000000, 0.9238795325112869605, 1.000000000000000000, 0.9238795325112869605, 1.000000000000000000, 0.9238795325112869605, 1.000000000000000000, 0.9238795325112869605, 1.000000000000000000, 0.9238795325112869605, 1.000000000000000000, 0.9238795325112869605, 1.000000000000000000, 0.9238795325112869605, 1.000000000000000000, 0.9238795325112869605, 1.000000000000000000, 0.9238795325112869605, 1.000000000000000000, 0.9238795325112869605, 1.000000000000000000, 0.9238795325112869605, 1.000000000000000000, 0.9238795325112869605, 1.000000000000000000, 0.9238795325112869605, 1.000000000000000000, 0.9238795325112869605, 1.000000000000000000, 0.9238795325112869605, 1.000000000000000000, 0.9238795325112869605, 1.000000000000000000, 0.9238795325112869605, 1.000000000000000000, 0.9238795325112869605, 1.000000000000000000, 0.9238795325112869605, 1.000000000000000000, 0.9238795325112869605, 1.000000000000000000, 0.9238795325112869605, 1.000000000000000000) ) ) 
 REPRESENTATION_ITEM ( '' )  SURFACE ( )  );
#40154 = CARTESIAN_POINT ( 'NONE',  ( 121.2485348109119769, -0.4660016031367893996, -10.09054647747474043 ) ) ;
#40155 = CARTESIAN_POINT ( 'NONE',  ( 108.8156921295247912, 0.8980012041604618078, -13.39321520033831447 ) ) ;
#40156 = CARTESIAN_POINT ( 'NONE',  ( 94.20708369096698220, -25.14343533174585943, -14.10537061818067883 ) ) ;
#40157 = ORIENTED_EDGE ( 'NONE', *, *, #7871, .F. ) ;
#40158 = DIRECTION ( 'NONE',  ( 0.000000000000000000, -0.3818493186865927203, 0.9242245927363029745 ) ) ;
#40159 = AXIS2_PLACEMENT_3D ( 'NONE', #271, #3473, #24446 ) ;
#40160 = CARTESIAN_POINT ( 'NONE',  ( 119.7169148109119874, -0.1624402480850797581, -16.17319339645315424 ) ) ;
#40161 = CARTESIAN_POINT ( 'NONE',  ( 118.4689281442453392, 0.9020085738987339008, -11.91225656197089222 ) ) ;
#40162 = CARTESIAN_POINT ( 'NONE',  ( 114.0442481442453300, -1.834011780172310813, -8.268836392978581529 ) ) ;
#40163 = CARTESIAN_POINT ( 'NONE',  ( 118.6842048136183365, -3.929494816604741203, -18.62311481910882804 ) ) ;
#40164 = CARTESIAN_POINT ( 'NONE',  ( 121.8158014775786171, -4.153390946401325223, -8.397313243818185668 ) ) ;
#40165 = CARTESIAN_POINT ( 'NONE',  ( 120.9649014775786355, -6.222761293078241884, -8.102969835052219238 ) ) ;
#40166 = EDGE_LOOP ( 'NONE', ( #34966, #44206, #36163, #1382, #24011 ) ) ;
#40167 = CARTESIAN_POINT ( 'NONE',  ( 122.0354079359119908, -5.444069387712269226, -19.60292469916370450 ) ) ;
#40168 = CARTESIAN_POINT ( 'NONE',  ( 113.3068014775786594, -8.166667518702817929, -8.995218007635859436 ) ) ;
#40169 = CARTESIAN_POINT ( 'NONE',  ( 122.4965214775786251, 0.1319031606808879209, -14.10382304977623669 ) ) ;
#40170 = ORIENTED_EDGE ( 'NONE', *, *, #28069, .T. ) ;
#40171 = CARTESIAN_POINT ( 'NONE',  ( 124.1884548109119777, -2.527210466738041728, -8.967976844669124148 ) ) ;
#40172 = CARTESIAN_POINT ( 'NONE',  ( 116.7671281442453335, -1.834011780172310813, -8.268836392978581529 ) ) ;
#40173 = CARTESIAN_POINT ( 'NONE',  ( 113.8163171295247764, -10.62599879583958540, -13.39321520033831447 ) ) ;
#40174 = CARTESIAN_POINT ( 'NONE',  ( 116.3133148109120043, -2.084020599724406786, -8.691656652584148546 ) ) ;
#40175 = ORIENTED_EDGE ( 'NONE', *, *, #7441, .T. ) ;
#40176 = EDGE_LOOP ( 'NONE', ( #18015, #19931, #42426, #28286, #27755 ) ) ;
#40177 = AXIS2_PLACEMENT_3D ( 'NONE', #28060, #31242, #454 ) ;
#40178 = CARTESIAN_POINT ( 'NONE',  ( 123.6877814775786533, -6.222761293078241884, -8.102969835052219238 ) ) ;
#40179 = CARTESIAN_POINT ( 'NONE',  ( 121.5888948109119809, 0.1319031606808879209, -14.10382304977623669 ) ) ;
#40180 = DIRECTION ( 'NONE',  ( 0.9609149988134837450, -0.1028163501681639419, 0.2570431154366518145 ) ) ;
#40181 = EDGE_CURVE ( 'NONE', #9778, #2680, #20949, .T. ) ;
#40182 = ORIENTED_EDGE ( 'NONE', *, *, #39993, .T. ) ;
#40183 = CARTESIAN_POINT ( 'NONE',  ( 71.36400868967236022, -24.42718413923373788, -4.893215200338314474 ) ) ;
#40184 = CARTESIAN_POINT ( 'NONE',  ( 118.1852948109119836, -5.638512984488999180, -18.83840828888717311 ) ) ;
#40185 = CARTESIAN_POINT ( 'NONE',  ( 76.69189222814998175, -49.76310523276723785, -19.39321520033831447 ) ) ;
#40186 = VECTOR ( 'NONE', #31881, 1000.000000000000000 ) ;
#40187 = CARTESIAN_POINT ( 'NONE',  ( 117.1642148109119859, -9.261995988541697145, -16.69588392320189030 ) ) ;
#40189 = CARTESIAN_POINT ( 'NONE',  ( 116.7671281442453335, -7.643976991954077427, -18.09477374809248928 ) ) ;
#40188 = CARTESIAN_POINT ( 'NONE',  ( 116.5969481442453031, 0.5811942927096154232, -14.16772938898807155 ) ) ;
#40190 = CARTESIAN_POINT ( 'NONE',  ( 122.4397948109119767, -0.1624402480850797581, -16.17319339645315424 ) ) ;
#40191 = CARTESIAN_POINT ( 'NONE',  ( 113.4769814775786330, -10.63000616557722466, -14.87417383870573495 ) ) ;
#40192 = VERTEX_POINT ( 'NONE', #39525 ) ;
#40193 = CARTESIAN_POINT ( 'NONE',  ( 119.8870948109119752, -0.8288870151387760510, -10.36305467784173118 ) ) ;
#40194 = CYLINDRICAL_SURFACE ( 'NONE', #19115, 0.5000000000000039968 ) ;
#40195 = CARTESIAN_POINT ( 'NONE',  ( 113.1217858795247935, -0.7896495226426338832, -17.46756447353520159 ) ) ;
#40196 = CARTESIAN_POINT ( 'NONE',  ( 69.36136150295220659, -54.61625449731858595, -31.94451292116425023 ) ) ;
#40197 = CARTESIAN_POINT ( 'NONE',  ( 114.0246765045248196, -7.250697342233347165, -19.15521520033831138 ) ) ;
#40198 = EDGE_CURVE ( 'NONE', #12976, #40373, #23870, .T. ) ;
#40199 = CARTESIAN_POINT ( 'NONE',  ( 117.9016614775786280, -9.988377603198976828, -10.36322818467138340 ) ) ;
#40200 = ORIENTED_EDGE ( 'NONE', *, *, #28400, .F. ) ;
#40201 = CARTESIAN_POINT ( 'NONE',  ( 119.6034614775786196, -6.344957434206665248, -7.627207830600338134 ) ) ;
#40202 = CARTESIAN_POINT ( 'NONE',  ( 63.51630259865831363, -37.86186143294432327, -4.893262514330128710 ) ) ;
#40203 = CARTESIAN_POINT ( 'NONE',  ( 109.4407702545248355, -10.62599879583958717, -15.77991374673208469 ) ) ;
#40204 = CARTESIAN_POINT ( 'NONE',  ( 120.2841814775786276, 0.9020085738987339008, -11.91225656197089222 ) ) ;
#40205 = CARTESIAN_POINT ( 'NONE',  ( 117.3343948109119737, -3.383040157471821630, -19.15922257007629170 ) ) ;
#40206 = PLANE ( 'NONE',  #41078 ) ;
#40207 = CARTESIAN_POINT ( 'NONE',  ( 117.2294421295247844, -10.84261285664941177, -5.229271512936652933 ) ) ;
#40208 = EDGE_LOOP ( 'NONE', ( #17632, #17655 ) ) ;
#40209 = CARTESIAN_POINT ( 'NONE',  ( 128.2184548109119930, -4.863998795839242995, -13.39321520033831447 ) ) ;
#40210 = CARTESIAN_POINT ( 'NONE',  ( 109.2294347450687866, -10.29077967592130349, -14.42818681898541300 ) ) ;
#40211 = CONICAL_SURFACE ( 'NONE', #18370, 5.999999999999997335, 0.4636476090008060935 ) ;
#40212 = CARTESIAN_POINT ( 'NONE',  ( 119.2631014775786298, -9.565557343593413364, -10.61323700422348004 ) ) ;
#40214 = CARTESIAN_POINT ( 'NONE',  ( 110.0658483795247804, -8.402594152722688392, -16.93181055722141792 ) ) ;
#40213 = APPLICATION_CONTEXT ( 'automotive_design' ) ;
#40215 = CARTESIAN_POINT ( 'NONE',  ( 109.2324108795247923, -1.325403438956436419, -16.93181055722141792 ) ) ;
#40216 = CARTESIAN_POINT ( 'NONE',  ( 118.2420214775786320, -6.222761293078241884, -8.102969835052219238 ) ) ;
#40217 = CYLINDRICAL_SURFACE ( 'NONE', #25579, 10.00000000000000000 ) ;
#40218 = CARTESIAN_POINT ( 'NONE',  ( 69.63874157094764428, -25.41500789246203951, -5.785566283887345840 ) ) ;
#40219 = CARTESIAN_POINT ( 'NONE',  ( 113.8173414775786512, -9.565557343593413364, -10.61323700422348004 ) ) ;
#40220 = CARTESIAN_POINT ( 'NONE',  ( 122.0994348109119443, 0.9020085738987339008, -11.91225656197089222 ) ) ;
#40221 = VERTEX_POINT ( 'NONE', #40196 ) ;
#40222 = CARTESIAN_POINT ( 'NONE',  ( 122.1561614775786353, -8.899110576539710493, -16.42337572283490132 ) ) ;
#40223 = CONICAL_SURFACE ( 'NONE', #33651, 2.000000000000000444, 0.9599310885968830309 ) ;
#40224 = CARTESIAN_POINT ( 'NONE',  ( 114.3278814775786429, -10.30919188438810075, -12.61870101168855918 ) ) ;
#40225 = CARTESIAN_POINT ( 'NONE',  ( 121.9292548109119849, -1.561330072975668948, -17.79121239304076951 ) ) ;
#40226 = CARTESIAN_POINT ( 'NONE',  ( 122.2696148109119889, -5.574606645277164318, -18.38911715685844683 ) ) ;
#40227 = ORIENTED_EDGE ( 'NONE', *, *, #8365, .T. ) ;
#40228 = CARTESIAN_POINT ( 'NONE',  ( 123.2906948109119867, -1.833838273342659697, -17.42832698103878286 ) ) ;
#40229 = CARTESIAN_POINT ( 'NONE',  ( 124.6521348109119884, -1.561330072975668948, -17.79121239304076951 ) ) ;
#40230 = CARTESIAN_POINT ( 'NONE',  ( 72.54180985774836188, -55.08604862764417476, -34.50806356816917742 ) ) ;
#40231 = B_SPLINE_CURVE_WITH_KNOTS ( 'NONE', 3,
 ( #30499, #6333, #37331, #5868, #19791, #37564, #33674, #12962 ),
 .UNSPECIFIED., .F., .F.,
 ( 4, 2, 2, 4 ),
 ( 0.000000000000000000, 0.2499999999999996669, 0.4999999999999993339, 1.000000000000000000 ),
 .UNSPECIFIED. ) ;
#40232 = CARTESIAN_POINT ( 'NONE',  ( 126.1837548109119211, -10.63000616557722466, -14.87417383870573495 ) ) ;
#40233 = CARTESIAN_POINT ( 'NONE',  ( 106.0375671295248310, -10.62599879583958540, -13.39321520033831447 ) ) ;
#40234 = CARTESIAN_POINT ( 'NONE',  ( 87.41631446019775353, -25.99489077589524300, -13.39321520033831625 ) ) ;
#40235 = DIRECTION ( 'NONE',  ( -0.7871354856660202071, 0.6167752151498580027, 0.002461946824133919541 ) ) ;
#40236 = CARTESIAN_POINT ( 'NONE',  ( 109.7185827545247889, -6.936859964151250502, -8.388885654883777576 ) ) ;
#40237 = CARTESIAN_POINT ( 'NONE',  ( 59.24641515291911986, -13.72835195454734425, -7.393215200338315363 ) ) ;
#40238 = DIRECTION ( 'NONE',  ( 0.000000000000000000, 0.000000000000000000, -1.000000000000000000 ) ) ;
#40239 = CARTESIAN_POINT ( 'NONE',  ( 120.5678148109119832, -1.833838273342659253, -17.42832698103878286 ) ) ;
#40240 = CARTESIAN_POINT ( 'NONE',  ( 126.2404814775786264, -9.261995988541697145, -16.69588392320189030 ) ) ;
#40241 = CARTESIAN_POINT ( 'NONE',  ( 126.9733055311670284, -0.02945601996773287642, -11.03864623346424523 ) ) ;
#40242 = VERTEX_POINT ( 'NONE', #32880 ) ;
#40243 = CARTESIAN_POINT ( 'NONE',  ( 116.4555358795247884, -8.402594152722688392, -9.854619843455216355 ) ) ;
#40244 = CARTESIAN_POINT ( 'NONE',  ( 108.1211608795247798, -1.325403438956436419, -16.93181055722141792 ) ) ;
#40245 = EDGE_LOOP ( 'NONE', ( #42705, #8199, #16840, #24088, #13776, #15446 ) ) ;
#40246 = CARTESIAN_POINT ( 'NONE',  ( 117.7882081442453170, -3.505236298600246325, -18.68346056562440793 ) ) ;
#40247 = CYLINDRICAL_SURFACE ( 'NONE', #31142, 1.499999999999996225 ) ;
#40248 = CONICAL_SURFACE ( 'NONE', #20611, 1.610000000000000986, 0.9599310885968765916 ) ;
#40249 = CARTESIAN_POINT ( 'NONE',  ( 61.69189222814998175, -61.90644496644519990, -36.30514255143466329 ) ) ;
#40250 = DIRECTION ( 'NONE',  ( -0.000000000000000000, -0.9284778069183721172, -0.3713878862591650232 ) ) ;
#40252 = CARTESIAN_POINT ( 'NONE',  ( 122.8368814775786291, -1.561330072975668948, -17.79121239304076951 ) ) ;
#40251 = CARTESIAN_POINT ( 'NONE',  ( 89.78938736644981589, -26.75858941326842810, -11.54476601486570964 ) ) ;
#40253 = EDGE_CURVE ( 'NONE', #9298, #22284, #35854, .T. ) ;
#40254 = CARTESIAN_POINT ( 'NONE',  ( 121.1350814775786233, -9.859900752359378018, -12.68260735090039759 ) ) ;
#40255 = ORIENTED_EDGE ( 'NONE', *, *, #33228, .T. ) ;
#40256 = PLANE ( 'NONE',  #25865 ) ;
#40257 = CARTESIAN_POINT ( 'NONE',  ( 66.27224413149734517, -14.92707987627686350, -10.39321520033831803 ) ) ;
#40258 = CARTESIAN_POINT ( 'NONE',  ( 108.9545983795247821, -8.402594152722688392, -16.93181055722141792 ) ) ;
#40259 = CARTESIAN_POINT ( 'NONE',  ( 120.1707281442453166, -9.565557343593413364, -10.61323700422348004 ) ) ;
#40260 = CARTESIAN_POINT ( 'NONE',  ( 118.8092881442453290, -0.1624402480850797581, -16.17319339645315424 ) ) ;
#40261 = CARTESIAN_POINT ( 'NONE',  ( 119.5633519737025523, -1.196538596002817867, -17.02799684832028504 ) ) ;
#40262 = CARTESIAN_POINT ( 'NONE',  ( 115.9693640045247776, 0.1403307496149616695, -15.46607636864997204 ) ) ;
#40263 = CARTESIAN_POINT ( 'NONE',  ( 116.7104014775786425, -0.4660016031367729128, -10.09054647747476174 ) ) ;
#40264 = DIRECTION ( 'NONE',  ( 0.000000000000000000, 0.3818493186865927203, -0.9242245927363029745 ) ) ;
#40265 = DIRECTION ( 'NONE',  ( -0.000000000000000000, -0.9242245927363028635, -0.3818493186865929423 ) ) ;
#40266 = CARTESIAN_POINT ( 'NONE',  ( 110.2742077545248094, -7.250697342233347165, -7.631215200338321125 ) ) ;
#40267 = CARTESIAN_POINT ( 'NONE',  ( 88.73939138327467901, -25.99489077589524300, -13.39321520033831625 ) ) ;
#40268 = CARTESIAN_POINT ( 'NONE',  ( 114.8581140045248361, -10.62599879583958717, -11.00651665394454604 ) ) ;
#40269 = CARTESIAN_POINT ( 'NONE',  ( 120.0572748109119772, -3.383040157471821630, -19.15922257007629170 ) ) ;
#40270 = CARTESIAN_POINT ( 'NONE',  ( 122.0427081442452817, 0.5811942927096110934, -14.16772938898807510 ) ) ;
#40271 = FACE_OUTER_BOUND ( 'NONE', #43057, .T. ) ;
#40272 = CARTESIAN_POINT ( 'NONE',  ( 115.1220548109119761, -8.166667518702817929, -8.995218007635861213 ) ) ;
#40273 = DIRECTION ( 'NONE',  ( 0.000000000000000000, -0.3713878862591665220, 0.9284778069183713400 ) ) ;
#40274 = EDGE_LOOP ( 'NONE', ( #2919, #40101, #22885, #14207 ) ) ;
#40275 = CARTESIAN_POINT ( 'NONE',  ( 109.2294421295247844, 0.2400687412228638684, -12.14321520033831625 ) ) ;
#40276 = VECTOR ( 'NONE', #27378, 1000.000000000000114 ) ;
#40277 = CARTESIAN_POINT ( 'NONE',  ( 123.8012348109119642, 0.2603800115204892296, -16.42320221600525088 ) ) ;
#40278 = AXIS2_PLACEMENT_3D ( 'NONE', #41406, #30448, #17226 ) ;
#40279 = CARTESIAN_POINT ( 'NONE',  ( 121.5888948109119809, -10.30919188438810075, -12.61870101168855918 ) ) ;
#40280 = CARTESIAN_POINT ( 'NONE',  ( 124.8790414775786246, -8.899110576539710493, -16.42337572283490132 ) ) ;
#40281 = APPLICATION_PROTOCOL_DEFINITION ( 'draft international standard', 'automotive_design', 1998, #33198 ) ;
#40282 = CARTESIAN_POINT ( 'NONE',  ( 112.9664414775786412, -9.859900752359374465, -12.68260735090039404 ) ) ;
#40283 = CARTESIAN_POINT ( 'NONE',  ( 115.6325948109119821, -9.565557343593413364, -10.61323700422348004 ) ) ;
#40284 = CARTESIAN_POINT ( 'NONE',  ( 125.7866681442452688, -0.4660016031367893996, -10.09054647747474043 ) ) ;
#40285 = CARTESIAN_POINT ( 'NONE',  ( 123.6310548109119765, -5.638512984488999180, -18.83840828888717311 ) ) ;
#40286 = CARTESIAN_POINT ( 'NONE',  ( 110.6909265045248247, -7.250697342233347165, -19.15521520033831138 ) ) ;
#40287 = CIRCLE ( 'NONE', #7527, 2.999999999999999556 ) ;
#40288 = CARTESIAN_POINT ( 'NONE',  ( 120.3976348109119812, -7.643976991954077427, -18.09477374809248928 ) ) ;
#40289 = CARTESIAN_POINT ( 'NONE',  ( 116.7891407172877791, -3.223887174354909568, -18.32229490764988000 ) ) ;
#40290 = DIRECTION ( 'NONE',  ( 0.000000000000000000, 0.000000000000000000, -1.000000000000000000 ) ) ;
#40291 = ORIENTED_EDGE ( 'NONE', *, *, #36224, .T. ) ;
#40292 = DIRECTION ( 'NONE',  ( 0.5040994586965589219, 0.8636456077245088236, 0.000000000000000000 ) ) ;
#40293 = CARTESIAN_POINT ( 'NONE',  ( 122.6099748109119929, -9.261995988541697145, -16.69588392320189030 ) ) ;
#40294 = CARTESIAN_POINT ( 'NONE',  ( 70.19189222814998175, -61.90193818873174791, -37.96356864969668266 ) ) ;
#40295 = CARTESIAN_POINT ( 'NONE',  ( 125.0660727672600956, 2.552004055856275322, -12.19903144353943603 ) ) ;
#40296 = DIRECTION ( 'NONE',  ( 0.000000000000000000, 1.000000000000000000, 0.000000000000000000 ) ) ;
#40297 = CARTESIAN_POINT ( 'NONE',  ( 67.57613997102261294, -0.2549909087870869118, -16.39321520033831447 ) ) ;
#40298 = DIRECTION ( 'NONE',  ( 0.9609149988134843001, -0.1028163501681632064, 0.2570431154366505933 ) ) ;
#40299 = CARTESIAN_POINT ( 'NONE',  ( 122.8936081442453059, -9.565557343593413364, -10.61323700422348004 ) ) ;
#40300 = CARTESIAN_POINT ( 'NONE',  ( 123.5288836215688235, -1.135392229370316919, -17.10942237759952533 ) ) ;
#40301 = CARTESIAN_POINT ( 'NONE',  ( 123.9714148109119805, -8.899110576539710493, -16.42337572283490132 ) ) ;
#40302 = CONICAL_SURFACE ( 'NONE', #43928, 2.000000000000000444, 0.9599310885968830309 ) ;
#40303 = CARTESIAN_POINT ( 'NONE',  ( 124.2749441479622021, -11.95494744398080655, -17.02855821661913183 ) ) ;
#40304 = CARTESIAN_POINT ( 'NONE',  ( 124.9924948109119924, -4.089484607189486809, -7.948022111789456723 ) ) ;
#40305 = CARTESIAN_POINT ( 'NONE',  ( 119.3765548109119834, -10.15424416112533912, -14.75197769757731336 ) ) ;
#40306 = CARTESIAN_POINT ( 'NONE',  ( 62.22678445075433018, -36.72958069525633817, -5.531797115907686191 ) ) ;
#40307 = ORIENTED_EDGE ( 'NONE', *, *, #37017, .T. ) ;
#40308 = CARTESIAN_POINT ( 'NONE',  ( 122.3830681442452857, -8.166667518702819706, -8.995218007635861213 ) ) ;
#40309 = CARTESIAN_POINT ( 'NONE',  ( 116.6536748109119941, 0.9020085738987339008, -11.91225656197089222 ) ) ;
#40310 = CARTESIAN_POINT ( 'NONE',  ( 116.8028015045247940, -6.936859964151250502, -18.39754474579286025 ) ) ;
#40311 = CARTESIAN_POINT ( 'NONE',  ( 112.9097148109120070, -9.565557343593413364, -10.61323700422348004 ) ) ;
#40312 = CARTESIAN_POINT ( 'NONE',  ( 124.1983214775786166, -1.833838273342659697, -17.42832698103878286 ) ) ;
#40313 = CARTESIAN_POINT ( 'NONE',  ( 122.6099748109119929, -9.261995988541697145, -16.69588392320189030 ) ) ;
#40314 = CARTESIAN_POINT ( 'NONE',  ( 115.9693640045247776, -10.62599879583958717, -11.00651665394454604 ) ) ;
#40315 = CARTESIAN_POINT ( 'NONE',  ( 110.5520202545248054, 0.1403307496149616695, -11.32035403202665336 ) ) ;
#40316 = CARTESIAN_POINT ( 'NONE',  ( 84.49707967414211396, -25.99489077589524300, -13.39321520033831625 ) ) ;
#40317 = AXIS2_PLACEMENT_3D ( 'NONE', #23472, #43766, #9103 ) ;
#40318 = CARTESIAN_POINT ( 'NONE',  ( 113.8173414775786512, -9.565557343593413364, -10.61323700422348004 ) ) ;
#40319 = CARTESIAN_POINT ( 'NONE',  ( 117.2209414775786485, -2.084020599724406786, -8.691656652584148546 ) ) ;
#40320 = CARTESIAN_POINT ( 'NONE',  ( 89.78938736644981589, -25.99489077589524300, -13.39321520033831625 ) ) ;
#40321 = CARTESIAN_POINT ( 'NONE',  ( 111.5243640045248412, 0.1403307496149616695, -15.46607636864997204 ) ) ;
#40322 = VERTEX_POINT ( 'NONE', #36085 ) ;
#40323 = CARTESIAN_POINT ( 'NONE',  ( 125.1626748109119802, -0.1624402480850797581, -16.17319339645315424 ) ) ;
#40324 = CARTESIAN_POINT ( 'NONE',  ( 120.2296266859119953, -9.033780868592240054, -16.85052413769862056 ) ) ;
#40325 = CARTESIAN_POINT ( 'NONE',  ( 121.8965016859119856, -9.665098340737509730, -17.37397104707595474 ) ) ;
#40326 = VERTEX_POINT ( 'NONE', #36534 ) ;
#40327 = DIRECTION ( 'NONE',  ( -0.9970811988817437355, 0.07634843047859309062, -9.125038414728249219E-18 ) ) ;
#40328 = CARTESIAN_POINT ( 'NONE',  ( 116.8800879763089995, -11.65005305785124712, -21.48974400451860234 ) ) ;
#40329 = VERTEX_POINT ( 'NONE', #8287 ) ;
#40330 = CARTESIAN_POINT ( 'NONE',  ( 118.1285681442453068, -7.893985811506177619, -18.51759400769804742 ) ) ;
#40331 = CARTESIAN_POINT ( 'NONE',  ( 124.7655881442452852, -9.859900752359378018, -12.68260735090039759 ) ) ;
#40332 = CARTESIAN_POINT ( 'NONE',  ( 114.5547881442453217, -4.153390946401321671, -8.397313243818183892 ) ) ;
#40333 = PLANE ( 'NONE',  #909 ) ;
#40334 = CARTESIAN_POINT ( 'NONE',  ( 117.2294421295247844, 0.2335149919452661482, -4.893215200338314474 ) ) ;
#40335 = CARTESIAN_POINT ( 'NONE',  ( 114.3278814775786429, -10.30919188438810075, -12.61870101168855918 ) ) ;
#40336 = AXIS2_PLACEMENT_3D ( 'NONE', #44063, #40870, #23304 ) ;
#40337 = CARTESIAN_POINT ( 'NONE',  ( 111.5938171295247940, 0.1403307496149613920, -13.39321520033831447 ) ) ;
#40338 = CARTESIAN_POINT ( 'NONE',  ( 125.6164881442453094, 0.2603800115204892296, -16.42320221600525088 ) ) ;
#40339 = CYLINDRICAL_SURFACE ( 'NONE', #21381, 1.999999999999998890 ) ;
#40340 = ORIENTED_EDGE ( 'NONE', *, *, #38994, .T. ) ;
#40341 = EDGE_CURVE ( 'NONE', #2587, #24723, #21659, .T. ) ;
#40342 = CARTESIAN_POINT ( 'NONE',  ( 114.4413348109119823, -9.261995988541697145, -16.69588392320189030 ) ) ;
#40343 = ADVANCED_FACE ( 'NONE', ( #32217 ), #12007, .T. ) ;
#40344 = EDGE_CURVE ( 'NONE', #21214, #14508, #25313, .T. ) ;
#40345 = CARTESIAN_POINT ( 'NONE',  ( 113.3635281442453504, -0.1624402480850797581, -16.17319339645315424 ) ) ;
#40346 = CARTESIAN_POINT ( 'NONE',  ( 126.5254139958929045, -4.932287615856277618, -18.54625524651014956 ) ) ;
#40347 = CARTESIAN_POINT ( 'NONE',  ( 113.1933481442453058, -4.089484607189486809, -7.948022111789456723 ) ) ;
#40348 = EDGE_LOOP ( 'NONE', ( #15109, #33240, #34015, #11650 ) ) ;
#40349 = CARTESIAN_POINT ( 'NONE',  ( 122.9503348109119827, 0.5811942927096110934, -14.16772938898807510 ) ) ;
#40350 = DIRECTION ( 'NONE',  ( 1.000000000000000000, 0.000000000000000000, 0.000000000000000000 ) ) ;
#40351 = DIRECTION ( 'NONE',  ( 0.000000000000000000, 0.000000000000000000, -1.000000000000000000 ) ) ;
#40352 = CARTESIAN_POINT ( 'NONE',  ( 73.07463722459043254, -57.56799820464436834, -35.33549987209089238 ) ) ;
#40353 = CARTESIAN_POINT ( 'NONE',  ( 112.4567343740715870, -2.419733177069674834, -17.89711025544712086 ) ) ;
#40354 = CARTESIAN_POINT ( 'NONE',  ( 115.8595014775786609, -7.643976991954077427, -18.09477374809248928 ) ) ;
#40355 = LINE ( 'NONE', #19832, #27012 ) ;
#40356 = CARTESIAN_POINT ( 'NONE',  ( 125.3290191022591529, -2.376857512254589189, -20.05354607378702525 ) ) ;
#40357 = CARTESIAN_POINT ( 'NONE',  ( 113.1933481442453058, -5.574606645277164318, -18.38911715685844683 ) ) ;
#40358 = CARTESIAN_POINT ( 'NONE',  ( 113.7606148109119886, -1.561330072975668060, -17.79121239304076596 ) ) ;
#40359 = CARTESIAN_POINT ( 'NONE',  ( 121.6881423109119709, -0.4387604401700512802, -15.73000352943951619 ) ) ;
#40360 = CARTESIAN_POINT ( 'NONE',  ( 126.0703014775786102, -0.1624402480850797581, -16.17319339645315424 ) ) ;
#40361 = CARTESIAN_POINT ( 'NONE',  ( 114.8384214775786489, -10.15424416112533912, -14.75197769757731336 ) ) ;
#40362 = CARTESIAN_POINT ( 'NONE',  ( 124.7088614775786226, 0.2603800115204892296, -16.42320221600525088 ) ) ;
#40363 = CIRCLE ( 'NONE', #23648, 5.952500000000000568 ) ;
#40364 = CARTESIAN_POINT ( 'NONE',  ( 121.5321681442453183, -9.988377603198976828, -10.36322818467138340 ) ) ;
#40365 = ORIENTED_EDGE ( 'NONE', *, *, #341, .F. ) ;
#40366 = CARTESIAN_POINT ( 'NONE',  ( 113.0798948109119948, -0.4660016031367893996, -10.09054647747474043 ) ) ;
#40367 = CARTESIAN_POINT ( 'NONE',  ( 113.5385046295247804, -4.863998795839590272, -7.631215200338315796 ) ) ;
#40368 = EDGE_CURVE ( 'NONE', #39689, #6914, #2366, .T. ) ;
#40369 = CARTESIAN_POINT ( 'NONE',  ( 108.0517077545248696, -2.791137627527939813, -18.39754474579286025 ) ) ;
#40370 = CARTESIAN_POINT ( 'NONE',  ( 110.6214733795247867, -1.325403438956436419, -9.854619843455211026 ) ) ;
#40371 = CARTESIAN_POINT ( 'NONE',  ( 64.33868347142437472, -36.47288101306110519, -5.626337088425048982 ) ) ;
#40372 = CARTESIAN_POINT ( 'NONE',  ( 117.1074881442453233, -10.63000616557722466, -14.87417383870573495 ) ) ;
#40373 = VERTEX_POINT ( 'NONE', #5345 ) ;
#40374 = LINE ( 'NONE', #9137, #17292 ) ;
#40375 = CARTESIAN_POINT ( 'NONE',  ( 124.2193060444391790, -1.267766418764731728, -16.93314635290706605 ) ) ;
#40376 = CARTESIAN_POINT ( 'NONE',  ( 120.8557914811013347, -2.280480477428469488, -18.08254604495227014 ) ) ;
#40377 = CARTESIAN_POINT ( 'NONE',  ( 115.4624148109119943, -4.153390946401321671, -8.397313243818183892 ) ) ;
#40378 = EDGE_CURVE ( 'NONE', #6291, #40322, #32093, .T. ) ;
#40379 = CARTESIAN_POINT ( 'NONE',  ( 105.2041296295248287, -4.863998795839590272, -8.388885654883775800 ) ) ;
#40380 = CARTESIAN_POINT ( 'NONE',  ( 121.5321681442453183, -9.988377603198976828, -10.36322818467138340 ) ) ;
#40381 = ADVANCED_FACE ( 'NONE', ( #37479 ), #31531, .F. ) ;
#40382 = CARTESIAN_POINT ( 'NONE',  ( 108.1906140045248463, -10.62599879583958717, -11.00651665394454604 ) ) ;
#40383 = FACE_OUTER_BOUND ( 'NONE', #23596, .T. ) ;
#40384 = VERTEX_POINT ( 'NONE', #34057 ) ;
#40385 = FACE_BOUND ( 'NONE', #12596, .T. ) ;
#40386 = CARTESIAN_POINT ( 'NONE',  ( 122.4397948109119767, -0.1624402480850797581, -16.17319339645315424 ) ) ;
#40387 = CARTESIAN_POINT ( 'NONE',  ( 120.6812681442452941, -10.30919188438810075, -12.61870101168855918 ) ) ;
#40388 = CARTESIAN_POINT ( 'NONE',  ( 113.7038881442453402, -6.222761293078241884, -8.102969835052219238 ) ) ;
#40389 = CARTESIAN_POINT ( 'NONE',  ( 114.5547881442453217, -5.638512984488999180, -18.83840828888717311 ) ) ;
#40390 = CARTESIAN_POINT ( 'NONE',  ( 136.3817460758107813, -7.085787385089622248, -18.75052711434078390 ) ) ;
#40391 = CARTESIAN_POINT ( 'NONE',  ( 124.6521348109119884, -7.894159318335828068, -9.358103419637847864 ) ) ;
#40392 = CARTESIAN_POINT ( 'NONE',  ( 118.4122014775786340, -9.859900752359374465, -12.68260735090039404 ) ) ;
#40393 = EDGE_LOOP ( 'NONE', ( #28758, #2064 ) ) ;
#40394 = AXIS2_PLACEMENT_3D ( 'NONE', #30256, #40753, #23427 ) ;
#40395 = CARTESIAN_POINT ( 'NONE',  ( 122.2437673109119629, 0.2312338769422704887, -16.08380026872395874 ) ) ;
#40396 = CARTESIAN_POINT ( 'NONE',  ( 112.6260814775786514, -9.261995988541697145, -16.69588392320189030 ) ) ;
#40397 = CARTESIAN_POINT ( 'NONE',  ( 121.4187148109119789, -3.505236298600246325, -18.68346056562440793 ) ) ;
#40398 = ORIENTED_EDGE ( 'NONE', *, *, #28135, .T. ) ;
#40399 = EDGE_CURVE ( 'NONE', #27626, #22908, #302, .T. ) ;
#40400 = CARTESIAN_POINT ( 'NONE',  ( 122.1743141859119817, -8.321307733199551748, -9.223433127585318303 ) ) ;
#40401 = ADVANCED_FACE ( 'NONE', ( #41599 ), #2824, .F. ) ;
#40402 = EDGE_CURVE ( 'NONE', #38575, #38752, #7108, .T. ) ;
#40403 = CARTESIAN_POINT ( 'NONE',  ( 117.2209414775786485, -7.893985811506177619, -18.51759400769804742 ) ) ;
#40404 = CIRCLE ( 'NONE', #42581, 2.000000000000000444 ) ;
#40405 = CARTESIAN_POINT ( 'NONE',  ( 111.4549108795247747, -8.938348069036489818, -9.318865927141430916 ) ) ;
#40406 = CARTESIAN_POINT ( 'NONE',  ( 116.6536748109119941, -10.15424416112533912, -14.75197769757731336 ) ) ;
#40407 = VERTEX_POINT ( 'NONE', #6927 ) ;
#40408 = ORIENTED_EDGE ( 'NONE', *, *, #6377, .T. ) ;
#40409 = CARTESIAN_POINT ( 'NONE',  ( 124.1983214775786166, -1.833838273342659697, -17.42832698103878286 ) ) ;
#40410 = B_SPLINE_CURVE_WITH_KNOTS ( 'NONE', 3,
 ( #41509, #13466, #6614, #31219 ),
 .UNSPECIFIED., .F., .F.,
 ( 4, 4 ),
 ( 0.01196303694811591892, 0.01338272309942444005 ),
 .UNSPECIFIED. ) ;
#40411 = CARTESIAN_POINT ( 'NONE',  ( 120.2841814775786276, -10.15424416112533912, -14.75197769757731336 ) ) ;
#40412 = CARTESIAN_POINT ( 'NONE',  ( 65.41257106814472877, -15.47412461924279725, -16.39321520033831447 ) ) ;
#40413 = CARTESIAN_POINT ( 'NONE',  ( 70.19189222814998175, -58.90901798090458641, -36.76641099935233825 ) ) ;
#40414 = CARTESIAN_POINT ( 'NONE',  ( 119.7169148109119874, -9.988377603198976828, -10.36322818467138340 ) ) ;
#40415 = CARTESIAN_POINT ( 'NONE',  ( 84.39081516114413262, -30.32262605124143562, -18.39321520033831803 ) ) ;
#40416 = CARTESIAN_POINT ( 'NONE',  ( 116.9940348109119839, -9.988377603198976828, -10.36322818467138340 ) ) ;
#40418 = CARTESIAN_POINT ( 'NONE',  ( 115.4624148109119943, -4.153390946401321671, -8.397313243818183892 ) ) ;
#40417 = CARTESIAN_POINT ( 'NONE',  ( 116.8238548109119819, -4.089484607189486809, -7.948022111789456723 ) ) ;
#40419 =( BOUNDED_CURVE ( )  B_SPLINE_CURVE ( 3, ( #24075, #27270, #17013, #2626 ),
 .UNSPECIFIED., .F., .F. ) 
 B_SPLINE_CURVE_WITH_KNOTS ( ( 4, 4 ),
 ( 1.570796326794895004, 2.115579167352664935 ),
 .UNSPECIFIED. ) 
 CURVE ( )  GEOMETRIC_REPRESENTATION_ITEM ( )  RATIONAL_B_SPLINE_CURVE ( ( 1.000000000000000000, 0.9754201827720950790, 0.9754201827720950790, 1.000000000000000000 ) ) 
 REPRESENTATION_ITEM ( '' )  );
#40420 = CARTESIAN_POINT ( 'NONE',  ( 124.0848681442452772, -5.574606645277164318, -18.38911715685844683 ) ) ;
#40421 = CARTESIAN_POINT ( 'NONE',  ( 112.1722681442453222, -0.4660016031367893996, -10.09054647747474043 ) ) ;
#40422 = ORIENTED_EDGE ( 'NONE', *, *, #9793, .F. ) ;
#40423 = CARTESIAN_POINT ( 'NONE',  ( 123.9714148109119805, -8.899110576539710493, -16.42337572283490132 ) ) ;
#40424 = CARTESIAN_POINT ( 'NONE',  ( 122.2076758011493922, -1.149058757900107697, -17.09122335155391781 ) ) ;
#40425 = CARTESIAN_POINT ( 'NONE',  ( 70.19189222814998175, -70.61873396092025246, -41.45025657337532010 ) ) ;
#40426 = MECHANICAL_DESIGN_GEOMETRIC_PRESENTATION_REPRESENTATION (  '', ( #30201 ), #9109 ) ;
#40427 = CARTESIAN_POINT ( 'NONE',  ( 114.1635827545248389, -2.477300249445798297, -19.15521520033831138 ) ) ;
#40428 = CARTESIAN_POINT ( 'NONE',  ( 112.2188952545247531, -9.868328341294098749, -15.46607636864997204 ) ) ;
#40429 = CARTESIAN_POINT ( 'NONE',  ( 109.8574890045247940, 0.8980012041604421569, -15.77991374673208469 ) ) ;
#40430 = CARTESIAN_POINT ( 'NONE',  ( 118.8660148109119774, -10.30919188438810075, -12.61870101168855918 ) ) ;
#40431 = EDGE_LOOP ( 'NONE', ( #5656, #26206, #22170, #20150, #3433 ) ) ;
#40432 = CARTESIAN_POINT ( 'NONE',  ( 119.0929214775786278, -5.638512984488999180, -18.83840828888717311 ) ) ;
#40433 = CARTESIAN_POINT ( 'NONE',  ( 112.8529881442453302, -7.894159318335828068, -9.358103419637847864 ) ) ;
#40434 = CARTESIAN_POINT ( 'NONE',  ( 108.1211608795247798, -8.938348069036489818, -9.318865927141430916 ) ) ;
#40435 = CARTESIAN_POINT ( 'NONE',  ( 120.6812681442452941, -10.30919188438810075, -12.61870101168855918 ) ) ;
#40436 = CARTESIAN_POINT ( 'NONE',  ( 121.9859814775786333, 0.2603800115204892296, -16.42320221600525088 ) ) ;
#40437 = CARTESIAN_POINT ( 'NONE',  ( 62.61908855860606593, -3.462305083068016209, -19.20062954177708647 ) ) ;
#40438 = DIRECTION ( 'NONE',  ( 0.000000000000000000, 0.000000000000000000, 1.000000000000000000 ) ) ;
#40439 = CARTESIAN_POINT ( 'NONE',  ( 119.3961891859119930, -1.406689858478933353, -17.56299727309130887 ) ) ;
#40440 = ORIENTED_EDGE ( 'NONE', *, *, #41214, .F. ) ;
#40441 = CARTESIAN_POINT ( 'NONE',  ( -2.989272046485941914, -7.181056780202320411, -7.392714882508171215 ) ) ;
#40442 = DIRECTION ( 'NONE',  ( 0.000000000000000000, -0.3818493186865936084, 0.9242245927363024194 ) ) ;
#40443 = CARTESIAN_POINT ( 'NONE',  ( 122.7801548109119665, -6.222761293078241884, -8.102969835052219238 ) ) ;
#40444 = CARTESIAN_POINT ( 'NONE',  ( 116.5249890045247980, 0.8980012041604421569, -15.77991374673208469 ) ) ;
#40445 = CARTESIAN_POINT ( 'NONE',  ( 109.4407702545248355, 0.1403307496149616695, -11.32035403202665336 ) ) ;
#40446 = CARTESIAN_POINT ( 'NONE',  ( 116.9373081442452929, -1.833838273342659253, -17.42832698103878286 ) ) ;
#40447 = CARTESIAN_POINT ( 'NONE',  ( 84.49707967414211396, -25.99489077589524300, -13.39321520033831625 ) ) ;
#40448 = CARTESIAN_POINT ( 'NONE',  ( 68.96140303619711176, -25.88415598586878730, -5.893215200338315363 ) ) ;
#40449 = CARTESIAN_POINT ( 'NONE',  ( 112.3991748109119868, -1.833838273342658809, -17.42832698103878286 ) ) ;
#40450 = CARTESIAN_POINT ( 'NONE',  ( 122.0427081442452817, 0.5811942927096110934, -14.16772938898807510 ) ) ;
#40452 = VERTEX_POINT ( 'NONE', #6482 ) ;
#40451 = EDGE_CURVE ( 'NONE', #13784, #45010, #44271, .T. ) ;
#40453 = CARTESIAN_POINT ( 'NONE',  ( 122.7234281442452755, -4.153390946401325223, -8.397313243818185668 ) ) ;
#40454 = CARTESIAN_POINT ( 'NONE',  ( 113.7038881442453402, -3.383040157471821630, -19.15922257007629170 ) ) ;
#40455 = CARTESIAN_POINT ( 'NONE',  ( 122.6667014775786413, -7.893985811506177619, -18.51759400769804742 ) ) ;
#40456 = CARTESIAN_POINT ( 'NONE',  ( 122.2128881442453263, -7.643976991954077427, -18.09477374809248928 ) ) ;
#40457 = EDGE_LOOP ( 'NONE', ( #28580, #3874, #15329, #2387, #1002, #22399 ) ) ;
#40458 = FACE_OUTER_BOUND ( 'NONE', #40431, .T. ) ;
#40459 = VECTOR ( 'NONE', #9007, 1000.000000000000114 ) ;
#40460 = CARTESIAN_POINT ( 'NONE',  ( 125.1059481442452750, -8.166667518702819706, -8.995218007635861213 ) ) ;
#40461 = ADVANCED_FACE ( 'NONE', ( #13992 ), #17197, .T. ) ;
#40462 = CARTESIAN_POINT ( 'NONE',  ( 113.3635281442453504, -0.1624402480850797581, -16.17319339645315424 ) ) ;
#40463 = CARTESIAN_POINT ( 'NONE',  ( 123.7445081442452874, -1.561330072975668948, -17.79121239304076951 ) ) ;
#40464 = EDGE_CURVE ( 'NONE', #35202, #25805, #10137, .T. ) ;
#40465 = CARTESIAN_POINT ( 'NONE',  ( 106.2459265045248173, -7.250697342233347165, -19.15521520033831138 ) ) ;
#40466 = AXIS2_PLACEMENT_3D ( 'NONE', #44398, #17464, #13162 ) ;
#40467 = CARTESIAN_POINT ( 'NONE',  ( 120.9936110609119737, -6.340755971794695078, -8.611740276972781771 ) ) ;
#40468 = ORIENTED_EDGE ( 'NONE', *, *, #24542, .T. ) ;
#40469 = CARTESIAN_POINT ( 'NONE',  ( 87.44708369096657918, -29.99489077589588959, -18.39321520033831803 ) ) ;
#40470 = CARTESIAN_POINT ( 'NONE',  ( 108.3295202545248657, 0.1403307496149616695, -11.32035403202665336 ) ) ;
#40471 = CARTESIAN_POINT ( 'NONE',  ( 59.36680634945872725, -12.84644995903807896, -19.39321520033831447 ) ) ;
#40472 = CARTESIAN_POINT ( 'NONE',  ( 119.9438214775786378, -2.084020599724406786, -8.691656652584148546 ) ) ;
#40473 = CARTESIAN_POINT ( 'NONE',  ( 114.8951481442453115, -8.899110576539710493, -16.42337572283490132 ) ) ;
#40474 = CARTESIAN_POINT ( 'NONE',  ( 125.4463081442452932, -4.153390946401321671, -8.397313243818183892 ) ) ;
#40475 = ORIENTED_EDGE ( 'NONE', *, *, #31425, .F. ) ;
#40476 = CARTESIAN_POINT ( 'NONE',  ( 116.8059765045247502, -6.935066607705044461, -18.39321520033830737 ) ) ;
#40477 = CARTESIAN_POINT ( 'NONE',  ( 115.4624148109119943, -4.153390946401321671, -8.397313243818183892 ) ) ;
#40478 = CARTESIAN_POINT ( 'NONE',  ( 113.5904348109119866, -2.084020599724406786, -8.691656652584148546 ) ) ;
#40479 = B_SPLINE_CURVE_WITH_KNOTS ( 'NONE', 3,
 ( #14519, #32289, #35008, #39365, #35700, #28659, #13470, #4018, #3790, #17716 ),
 .UNSPECIFIED., .F., .F.,
 ( 4, 3, 3, 4 ),
 ( 0.000000000000000000, 0.0002476487219222729902, 0.0004952974148303419637, 0.0009534114850261800637 ),
 .UNSPECIFIED. ) ;
#40480 = CARTESIAN_POINT ( 'NONE',  ( 67.63289214294319152, -0.2818690679646981834, -10.39321520033831625 ) ) ;
#40481 = CARTESIAN_POINT ( 'NONE',  ( 112.0020881442453344, -9.565557343593413364, -10.61323700422348004 ) ) ;
#40483 = CARTESIAN_POINT ( 'NONE',  ( 121.5321681442453183, -9.988377603198976828, -10.36322818467138340 ) ) ;
#40482 = DIRECTION ( 'NONE',  ( -0.4225728684367169308, 0.9063289528979889820, 0.000000000000000000 ) ) ;
#40484 = VECTOR ( 'NONE', #34526, 1000.000000000000000 ) ;
#40485 = CARTESIAN_POINT ( 'NONE',  ( 124.4252281442452812, -0.8288870151387760510, -10.36305467784173118 ) ) ;
#40486 = EDGE_LOOP ( 'NONE', ( #18664, #19651, #30565, #21933, #6852, #28766 ) ) ;
#40487 = CARTESIAN_POINT ( 'NONE',  ( 125.4584548109119737, -4.863998795839242995, -13.39321520033831447 ) ) ;
#40488 = CARTESIAN_POINT ( 'NONE',  ( 65.62759297140451054, -15.45042670135892671, -10.39321520033831803 ) ) ;
#40489 = CARTESIAN_POINT ( 'NONE',  ( 111.1076452545248259, -9.868328341294098749, -15.46607636864997204 ) ) ;
#40490 = CARTESIAN_POINT ( 'NONE',  ( 123.7445081442452874, -7.894159318335828068, -9.358103419637847864 ) ) ;
#40491 = CARTESIAN_POINT ( 'NONE',  ( 118.6958348109119754, -3.505236298600246325, -18.68346056562440793 ) ) ;
#40492 = CARTESIAN_POINT ( 'NONE',  ( 120.8060036215688484, -1.135392229370310258, -17.10942237759953244 ) ) ;
#40493 = CARTESIAN_POINT ( 'NONE',  ( 105.7597546295248350, -4.863998795839590272, -7.631215200338315796 ) ) ;
#40494 = CIRCLE ( 'NONE', #9174, 6.426280380454326924 ) ;
#40495 = CYLINDRICAL_SURFACE ( 'NONE', #11347, 1.499999999999996225 ) ;
#40496 = CARTESIAN_POINT ( 'NONE',  ( 113.1933481442453058, -5.574606645277164318, -18.38911715685844683 ) ) ;
#40497 = CARTESIAN_POINT ( 'NONE',  ( 110.5520202545248054, -10.62599879583958717, -15.77991374673208469 ) ) ;
#40498 = FACE_OUTER_BOUND ( 'NONE', #23206, .T. ) ;
#40499 = CARTESIAN_POINT ( 'NONE',  ( 115.9693640045247776, -10.62599879583958717, -11.00651665394454604 ) ) ;
#40500 = CARTESIAN_POINT ( 'NONE',  ( 120.8514481442452961, -7.893985811506177619, -18.51759400769804742 ) ) ;
#40501 = CARTESIAN_POINT ( 'NONE',  ( 120.4543614775786295, -4.089484607189486809, -7.948022111789456723 ) ) ;
#40502 = CARTESIAN_POINT ( 'NONE',  ( 111.8215301496069998, 0.3591747506842615789, -14.64321520033831447 ) ) ;
#40503 = CARTESIAN_POINT ( 'NONE',  ( 115.8027748109119841, -0.4660016031367893996, -10.09054647747474043 ) ) ;
#40504 = CARTESIAN_POINT ( 'NONE',  ( 113.6471614775786492, -5.638512984488999180, -18.83840828888717311 ) ) ;
#40505 = ORIENTED_EDGE ( 'NONE', *, *, #15886, .F. ) ;
#40506 = CARTESIAN_POINT ( 'NONE',  ( 113.0798948109119948, -8.899110576539710493, -16.42337572283490132 ) ) ;
#40507 = VECTOR ( 'NONE', #40812, 1000.000000000000227 ) ;
#40508 = CARTESIAN_POINT ( 'NONE',  ( 111.2646414775786496, -8.899110576539710493, -16.42337572283490132 ) ) ;
#40509 = CARTESIAN_POINT ( 'NONE',  ( 118.8660148109119774, -10.30919188438810075, -12.61870101168855918 ) ) ;
#40510 = CARTESIAN_POINT ( 'NONE',  ( 124.2550481442452792, -0.1624402480850797581, -16.17319339645315424 ) ) ;
#40511 = CARTESIAN_POINT ( 'NONE',  ( 126.2404814775786264, -9.261995988541697145, -16.69588392320189030 ) ) ;
#40512 = VERTEX_POINT ( 'NONE', #27908 ) ;
#40513 = CARTESIAN_POINT ( 'NONE',  ( 118.9794681442453026, -0.8288870151387760510, -10.36305467784173118 ) ) ;
#40514 = CARTESIAN_POINT ( 'NONE',  ( 111.2646414775786496, -8.899110576539710493, -16.42337572283490132 ) ) ;
#40515 = CARTESIAN_POINT ( 'NONE',  ( 107.9128015045248219, -2.477300249445798297, -7.631215200338321125 ) ) ;
#40516 = EDGE_CURVE ( 'NONE', #27773, #9431, #34714, .T. ) ;
#40517 = CARTESIAN_POINT ( 'NONE',  ( 120.1707281442453166, -9.565557343593413364, -10.61323700422348004 ) ) ;
#40518 = CARTESIAN_POINT ( 'NONE',  ( 110.1353015045248185, -2.477300249445851144, -7.631215200338310467 ) ) ;
#40519 = CIRCLE ( 'NONE', #29570, 2.000000000000000444 ) ;
#40520 = DIRECTION ( 'NONE',  ( 1.000000000000000000, 0.000000000000000000, -0.000000000000000000 ) ) ;
#40521 = EDGE_LOOP ( 'NONE', ( #4631, #28909, #11516, #35757, #39233, #8675 ) ) ;
#40522 = CARTESIAN_POINT ( 'NONE',  ( 85.70478001548416103, -25.99489077589524300, -13.39321520033831447 ) ) ;
#40523 = CARTESIAN_POINT ( 'NONE',  ( 124.5386814775786206, -5.638512984488999180, -18.83840828888717311 ) ) ;
#40524 = CIRCLE ( 'NONE', #7026, 4.000000000000000888 ) ;
#40525 = CARTESIAN_POINT ( 'NONE',  ( 113.2606921295247702, -9.868328341294093420, -13.39321520033836421 ) ) ;
#40526 = CARTESIAN_POINT ( 'NONE',  ( 112.3991748109119868, -8.166667518702817929, -8.995218007635859436 ) ) ;
#40527 = CARTESIAN_POINT ( 'NONE',  ( 94.86797725101185108, -25.51174947080612654, -12.63637840582423166 ) ) ;
#40528 = CARTESIAN_POINT ( 'NONE',  ( 106.5931921295248372, -9.868328341294093420, -13.39321520033831447 ) ) ;
#40529 = CARTESIAN_POINT ( 'NONE',  ( 70.19189222814998175, -61.33395589173652951, -37.73637771078367109 ) ) ;
#40530 = CIRCLE ( 'NONE', #32472, 6.000000000000005329 ) ;
#40531 = CARTESIAN_POINT ( 'NONE',  ( 135.7445839641027305, -4.121996687475771637, -19.31599879726310576 ) ) ;
#40532 = CARTESIAN_POINT ( 'NONE',  ( 125.2320293092190013, -12.02258392215929561, -14.78429556032320669 ) ) ;
#40533 = EDGE_CURVE ( 'NONE', #18672, #25132, #40923, .T. ) ;
#40534 = CARTESIAN_POINT ( 'NONE',  ( 123.9832704359119759, 0.5245030254254422486, -13.89657392289357141 ) ) ;
#40535 = CARTESIAN_POINT ( 'NONE',  ( 116.5969481442453031, -9.859900752359374465, -12.68260735090039404 ) ) ;
#40536 = CARTESIAN_POINT ( 'NONE',  ( 125.2761281442453054, 0.4262465694468514643, -12.03445270309931736 ) ) ;
#40537 = ORIENTED_EDGE ( 'NONE', *, *, #20396, .T. ) ;
#40538 = CARTESIAN_POINT ( 'NONE',  ( 123.1772414775786189, -4.089484607189486809, -7.948022111789456723 ) ) ;
#40539 = CARTESIAN_POINT ( 'NONE',  ( 116.4267681442453153, -3.383040157471821630, -19.15922257007629170 ) ) ;
#40540 = CARTESIAN_POINT ( 'NONE',  ( 116.7333483795247844, -8.402594152722688392, -16.93181055722141792 ) ) ;
#40541 = DIRECTION ( 'NONE',  ( 0.000000000000000000, 0.000000000000000000, -1.000000000000000000 ) ) ;
#40542 = CARTESIAN_POINT ( 'NONE',  ( 124.5954081442453116, -6.222761293078241884, -8.102969835052219238 ) ) ;
#40543 = CARTESIAN_POINT ( 'NONE',  ( 124.8223148109119762, 0.9020085738987339008, -11.91225656197089222 ) ) ;
#40544 = CARTESIAN_POINT ( 'NONE',  ( 106.0375671295248310, 0.1403307496149613920, -13.39321520033831447 ) ) ;
#40545 = CARTESIAN_POINT ( 'NONE',  ( 109.7185827545247889, -6.936859964151250502, -8.388885654883777576 ) ) ;
#40546 = CARTESIAN_POINT ( 'NONE',  ( 82.82366151329020454, -31.79927569882703153, -23.15978140744613256 ) ) ;
#40547 = CARTESIAN_POINT ( 'NONE',  ( 114.8951481442453115, -8.899110576539710493, -16.42337572283490132 ) ) ;
#40548 = CARTESIAN_POINT ( 'NONE',  ( 117.1642148109119859, -0.8288870151387760510, -10.36305467784173118 ) ) ;
#40549 = CARTESIAN_POINT ( 'NONE',  ( 117.2294421295247844, 7.836001204160461420, -14.64321520033831447 ) ) ;
#40550 = AXIS2_PLACEMENT_3D ( 'NONE', #24037, #37235, #2362 ) ;
#40551 = CARTESIAN_POINT ( 'NONE',  ( 114.7886608795247696, -1.325403438956436419, -16.93181055722141792 ) ) ;
#40552 = ORIENTED_EDGE ( 'NONE', *, *, #19475, .F. ) ;
#40553 = CARTESIAN_POINT ( 'NONE',  ( 122.4514248082055587, -0.1020945015695078478, -15.74893487844866691 ) ) ;
#40554 = CARTESIAN_POINT ( 'NONE',  ( 124.3685014775786328, 0.4262465694468514643, -12.03445270309931736 ) ) ;
#40555 = CARTESIAN_POINT ( 'NONE',  ( 120.3685329359119862, -5.367793381288652910, -18.78638297431638904 ) ) ;
#40556 = CARTESIAN_POINT ( 'NONE',  ( 122.3132204359119868, -10.25716656981731489, -12.88942061488890545 ) ) ;
#40557 = VERTEX_POINT ( 'NONE', #37712 ) ;
#40558 = DIRECTION ( 'NONE',  ( -0.000000000000000000, -0.9284778069183721172, -0.3713878862591650232 ) ) ;
#40559 = CARTESIAN_POINT ( 'NONE',  ( 76.69189222814998175, -49.76310523276723785, -7.393215200338315363 ) ) ;
#40560 = CONICAL_SURFACE ( 'NONE', #15060, 2.000000000000000444, 0.9599310885968830309 ) ;
#40561 = ORIENTED_EDGE ( 'NONE', *, *, #8562, .T. ) ;
#40562 = CARTESIAN_POINT ( 'NONE',  ( 118.1852948109119836, -5.638512984488999180, -18.83840828888717311 ) ) ;
#40563 = CARTESIAN_POINT ( 'NONE',  ( 125.1059481442452750, -1.833838273342660141, -17.42832698103878286 ) ) ;
#40564 = CARTESIAN_POINT ( 'NONE',  ( 115.2922348109119781, 0.4262465694468514643, -12.03445270309931736 ) ) ;
#40565 = CARTESIAN_POINT ( 'NONE',  ( 67.08264006073221708, -20.21382323020432992, -16.39321520033831447 ) ) ;
#40566 = CARTESIAN_POINT ( 'NONE',  ( 114.7664692294923867, -2.263366209404213958, -18.10533625161307114 ) ) ;
#40567 = CARTESIAN_POINT ( 'NONE',  ( 112.7962614775786676, -3.383040157471821630, -19.15922257007629170 ) ) ;
#40568 = CARTESIAN_POINT ( 'NONE',  ( 110.4825671295247815, 0.1403307496149613920, -13.39321520033831447 ) ) ;
#40569 = CARTESIAN_POINT ( 'NONE',  ( 122.7234281442452755, -5.638512984488999180, -18.83840828888717311 ) ) ;
#40570 = DIRECTION ( 'NONE',  ( 0.000000000000000000, -0.9242245927363028635, -0.3818493186865930533 ) ) ;
#40571 = ORIENTED_EDGE ( 'NONE', *, *, #21238, .F. ) ;
#40572 = CARTESIAN_POINT ( 'NONE',  ( 113.9875214775786532, -0.4660016031367893996, -10.09054647747474043 ) ) ;
#40573 = CARTESIAN_POINT ( 'NONE',  ( 112.7962614775786676, -6.222761293078241884, -8.102969835052219238 ) ) ;
#40574 = CARTESIAN_POINT ( 'NONE',  ( 84.38170309240724976, -25.99489077589524300, -13.39321520033831447 ) ) ;
#40575 = CARTESIAN_POINT ( 'NONE',  ( 112.9097148109120070, 0.2603800115204892296, -16.42320221600525088 ) ) ;
#40576 = VERTEX_POINT ( 'NONE', #3498 ) ;
#40577 = CARTESIAN_POINT ( 'NONE',  ( 123.2906948109119867, -8.166667518702819706, -8.995218007635861213 ) ) ;
#40579 = DIRECTION ( 'NONE',  ( 0.000000000000000000, 0.000000000000000000, -1.000000000000000000 ) ) ;
#40578 = CIRCLE ( 'NONE', #39102, 2.445500000000001339 ) ;
#40580 = CARTESIAN_POINT ( 'NONE',  ( 119.9486391859119863, -8.318316608003105017, -9.227040655997587493 ) ) ;
#40581 = CARTESIAN_POINT ( 'NONE',  ( 124.7446598611595761, -1.036737761566197014, -17.24079555149560861 ) ) ;
#40582 = CARTESIAN_POINT ( 'NONE',  ( 115.4624148109119943, -4.153390946401321671, -8.397313243818183892 ) ) ;
#40583 = CARTESIAN_POINT ( 'NONE',  ( 123.6188425880120150, -4.416445946866398131, -15.23819856170553955 ) ) ;
#40584 = CARTESIAN_POINT ( 'NONE',  ( 114.4980614775786734, -2.084020599724406786, -8.691656652584148546 ) ) ;
#40585 = DIRECTION ( 'NONE',  ( 1.000000000000000000, 1.131967377815149893E-16, 4.676795828538290169E-17 ) ) ;
#40586 = CARTESIAN_POINT ( 'NONE',  ( 125.2732466787873591, -2.097490018383950439, -20.06580088923637106 ) ) ;
#40587 = CARTESIAN_POINT ( 'NONE',  ( 114.2144281442453178, -1.833838273342658809, -17.42832698103878286 ) ) ;
#40588 = CARTESIAN_POINT ( 'NONE',  ( 116.8805814775786445, -6.344957434206662583, -7.627207830600332805 ) ) ;
#40589 = CARTESIAN_POINT ( 'NONE',  ( 123.3550173109119612, -9.289237151508434209, -11.05642687123711276 ) ) ;
#40590 = CARTESIAN_POINT ( 'NONE',  ( 112.9664414775786412, 0.5811942927096154232, -14.16772938898807155 ) ) ;
#40591 = CARTESIAN_POINT ( 'NONE',  ( 114.6682414775786469, -7.894159318335828068, -9.358103419637847864 ) ) ;
#40592 = CARTESIAN_POINT ( 'NONE',  ( 123.6877814775786533, -3.383040157471821630, -19.15922257007629170 ) ) ;
#40593 = PRESENTATION_LAYER_ASSIGNMENT (  '', '', ( #19467 ) ) ;
#40594 = CARTESIAN_POINT ( 'NONE',  ( 120.9649014775786355, -3.383040157471821630, -19.15922257007629170 ) ) ;
#40595 = VERTEX_POINT ( 'NONE', #30871 ) ;
#40596 = CARTESIAN_POINT ( 'NONE',  ( 114.5547881442453217, -5.638512984488999180, -18.83840828888717311 ) ) ;
#40597 = CARTESIAN_POINT ( 'NONE',  ( 111.4549108795247747, -8.938348069036489818, -9.318865927141430916 ) ) ;
#40598 = CARTESIAN_POINT ( 'NONE',  ( 105.8986608795248401, -1.325403438956436419, -16.93181055722141792 ) ) ;
#40599 = CARTESIAN_POINT ( 'NONE',  ( 111.1770983795247787, -8.402594152722688392, -16.93181055722141792 ) ) ;
#40600 = CARTESIAN_POINT ( 'NONE',  ( 109.2294421295247844, -8.865838614420134434, -9.247624522711900497 ) ) ;
#40601 = CARTESIAN_POINT ( 'NONE',  ( 117.2209414775786485, -7.893985811506177619, -18.51759400769804742 ) ) ;
#40602 = EDGE_LOOP ( 'NONE', ( #17759, #22830, #10410, #21145 ) ) ;
#40603 = CARTESIAN_POINT ( 'NONE',  ( 126.0703014775786102, -9.988377603198980381, -10.36322818467138518 ) ) ;
#40604 = CARTESIAN_POINT ( 'NONE',  ( 124.7195491406318411, 0.3208234527006150749, -15.99825685930877128 ) ) ;
#40605 = CARTESIAN_POINT ( 'NONE',  ( 112.7962614775786676, -6.222761293078241884, -8.102969835052219238 ) ) ;
#40606 = ADVANCED_FACE ( 'NONE', ( #27461 ), #31869, .T. ) ;
#40607 = CARTESIAN_POINT ( 'NONE',  ( 105.7597546295248350, -4.863998795839590272, -18.39754474579285315 ) ) ;
#40608 = CARTESIAN_POINT ( 'NONE',  ( 119.5467348109119712, -4.089484607189486809, -7.948022111789456723 ) ) ;
#40609 = CARTESIAN_POINT ( 'NONE',  ( 114.9275671295247889, 0.1403307496149613920, -13.39321520033831447 ) ) ;
#40610 = CARTESIAN_POINT ( 'NONE',  ( 119.6392035773848761, -2.467220198592778413, -17.83387418641524391 ) ) ;
#40611 = VERTEX_POINT ( 'NONE', #79 ) ;
#40612 = CARTESIAN_POINT ( 'NONE',  ( 125.4584548109119737, -0.8336775508564547854, -5.760888413673081132 ) ) ;
#40613 = CARTESIAN_POINT ( 'NONE',  ( 120.8514481442452961, -2.084020599724406786, -8.691656652584148546 ) ) ;
#40614 = CARTESIAN_POINT ( 'NONE',  ( 121.4187148109119789, -6.344957434206665248, -7.627207830600338134 ) ) ;
#40615 = AXIS2_PLACEMENT_3D ( 'NONE', #8783, #16079, #29308 ) ;
#40616 = CARTESIAN_POINT ( 'NONE',  ( 114.1577014775786552, -3.505236298600246325, -18.68346056562440793 ) ) ;
#40617 = CARTESIAN_POINT ( 'NONE',  ( 116.9940348109119839, -9.988377603198976828, -10.36322818467138340 ) ) ;
#40618 = CARTESIAN_POINT ( 'NONE',  ( 69.48536631248848039, -66.77523564985355620, -42.98127819198803934 ) ) ;
#40619 = CARTESIAN_POINT ( 'NONE',  ( 127.3669547543381810, -1.266902555130286379, -9.134731740105504372 ) ) ;
#40620 = CARTESIAN_POINT ( 'NONE',  ( 118.9227414775786542, 0.4262465694468514643, -12.03445270309931736 ) ) ;
#40621 = ORIENTED_EDGE ( 'NONE', *, *, #27064, .F. ) ;
#40622 = CARTESIAN_POINT ( 'NONE',  ( 123.5633766859119760, -0.06289925094097943703, -9.412459353600674206 ) ) ;
#40623 = CARTESIAN_POINT ( 'NONE',  ( 114.8384214775786489, 0.9020085738987339008, -11.91225656197089222 ) ) ;
#40624 = CARTESIAN_POINT ( 'NONE',  ( 120.9649014775786355, -6.222761293078241884, -8.102969835052219238 ) ) ;
#40625 = VERTEX_POINT ( 'NONE', #7140 ) ;
#40626 = CARTESIAN_POINT ( 'NONE',  ( 123.3550173109119612, -9.289237151508434209, -11.05642687123711276 ) ) ;
#40627 = CARTESIAN_POINT ( 'NONE',  ( 118.4122014775786340, 0.5811942927096110934, -14.16772938898807510 ) ) ;
#40628 = CARTESIAN_POINT ( 'NONE',  ( 112.5661608795247872, -8.938348069036489818, -9.318865927141430916 ) ) ;
#40629 = CARTESIAN_POINT ( 'NONE',  ( 116.8805814775786445, -3.505236298600246325, -18.68346056562440793 ) ) ;
#40630 = EDGE_CURVE ( 'NONE', #24205, #34050, #16674, .T. ) ;
#40631 = ORIENTED_EDGE ( 'NONE', *, *, #42046, .F. ) ;
#40632 = ORIENTED_EDGE ( 'NONE', *, *, #11962, .F. ) ;
#40633 = CARTESIAN_POINT ( 'NONE',  ( 111.7751814775786556, -7.893985811506177619, -18.51759400769804742 ) ) ;
#40634 = CARTESIAN_POINT ( 'NONE',  ( 121.5321681442453183, -0.1624402480850797581, -16.17319339645315424 ) ) ;
#40635 = CARTESIAN_POINT ( 'NONE',  ( 71.02242295334774269, -60.83132161787954573, -40.64013340189661960 ) ) ;
#40636 = EDGE_CURVE ( 'NONE', #39949, #18111, #11537, .T. ) ;
#40637 = VERTEX_POINT ( 'NONE', #35453 ) ;
#40638 = EDGE_CURVE ( 'NONE', #5980, #2538, #2705, .T. ) ;
#40639 = CARTESIAN_POINT ( 'NONE',  ( 118.0718414775786300, -9.261995988541697145, -16.69588392320189030 ) ) ;
#40640 = CARTESIAN_POINT ( 'NONE',  ( 107.9128015045248219, -2.477300249445798297, -7.631215200338321125 ) ) ;
#40641 = CARTESIAN_POINT ( 'NONE',  ( 119.4332814775786318, -0.4660016031367893996, -10.09054647747474043 ) ) ;
#40643 = CARTESIAN_POINT ( 'NONE',  ( 120.2274548109119934, -9.859900752359374465, -12.68260735090039404 ) ) ;
#40642 = CARTESIAN_POINT ( 'NONE',  ( 114.4413348109119823, -9.261995988541697145, -16.69588392320189030 ) ) ;
#40644 = DIRECTION ( 'NONE',  ( 0.000000000000000000, 0.000000000000000000, 1.000000000000000000 ) ) ;
#40645 = CARTESIAN_POINT ( 'NONE',  ( 112.2857214775786474, -4.089484607189486809, -7.948022111789456723 ) ) ;
#40646 = EDGE_LOOP ( 'NONE', ( #4434, #42637, #2343, #31490 ) ) ;
#40647 = CARTESIAN_POINT ( 'NONE',  ( 121.8158014775786171, -4.153390946401325223, -8.397313243818185668 ) ) ;
#40648 = FACE_OUTER_BOUND ( 'NONE', #23333, .T. ) ;
#40649 = ADVANCED_FACE ( 'NONE', ( #18146 ), #2662, .T. ) ;
#40650 = CARTESIAN_POINT ( 'NONE',  ( 72.51188087854242781, -21.10583385764521225, -17.89321520033831447 ) ) ;
#40651 = CARTESIAN_POINT ( 'NONE',  ( 114.9275671295247889, -10.62599879583958540, -13.39321520033831447 ) ) ;
#40652 = CARTESIAN_POINT ( 'NONE',  ( 111.4549108795247747, -1.325403438956436419, -16.93181055722141792 ) ) ;
#40653 = CARTESIAN_POINT ( 'NONE',  ( 112.0105358795247810, -0.7896495226426338832, -17.46756447353520159 ) ) ;
#40654 = CARTESIAN_POINT ( 'NONE',  ( 121.2485348109119769, -0.4660016031367893996, -10.09054647747474043 ) ) ;
#40655 = CARTESIAN_POINT ( 'NONE',  ( 121.7023481442452919, -0.8288870151387760510, -10.36305467784173118 ) ) ;
#40656 = ORIENTED_EDGE ( 'NONE', *, *, #26390, .F. ) ;
#40657 = EDGE_CURVE ( 'NONE', #18680, #20781, #10428, .T. ) ;
#40658 = CARTESIAN_POINT ( 'NONE',  ( 120.2841814775786276, 0.9020085738987339008, -11.91225656197089222 ) ) ;
#40659 = CARTESIAN_POINT ( 'NONE',  ( 59.58307739690713589, -13.63526775528386459, -19.38935094674975801 ) ) ;
#40660 = CARTESIAN_POINT ( 'NONE',  ( 121.5888948109119809, -10.30919188438810075, -12.61870101168855918 ) ) ;
#40661 = EDGE_CURVE ( 'NONE', #33578, #13545, #23167, .T. ) ;
#40662 = EDGE_CURVE ( 'NONE', #30417, #42647, #22815, .T. ) ;
#40663 = CARTESIAN_POINT ( 'NONE',  ( 122.1561614775786353, -0.4660016031367893996, -10.09054647747474043 ) ) ;
#40664 = CARTESIAN_POINT ( 'NONE',  ( 85.72471707980444933, -15.28778963902104060, -9.893215200338316251 ) ) ;
#40665 = CARTESIAN_POINT ( 'NONE',  ( 124.4252281442452812, -0.8288870151387760510, -10.36305467784173118 ) ) ;
#40666 = CARTESIAN_POINT ( 'NONE',  ( 87.14323352029596492, -25.99489077589524300, -13.39321520033831625 ) ) ;
#40667 = CARTESIAN_POINT ( 'NONE',  ( 111.7297369549021937, -1.135392229370322026, -17.10942237759953954 ) ) ;
#40668 = VERTEX_POINT ( 'NONE', #20911 ) ;
#40669 = CARTESIAN_POINT ( 'NONE',  ( -2.210854019365580569, -6.947965325911625634, -7.693738507800350845 ) ) ;
#40670 = CARTESIAN_POINT ( 'NONE',  ( 73.01241679510815175, -68.13509210538408922, -39.58160742654554554 ) ) ;
#40671 = CARTESIAN_POINT ( 'NONE',  ( 124.7088614775786226, -9.565557343593413364, -10.61323700422348004 ) ) ;
#40672 = CARTESIAN_POINT ( 'NONE',  ( 107.4266296295248821, -4.863998795839590272, -8.388885654883775800 ) ) ;
#40673 = CARTESIAN_POINT ( 'NONE',  ( 111.7327233795247849, -1.325403438956436419, -9.854619843455211026 ) ) ;
#40674 = CARTESIAN_POINT ( 'NONE',  ( 117.5613014775786525, -10.15424416112533912, -14.75197769757731336 ) ) ;
#40675 = CARTESIAN_POINT ( 'NONE',  ( 64.73784058450603140, -41.08681216603740438, -10.39321520033831625 ) ) ;
#40676 = CARTESIAN_POINT ( 'NONE',  ( 71.45846722029260434, -25.75860963767633649, -5.221760208414266025 ) ) ;
#40677 = CARTESIAN_POINT ( 'NONE',  ( 117.1074881442453233, 0.4262465694468514643, -12.03445270309931736 ) ) ;
#40678 = B_SPLINE_CURVE_WITH_KNOTS ( 'NONE', 3,
 ( #450, #14141, #4316, #21653, #42413, #17787, #32131, #4084, #28951, #42189 ),
 .UNSPECIFIED., .F., .F.,
 ( 4, 3, 3, 4 ),
 ( 0.000000000000000000, 0.0002476486447138930014, 0.0004952972925464250303, 0.0009604418836934749786 ),
 .UNSPECIFIED. ) ;
#40679 = CARTESIAN_POINT ( 'NONE',  ( 123.3474214775786209, -9.988377603198976828, -10.36322818467138340 ) ) ;
#40680 = ORIENTED_EDGE ( 'NONE', *, *, #20085, .F. ) ;
#40681 = CARTESIAN_POINT ( 'NONE',  ( 121.4754414775786131, -1.833838273342659697, -17.42832698103878286 ) ) ;
#40682 = CARTESIAN_POINT ( 'NONE',  ( 117.6747548109119919, -1.834011780172310813, -8.268836392978581529 ) ) ;
#40683 = CARTESIAN_POINT ( 'NONE',  ( 124.3685014775786328, -10.63000616557722466, -14.87417383870573495 ) ) ;
#40684 = CONICAL_SURFACE ( 'NONE', #3528, 0.04618666666666765286, 0.7853981633974476129 ) ;
#40685 = CARTESIAN_POINT ( 'NONE',  ( 122.5532481442453019, 0.4262465694468514643, -12.03445270309931736 ) ) ;
#40686 = ORIENTED_EDGE ( 'NONE', *, *, #4400, .F. ) ;
#40687 = CARTESIAN_POINT ( 'NONE',  ( 120.9936110609119737, -6.340755971794696855, -8.611740276972787100 ) ) ;
#40688 = CARTESIAN_POINT ( 'NONE',  ( 123.8579614775786126, 0.5811942927096110934, -14.16772938898807510 ) ) ;
#40689 = CARTESIAN_POINT ( 'NONE',  ( 115.3489614775786407, -0.8288870151387760510, -10.36305467784173118 ) ) ;
#40690 = CARTESIAN_POINT ( 'NONE',  ( 124.1415948109119540, -6.344957434206665248, -7.627207830600338134 ) ) ;
#40691 = CARTESIAN_POINT ( 'NONE',  ( 108.5378796295247810, -4.863998795839590272, -19.15521520033831493 ) ) ;
#40692 = DIRECTION ( 'NONE',  ( 0.1352586133457952255, 0.9908103287288504424, 0.000000000000000000 ) ) ;
#40693 = ORIENTED_EDGE ( 'NONE', *, *, #38931, .T. ) ;
#40694 = EDGE_CURVE ( 'NONE', #2987, #31347, #4210, .T. ) ;
#40695 = CARTESIAN_POINT ( 'NONE',  ( 109.3713171295247832, 0.1403307496149613920, -13.39321520033831447 ) ) ;
#40696 = DIRECTION ( 'NONE',  ( 0.9609149988134837450, -0.1028163501681639419, 0.2570431154366518145 ) ) ;
#40697 = CARTESIAN_POINT ( 'NONE',  ( 120.6245414775786458, -0.1624402480850797581, -16.17319339645315424 ) ) ;
#40698 = CARTESIAN_POINT ( 'NONE',  ( 115.6325948109119821, -9.565557343593413364, -10.61323700422348004 ) ) ;
#40699 = CARTESIAN_POINT ( 'NONE',  ( 124.1585801725099998, -7.429215134363809092, -20.97079166887802160 ) ) ;
#40700 = EDGE_LOOP ( 'NONE', ( #42415, #2084, #34208, #30754 ) ) ;
#40701 = CARTESIAN_POINT ( 'NONE',  ( 116.0419921295247860, 0.1360012041604560795, -13.39321520033831447 ) ) ;
#40702 = CARTESIAN_POINT ( 'NONE',  ( 116.0864081442453113, -0.1624402480850797581, -16.17319339645315424 ) ) ;
#40703 = CARTESIAN_POINT ( 'NONE',  ( 113.8740681442453138, -9.859900752359374465, -12.68260735090039404 ) ) ;
#40704 = CARTESIAN_POINT ( 'NONE',  ( 66.43257361571872366, -0.06953383795915370202, -10.39321520033831447 ) ) ;
#40705 = CARTESIAN_POINT ( 'NONE',  ( 111.2646414775786496, -8.899110576539710493, -16.42337572283490132 ) ) ;
#40707 = CARTESIAN_POINT ( 'NONE',  ( 121.7590748109119687, -7.893985811506177619, -18.51759400769804742 ) ) ;
#40706 = FACE_OUTER_BOUND ( 'NONE', #1611, .T. ) ;
#40708 = CARTESIAN_POINT ( 'NONE',  ( 112.9097148109120070, 0.2603800115204892296, -16.42320221600525088 ) ) ;
#40709 = ORIENTED_EDGE ( 'NONE', *, *, #13949, .F. ) ;
#40710 = CARTESIAN_POINT ( 'NONE',  ( 114.5984981608379769, 0.3867979994853637526, -14.64321520033831447 ) ) ;
#40711 = CARTESIAN_POINT ( 'NONE',  ( 113.7015254349294793, -1.040089454026971172, -17.23633227186634187 ) ) ;
#40712 = CARTESIAN_POINT ( 'NONE',  ( 107.4960827545248350, -6.936859964151250502, -8.388885654883777576 ) ) ;
#40713 = EDGE_CURVE ( 'NONE', #6765, #1626, #34785, .T. ) ;
#40714 = CARTESIAN_POINT ( 'NONE',  ( 111.7751814775786556, -7.893985811506177619, -18.51759400769804742 ) ) ;
#40715 = CARTESIAN_POINT ( 'NONE',  ( 120.6812681442452941, 0.1319031606808879209, -14.10382304977623669 ) ) ;
#40716 = FACE_OUTER_BOUND ( 'NONE', #40646, .T. ) ;
#40717 = CARTESIAN_POINT ( 'NONE',  ( 112.4272546295247821, -4.863998795839590272, -18.39754474579285315 ) ) ;
#40718 = FACE_OUTER_BOUND ( 'NONE', #44231, .T. ) ;
#40719 = EDGE_CURVE ( 'NONE', #39549, #38098, #35502, .T. ) ;
#40720 = FACE_OUTER_BOUND ( 'NONE', #14996, .T. ) ;
#40721 = CARTESIAN_POINT ( 'NONE',  ( 113.1366214775786432, -7.643976991954091638, -18.09477374809248218 ) ) ;
#40722 = CARTESIAN_POINT ( 'NONE',  ( 112.1494421295248003, 0.8980012041604618078, -13.39321520033831447 ) ) ;
#40723 = CARTESIAN_POINT ( 'NONE',  ( 119.7434548109119703, -0.8336775508564547854, -5.760888413673081132 ) ) ;
#40724 = CARTESIAN_POINT ( 'NONE',  ( 112.0105358795247810, -0.7896495226426338832, -17.46756447353520159 ) ) ;
#40725 = CARTESIAN_POINT ( 'NONE',  ( 123.4608748109119745, -10.63000616557722466, -14.87417383870573495 ) ) ;
#40726 = CARTESIAN_POINT ( 'NONE',  ( 121.7590748109119687, -7.893985811506177619, -18.51759400769804742 ) ) ;
#40727 = DIRECTION ( 'NONE',  ( -0.5735764363510446051, 0.3127926500124816878, -0.7570804645221042017 ) ) ;
#40728 = EDGE_CURVE ( 'NONE', #15771, #10224, #37517, .T. ) ;
#40729 = CARTESIAN_POINT ( 'NONE',  ( 117.6747548109119919, -1.834011780172310813, -8.268836392978581529 ) ) ;
#40730 = CARTESIAN_POINT ( 'NONE',  ( 112.4559014775786494, -9.988377603198976828, -10.36322818467138340 ) ) ;
#40731 = ORIENTED_EDGE ( 'NONE', *, *, #8067, .F. ) ;
#40732 = CARTESIAN_POINT ( 'NONE',  ( 112.3424481442453384, -3.505236298600246325, -18.68346056562440793 ) ) ;
#40733 = CARTESIAN_POINT ( 'NONE',  ( 125.2761281442453054, -10.63000616557722466, -14.87417383870573495 ) ) ;
#40734 = CARTESIAN_POINT ( 'NONE',  ( 120.7379948109119709, -10.63000616557722466, -14.87417383870573495 ) ) ;
#40735 = CARTESIAN_POINT ( 'NONE',  ( 113.0231681442453322, 0.9020085738987339008, -11.91225656197089222 ) ) ;
#40736 = CONTEXT_DEPENDENT_SHAPE_REPRESENTATION ( #32601, #42717 ) ;
#40737 = CARTESIAN_POINT ( 'NONE',  ( 113.4202548109119846, 0.1319031606808879209, -14.10382304977623669 ) ) ;
#40738 = EDGE_LOOP ( 'NONE', ( #9228, #32635, #15634, #43590 ) ) ;
#40739 = CARTESIAN_POINT ( 'NONE',  ( 118.0151148109119816, 0.4262465694468514643, -12.03445270309931736 ) ) ;
#40740 = CARTESIAN_POINT ( 'NONE',  ( 114.6682414775786469, -7.894159318335828068, -9.358103419637847864 ) ) ;
#40741 = CARTESIAN_POINT ( 'NONE',  ( 110.7603796295247918, -4.863998795839590272, -19.15521520033831493 ) ) ;
#40742 = VECTOR ( 'NONE', #35020, 1000.000000000000114 ) ;
#40743 = CARTESIAN_POINT ( 'NONE',  ( 122.0994348109119443, -10.15424416112533912, -14.75197769757731336 ) ) ;
#40744 = CARTESIAN_POINT ( 'NONE',  ( 116.8434081373642641, -0.9077462878304770610, -16.84372492951588995 ) ) ;
#40745 = FACE_OUTER_BOUND ( 'NONE', #6501, .T. ) ;
#40746 = ORIENTED_EDGE ( 'NONE', *, *, #29592, .T. ) ;
#40747 = VECTOR ( 'NONE', #13789, 1000.000000000000000 ) ;
#40748 = CARTESIAN_POINT ( 'NONE',  ( 123.4244704359119709, -10.25716656981731489, -12.88942061488890545 ) ) ;
#40749 = CARTESIAN_POINT ( 'NONE',  ( 124.3117748109119844, -10.30919188438810075, -12.61870101168855918 ) ) ;
#40750 = CARTESIAN_POINT ( 'NONE',  ( 113.7231797178594093, -0.3595008806742178709, -15.96590799893916568 ) ) ;
#40751 = PRESENTATION_STYLE_ASSIGNMENT (( #2653 ) ) ;
#40752 = CARTESIAN_POINT ( 'NONE',  ( 116.4388388684191256, 2.231149969025194579, -6.374051288094602086 ) ) ;
#40753 = DIRECTION ( 'NONE',  ( 0.000000000000000000, 0.9284778069183720062, 0.3713878862591650232 ) ) ;
#40754 = CARTESIAN_POINT ( 'NONE',  ( 106.5237390045248418, -9.868328341294098749, -11.32035403202665869 ) ) ;
#40755 = EDGE_CURVE ( 'NONE', #38344, #43627, #38658, .T. ) ;
#40756 = CARTESIAN_POINT ( 'NONE',  ( 138.2184548109119930, -8.536181032868617180, -18.13822074491315561 ) ) ;
#40757 = CARTESIAN_POINT ( 'NONE',  ( 136.3620199738656993, -4.220151613809025370, -19.16374751516046970 ) ) ;
#40758 = LINE ( 'NONE', #23890, #33963 ) ;
#40759 = CARTESIAN_POINT ( 'NONE',  ( 124.6778016859120015, -9.030173340179786123, -16.84753301250241009 ) ) ;
#40760 = CARTESIAN_POINT ( 'NONE',  ( 121.6456214775786293, 0.4262465694468514643, -12.03445270309931736 ) ) ;
#40761 = CARTESIAN_POINT ( 'NONE',  ( 119.7434548109120271, -0.1940514955484507198, -11.17407767511812899 ) ) ;
#40762 = ORIENTED_EDGE ( 'NONE', *, *, #15556, .T. ) ;
#40763 = CARTESIAN_POINT ( 'NONE',  ( 122.2696148109119889, -4.089484607189486809, -7.948022111789456723 ) ) ;
#40764 = CARTESIAN_POINT ( 'NONE',  ( 119.6601881442453106, -8.166667518702819706, -8.995218007635861213 ) ) ;
#40765 = CARTESIAN_POINT ( 'NONE',  ( 116.3166296295247832, -4.863998795839590272, -8.388885654883775800 ) ) ;
#40766 = CARTESIAN_POINT ( 'NONE',  ( 113.3068014775786594, -1.833838273342658809, -17.42832698103878286 ) ) ;
#40767 = CARTESIAN_POINT ( 'NONE',  ( 113.4769814775786330, -10.63000616557722466, -14.87417383870573495 ) ) ;
#40768 = CARTESIAN_POINT ( 'NONE',  ( 124.7655881442452852, 0.5811942927096110934, -14.16772938898807510 ) ) ;
#40769 = CARTESIAN_POINT ( 'NONE',  ( 111.8021765045248372, -7.250697342233347165, -19.15521520033831138 ) ) ;
#40770 = CARTESIAN_POINT ( 'NONE',  ( 109.0935046295247872, -4.863998795839590272, -18.39754474579285315 ) ) ;
#40771 = CARTESIAN_POINT ( 'NONE',  ( 116.2471765045247594, -7.250697342233347165, -19.15521520033831138 ) ) ;
#40772 = CARTESIAN_POINT ( 'NONE',  ( 117.1074881442453233, 0.4262465694468514643, -12.03445270309931736 ) ) ;
#40773 = CARTESIAN_POINT ( 'NONE',  ( 116.8238548109119819, -5.574606645277164318, -18.38911715685844683 ) ) ;
#40774 = EDGE_CURVE ( 'NONE', #36801, #6063, #18154, .T. ) ;
#40775 = VECTOR ( 'NONE', #10992, 1000.000000000000114 ) ;
#40776 = CARTESIAN_POINT ( 'NONE',  ( 83.84865386347668448, -25.99489077589588604, -15.39321520033831625 ) ) ;
#40777 = CARTESIAN_POINT ( 'NONE',  ( 113.6774108795247997, -1.325403438956436419, -16.93181055722141792 ) ) ;
#40778 = VERTEX_POINT ( 'NONE', #35691 ) ;
#40779 = CARTESIAN_POINT ( 'NONE',  ( 124.1299648136183293, -3.929494816604725216, -18.62311481910882094 ) ) ;
#40780 = CARTESIAN_POINT ( 'NONE',  ( 111.9453614775786434, -1.561330072975668060, -17.79121239304076596 ) ) ;
#40781 = CARTESIAN_POINT ( 'NONE',  ( 112.0020881442453344, 0.2603800115204892296, -16.42320221600525088 ) ) ;
#40782 = CARTESIAN_POINT ( 'NONE',  ( 120.9936110609119737, -6.340755971794695078, -8.611740276972781771 ) ) ;
#40783 = CARTESIAN_POINT ( 'NONE',  ( 121.6881423109119709, -0.4387604401700512802, -15.73000352943951619 ) ) ;
#40784 = ORIENTED_EDGE ( 'NONE', *, *, #22523, .T. ) ;
#40785 = CARTESIAN_POINT ( 'NONE',  ( 114.2330358795247776, -0.7896495226426338832, -17.46756447353520159 ) ) ;
#40786 = DIRECTION ( 'NONE',  ( 0.000000000000000000, -0.3818493186865927203, 0.9242245927363029745 ) ) ;
#40787 = ORIENTED_EDGE ( 'NONE', *, *, #6638, .T. ) ;
#40788 = CARTESIAN_POINT ( 'NONE',  ( 118.2987481442453088, -1.561330072975668504, -17.79121239304076951 ) ) ;
#40789 = VECTOR ( 'NONE', #27940, 1000.000000000000227 ) ;
#40790 = CARTESIAN_POINT ( 'NONE',  ( 123.6310548109119765, -4.153390946401325223, -8.397313243818185668 ) ) ;
#40791 = CARTESIAN_POINT ( 'NONE',  ( 114.6682414775786469, -7.894159318335828068, -9.358103419637847864 ) ) ;
#40792 = SURFACE_SIDE_STYLE ('',( #26876 ) ) ;
#40793 = AXIS2_PLACEMENT_3D ( 'NONE', #11355, #855, #29126 ) ;
#40794 = DIRECTION ( 'NONE',  ( -0.2768435750659241079, -0.3568721902840686355, 0.8921882507333134260 ) ) ;
#40795 = CARTESIAN_POINT ( 'NONE',  ( 120.6245414775786458, -9.988377603198976828, -10.36322818467138340 ) ) ;
#40796 = CARTESIAN_POINT ( 'NONE',  ( 112.8529881442453302, -1.561330072975668060, -17.79121239304076596 ) ) ;
#40797 = CARTESIAN_POINT ( 'NONE',  ( 113.2606921295247702, -9.868328341294093420, -13.39321520033831447 ) ) ;
#40798 = EDGE_CURVE ( 'NONE', #34402, #44995, #19515, .T. ) ;
#40799 = CARTESIAN_POINT ( 'NONE',  ( 123.5743281442453139, -7.893985811506177619, -18.51759400769804742 ) ) ;
#40800 = LINE ( 'NONE', #1794, #27213 ) ;
#40801 = ORIENTED_EDGE ( 'NONE', *, *, #527, .F. ) ;
#40802 = CARTESIAN_POINT ( 'NONE',  ( 117.9016614775786280, -9.988377603198976828, -10.36322818467138340 ) ) ;
#40803 = CARTESIAN_POINT ( 'NONE',  ( 114.6682414775786469, -7.894159318335828068, -9.358103419637847864 ) ) ;
#40804 = CARTESIAN_POINT ( 'NONE',  ( 126.5125895482189833, -4.945298539089557188, -18.53964231575977095 ) ) ;
#40805 = CARTESIAN_POINT ( 'NONE',  ( 126.1837548109119496, 0.4262465694468514643, -12.03445270309931736 ) ) ;
#40806 = ORIENTED_EDGE ( 'NONE', *, *, #13435, .T. ) ;
#40807 = CARTESIAN_POINT ( 'NONE',  ( 123.1205148109119563, -1.834011780172310813, -8.268836392978581529 ) ) ;
#40808 = CIRCLE ( 'NONE', #5078, 2.000000000000000444 ) ;
#40809 = DIRECTION ( 'NONE',  ( -0.2768435750659241079, -0.3568721902840695792, 0.8921882507333129819 ) ) ;
#40810 = DIRECTION ( 'NONE',  ( 0.000000000000000000, -0.3818493186865927203, 0.9242245927363029745 ) ) ;
#40811 = DIRECTION ( 'NONE',  ( 0.000000000000000000, 0.4669533266896288004, 0.8842819633428518067 ) ) ;
#40812 = DIRECTION ( 'NONE',  ( -0.000000000000000000, -0.9284778069183718952, -0.3713878862591649677 ) ) ;
#40813 = CARTESIAN_POINT ( 'NONE',  ( 116.3700414775786527, -4.153390946401321671, -8.397313243818183892 ) ) ;
#40814 = CARTESIAN_POINT ( 'NONE',  ( 136.4173705901582423, -2.656029227767985113, -8.046337796338329795 ) ) ;
#40815 = CARTESIAN_POINT ( 'NONE',  ( 116.9373081442452929, -1.833838273342659253, -17.42832698103878286 ) ) ;
#40816 = CARTESIAN_POINT ( 'NONE',  ( 114.3719421295247827, -9.868328341294093420, -13.39321520033831447 ) ) ;
#40817 = VECTOR ( 'NONE', #28218, 1000.000000000000000 ) ;
#40818 = CARTESIAN_POINT ( 'NONE',  ( 70.19189222814998175, -100.0979043305785581, -53.24182196210380624 ) ) ;
#40819 = CARTESIAN_POINT ( 'NONE',  ( 116.7671281442453335, -7.643976991954077427, -18.09477374809248928 ) ) ;
#40820 = CIRCLE ( 'NONE', #29153, 0.8718221387495408425 ) ;
#40821 = CARTESIAN_POINT ( 'NONE',  ( 115.9162281442453235, -4.089484607189486809, -7.948022111789456723 ) ) ;
#40822 = CARTESIAN_POINT ( 'NONE',  ( 123.7717360609119623, -3.387241619883791355, -18.17469012370385073 ) ) ;
#40823 = CARTESIAN_POINT ( 'NONE',  ( 112.1722681442453222, -0.4660016031367893996, -10.09054647747474043 ) ) ;
#40824 = CARTESIAN_POINT ( 'NONE',  ( 115.2922348109119781, 0.4262465694468514643, -12.03445270309931736 ) ) ;
#40825 = CARTESIAN_POINT ( 'NONE',  ( 125.0492214775786266, -6.344957434206665248, -7.627207830600338134 ) ) ;
#40826 = CARTESIAN_POINT ( 'NONE',  ( 120.4543614775786295, -4.089484607189486809, -7.948022111789456723 ) ) ;
#40827 = ORIENTED_EDGE ( 'NONE', *, *, #9452, .F. ) ;
#40828 = CARTESIAN_POINT ( 'NONE',  ( 111.9453614775786434, -1.561330072975668060, -17.79121239304076596 ) ) ;
#40829 = CARTESIAN_POINT ( 'NONE',  ( 111.5243640045248412, -10.62599879583958717, -11.00651665394454604 ) ) ;
#40830 = CARTESIAN_POINT ( 'NONE',  ( 107.5655358795247736, -8.402594152722688392, -9.854619843455216355 ) ) ;
#40831 = DIRECTION ( 'NONE',  ( -0.1736481776669309696, -0.9848077530122079093, 0.000000000000000000 ) ) ;
#40832 = ADVANCED_FACE ( 'NONE', ( #35461 ), #4236, .F. ) ;
#40833 = CARTESIAN_POINT ( 'NONE',  ( 64.38113726523094726, -36.68293531231000060, -5.550475082982985420 ) ) ;
#40834 = CARTESIAN_POINT ( 'NONE',  ( 119.5467348109119712, -4.089484607189486809, -7.948022111789456723 ) ) ;
#40835 = EDGE_LOOP ( 'NONE', ( #20674, #10890, #29371, #3500, #19181 ) ) ;
#40836 = CARTESIAN_POINT ( 'NONE',  ( 125.4584548109119737, -7.429215134363809092, -20.97079166887802160 ) ) ;
#40837 = CARTESIAN_POINT ( 'NONE',  ( 117.2294421295247417, -10.75052641725357994, -21.89299348893975505 ) ) ;
#40838 = CARTESIAN_POINT ( 'NONE',  ( 115.6325948109119821, -9.565557343593413364, -10.61323700422348004 ) ) ;
#40839 = FACE_OUTER_BOUND ( 'NONE', #34716, .T. ) ;
#40840 = CARTESIAN_POINT ( 'NONE',  ( 122.7234281442452755, -5.638512984488999180, -18.83840828888717311 ) ) ;
#40841 = CARTESIAN_POINT ( 'NONE',  ( 114.5803015045248117, -6.936859964151250502, -18.39754474579286025 ) ) ;
#40842 = CARTESIAN_POINT ( 'NONE',  ( 71.02242295334774269, -55.98144579621563821, -38.70019997903393971 ) ) ;
#40843 = ORIENTED_EDGE ( 'NONE', *, *, #25319, .T. ) ;
#40844 = DIRECTION ( 'NONE',  ( -1.224775218828351615E-16, 0.3818493186865896116, -0.9242245927363041957 ) ) ;
#40845 = CARTESIAN_POINT ( 'NONE',  ( 121.4187148109119789, -3.505236298600246325, -18.68346056562440793 ) ) ;
#40846 = CARTESIAN_POINT ( 'NONE',  ( 119.9438214775786378, -7.893985811506177619, -18.51759400769804742 ) ) ;
#40847 = AXIS2_PLACEMENT_3D ( 'NONE', #6336, #43743, #20253 ) ;
#40848 = CARTESIAN_POINT ( 'NONE',  ( 112.1722681442453222, -8.899110576539710493, -16.42337572283490132 ) ) ;
#40849 = CARTESIAN_POINT ( 'NONE',  ( 114.3846081442453197, -10.63000616557722466, -14.87417383870573495 ) ) ;
#40850 = DIRECTION ( 'NONE',  ( 0.9063289528979890930, 0.4225728684367167087, 0.000000000000000000 ) ) ;
#40851 = DIRECTION ( 'NONE',  ( 0.000000000000000000, 0.000000000000000000, -1.000000000000000000 ) ) ;
#40852 = CARTESIAN_POINT ( 'NONE',  ( 119.1496481442453046, -6.222761293078241884, -8.102969835052219238 ) ) ;
#40853 = ORIENTED_EDGE ( 'NONE', *, *, #15006, .T. ) ;
#40854 = CARTESIAN_POINT ( 'NONE',  ( 122.1048610609119720, -3.163656168406935087, -18.89861972220014508 ) ) ;
#40855 = VECTOR ( 'NONE', #40727, 1000.000000000000114 ) ;
#40856 = CARTESIAN_POINT ( 'NONE',  ( 113.3635281442453504, -9.988377603198976828, -10.36322818467138340 ) ) ;
#40857 = CARTESIAN_POINT ( 'NONE',  ( 121.9292548109119849, -7.894159318335828068, -9.358103419637847864 ) ) ;
#40858 = ORIENTED_EDGE ( 'NONE', *, *, #29281, .F. ) ;
#40859 = CIRCLE ( 'NONE', #2226, 2.445500000000004448 ) ;
#40860 = CARTESIAN_POINT ( 'NONE',  ( 123.1466579359119891, -4.360204210389833968, -8.000047426360245240 ) ) ;
#40861 = CARTESIAN_POINT ( 'NONE',  ( 137.4443952029671721, -1.138448121875069941, -9.933366089684859901 ) ) ;
#40862 = CARTESIAN_POINT ( 'NONE',  ( 118.3554748109119998, 0.2603800115204892296, -16.42320221600525088 ) ) ;
#40863 = CARTESIAN_POINT ( 'NONE',  ( 110.8298327545248299, -2.477300249445798297, -19.15521520033831138 ) ) ;
#40864 = CARTESIAN_POINT ( 'NONE',  ( 117.8449348109119938, -1.833838273342659253, -17.42832698103878286 ) ) ;
#40865 = ORIENTED_EDGE ( 'NONE', *, *, #41467, .T. ) ;
#40866 = ORIENTED_EDGE ( 'NONE', *, *, #3466, .T. ) ;
#40867 = CARTESIAN_POINT ( 'NONE',  ( 124.8223148109119762, -10.15424416112533912, -14.75197769757731336 ) ) ;
#40868 = CARTESIAN_POINT ( 'NONE',  ( 119.3765548109119834, -10.15424416112533912, -14.75197769757731336 ) ) ;
#40869 = DIRECTION ( 'NONE',  ( 0.000000000000000000, 0.4669533266896289669, 0.8842819633428516957 ) ) ;
#40870 = DIRECTION ( 'NONE',  ( 1.000000000000000000, 0.000000000000000000, -0.000000000000000000 ) ) ;
#40871 = CARTESIAN_POINT ( 'NONE',  ( 123.2906948109119867, -8.166667518702819706, -8.995218007635861213 ) ) ;
#40872 = CARTESIAN_POINT ( 'NONE',  ( 106.3848327545248651, -2.477300249445798297, -19.15521520033831138 ) ) ;
#40873 = CIRCLE ( 'NONE', #22625, 2.999999999999998224 ) ;
#40874 = CARTESIAN_POINT ( 'NONE',  ( 119.1496481442453046, -3.383040157471821630, -19.15922257007629170 ) ) ;
#40876 = CARTESIAN_POINT ( 'NONE',  ( 119.8870948109119752, -0.8288870151387760510, -10.36305467784173118 ) ) ;
#40875 = CARTESIAN_POINT ( 'NONE',  ( 118.6958348109119754, -6.344957434206665248, -7.627207830600338134 ) ) ;
#40877 = CARTESIAN_POINT ( 'NONE',  ( 125.6732148109119862, -9.859900752359378018, -12.68260735090039759 ) ) ;
#40878 = CARTESIAN_POINT ( 'NONE',  ( 112.1155414775786454, 0.9020085738987339008, -11.91225656197089222 ) ) ;
#40879 = ORIENTED_EDGE ( 'NONE', *, *, #29, .T. ) ;
#40880 = CARTESIAN_POINT ( 'NONE',  ( 122.6099748109119929, -0.8288870151387760510, -10.36305467784173118 ) ) ;
#40881 = DIRECTION ( 'NONE',  ( -1.000000000000000000, 0.000000000000000000, -0.000000000000000000 ) ) ;
#40882 = DIRECTION ( 'NONE',  ( 0.000000000000000000, 0.4669533266896289669, 0.8842819633428518067 ) ) ;
#40883 = CARTESIAN_POINT ( 'NONE',  ( 107.5655358795247736, -0.7896495226426338832, -17.46756447353520159 ) ) ;
#40884 = CARTESIAN_POINT ( 'NONE',  ( 112.6356140045247827, 0.1403307496149616695, -15.46607636864997204 ) ) ;
#40885 = CARTESIAN_POINT ( 'NONE',  ( 105.8292077545248446, -7.250697342233347165, -7.631215200338321125 ) ) ;
#40886 = CARTESIAN_POINT ( 'NONE',  ( 120.7379948109119709, -10.63000616557722466, -14.87417383870573495 ) ) ;
#40887 = CARTESIAN_POINT ( 'NONE',  ( 122.4965214775786251, 0.1319031606808879209, -14.10382304977623669 ) ) ;
#40888 = VERTEX_POINT ( 'NONE', #14959 ) ;
#40889 = AXIS2_PLACEMENT_3D ( 'NONE', #466, #4330, #28293 ) ;
#40890 = CARTESIAN_POINT ( 'NONE',  ( 122.8368814775786291, -1.561330072975668948, -17.79121239304076951 ) ) ;
#40891 = CARTESIAN_POINT ( 'NONE',  ( 135.3184548109119874, -4.105398160058917334, -19.34506575923121474 ) ) ;
#40892 = CARTESIAN_POINT ( 'NONE',  ( 96.21525317080913453, -23.96406343964327590, -13.11138972548619641 ) ) ;
#40893 = CARTESIAN_POINT ( 'NONE',  ( 121.7590748109119687, -7.893985811506177619, -18.51759400769804742 ) ) ;
#40894 = CARTESIAN_POINT ( 'NONE',  ( 122.5532481442453019, -10.63000616557722466, -14.87417383870573495 ) ) ;
#40895 = CARTESIAN_POINT ( 'NONE',  ( 111.3768994516356230, -3.941856523015780489, -18.57470496855048481 ) ) ;
#40896 = CARTESIAN_POINT ( 'NONE',  ( 125.3328548109119964, -0.8288870151387760510, -10.36305467784173118 ) ) ;
#40897 = DIRECTION ( 'NONE',  ( 0.000000000000000000, -0.9284778069183722282, -0.3713878862591645791 ) ) ;
#40898 = CYLINDRICAL_SURFACE ( 'NONE', #11699, 3.000000000000001776 ) ;
#40899 = EDGE_CURVE ( 'NONE', #12518, #31222, #42784, .T. ) ;
#40900 = ORIENTED_EDGE ( 'NONE', *, *, #37558, .T. ) ;
#40901 = DIRECTION ( 'NONE',  ( -1.000000000000000000, 0.000000000000000000, 0.000000000000000000 ) ) ;
#40902 = CARTESIAN_POINT ( 'NONE',  ( 118.3179530757767566, -0.9924539043446216624, -17.29976612834909133 ) ) ;
#40903 = CARTESIAN_POINT ( 'NONE',  ( 122.9503348109119827, -9.859900752359378018, -12.68260735090039759 ) ) ;
#40904 = CARTESIAN_POINT ( 'NONE',  ( 109.5796765045248122, -2.791137627527939813, -8.388885654883777576 ) ) ;
#40905 = CARTESIAN_POINT ( 'NONE',  ( 113.0523327545247838, -6.936859964151250502, -8.388885654883777576 ) ) ;
#40906 = CARTESIAN_POINT ( 'NONE',  ( 118.1852948109119836, -4.153390946401325223, -8.397313243818185668 ) ) ;
#40907 =( NAMED_UNIT ( * ) PLANE_ANGLE_UNIT ( ) SI_UNIT ( $, .RADIAN. ) );
#40908 = CARTESIAN_POINT ( 'NONE',  ( 117.5613014775786525, -10.15424416112533912, -14.75197769757731336 ) ) ;
#40909 = CARTESIAN_POINT ( 'NONE',  ( 123.9714148109119805, -0.4660016031367893996, -10.09054647747474043 ) ) ;
#40910 = ORIENTED_EDGE ( 'NONE', *, *, #26803, .T. ) ;
#40911 = EDGE_CURVE ( 'NONE', #30461, #11921, #31158, .T. ) ;
#40912 = CARTESIAN_POINT ( 'NONE',  ( 121.4187148109119789, -3.505236298600246325, -18.68346056562440793 ) ) ;
#40913 = CARTESIAN_POINT ( 'NONE',  ( 119.6601881442453106, -8.166667518702819706, -8.995218007635861213 ) ) ;
#40914 = CARTESIAN_POINT ( 'NONE',  ( 124.7655881442452852, 0.5811942927096110934, -14.16772938898807510 ) ) ;
#40915 = CARTESIAN_POINT ( 'NONE',  ( 123.8579614775786126, -9.859900752359378018, -12.68260735090039759 ) ) ;
#40916 = ORIENTED_EDGE ( 'NONE', *, *, #29962, .T. ) ;
#40917 = DIRECTION ( 'NONE',  ( 0.000000000000000000, 0.6004852223388321697, -0.7996358532186279566 ) ) ;
#40918 = AXIS2_PLACEMENT_3D ( 'NONE', #30394, #3025, #44765 ) ;
#40919 = CARTESIAN_POINT ( 'NONE',  ( 125.6164881442453094, 0.2603800115204892296, -16.42320221600525088 ) ) ;
#40920 = CARTESIAN_POINT ( 'NONE',  ( 116.2565881442453133, -0.8288870151387760510, -10.36305467784173118 ) ) ;
#40921 = CARTESIAN_POINT ( 'NONE',  ( 124.8790414775786246, -0.4660016031367893996, -10.09054647747474043 ) ) ;
#40922 = EDGE_CURVE ( 'NONE', #28016, #21643, #15864, .T. ) ;
#40923 = LINE ( 'NONE', #17635, #16594 ) ;
#40924 = EDGE_CURVE ( 'NONE', #27136, #42526, #14095, .T. ) ;
#40925 = ADVANCED_FACE ( 'NONE', ( #2615 ), #11520, .T. ) ;
#40926 = CARTESIAN_POINT ( 'NONE',  ( 123.2161110609119703, -6.340755971794695078, -8.611740276972781771 ) ) ;
#40927 = ORIENTED_EDGE ( 'NONE', *, *, #7754, .F. ) ;
#40928 = FACE_OUTER_BOUND ( 'NONE', #5071, .T. ) ;
#40929 = CARTESIAN_POINT ( 'NONE',  ( 110.8992858795247827, -8.402594152722688392, -9.854619843455216355 ) ) ;
#40930 = CARTESIAN_POINT ( 'NONE',  ( 64.19189222814998175, -49.76310523276725206, -29.87698278062875445 ) ) ;
#40931 = CARTESIAN_POINT ( 'NONE',  ( 121.0216281442452981, -7.894159318335828068, -9.358103419637847864 ) ) ;
#40932 = CARTESIAN_POINT ( 'NONE',  ( 115.0086014775786509, -5.574606645277164318, -18.38911715685844683 ) ) ;
#40933 = CARTESIAN_POINT ( 'NONE',  ( 127.7425183523502881, -7.050714571525749541, -18.72418924296322729 ) ) ;
#40934 = ORIENTED_EDGE ( 'NONE', *, *, #39235, .T. ) ;
#40935 = CARTESIAN_POINT ( 'NONE',  ( 125.3328548109119964, -9.261995988541029234, -16.69588392320277848 ) ) ;
#40936 = CARTESIAN_POINT ( 'NONE',  ( 119.3198281442452924, -9.859900752359374465, -12.68260735090039404 ) ) ;
#40937 = CARTESIAN_POINT ( 'NONE',  ( 113.7606148109119886, -7.894159318335828068, -9.358103419637847864 ) ) ;
#40938 = DIRECTION ( 'NONE',  ( -0.000000000000000000, -0.9284778069183718952, -0.3713878862591649677 ) ) ;
#40939 = CARTESIAN_POINT ( 'NONE',  ( 111.4915481442453142, -1.833838273342658365, -17.42832698103878286 ) ) ;
#40941 = CARTESIAN_POINT ( 'NONE',  ( 124.1415948109119540, -6.344957434206665248, -7.627207830600338134 ) ) ;
#40940 = CARTESIAN_POINT ( 'NONE',  ( 70.29296507063932609, -26.37030337512767275, -5.626337071866863049 ) ) ;
#40942 = CARTESIAN_POINT ( 'NONE',  ( 125.9568481442452850, -3.505236298600246325, -18.68346056562440793 ) ) ;
#40943 = ORIENTED_EDGE ( 'NONE', *, *, #8438, .T. ) ;
#40944 = CARTESIAN_POINT ( 'NONE',  ( 114.8384214775786489, 0.9020085738987339008, -11.91225656197089222 ) ) ;
#40945 = DIRECTION ( 'NONE',  ( 0.000000000000000000, -0.9242245927363028635, -0.3818493186865930533 ) ) ;
#40946 = CARTESIAN_POINT ( 'NONE',  ( 106.6626452545248611, -9.868328341294098749, -15.46607636864997204 ) ) ;
#40947 = CARTESIAN_POINT ( 'NONE',  ( 125.9001214775786224, -5.574606645277164318, -18.38911715685844683 ) ) ;
#40948 = CARTESIAN_POINT ( 'NONE',  ( 121.1350814775786233, -9.859900752359378018, -12.68260735090039759 ) ) ;
#40949 = DIRECTION ( 'NONE',  ( -0.5735764363510446051, 0.3127926500124816878, -0.7570804645221042017 ) ) ;
#40950 = CARTESIAN_POINT ( 'NONE',  ( 112.7050671295247923, 0.1403307496149613920, -13.39321520033831447 ) ) ;
#40951 = EDGE_CURVE ( 'NONE', #10999, #37436, #11993, .T. ) ;
#40952 = AXIS2_PLACEMENT_3D ( 'NONE', #43846, #23555, #16024 ) ;
#40953 = CARTESIAN_POINT ( 'NONE',  ( 65.49983523453742862, -18.16718729050178993, -4.893215200338314474 ) ) ;
#40954 = CARTESIAN_POINT ( 'NONE',  ( 109.2294421295247275, -1.527404628864407199, -17.14082320569335494 ) ) ;
#40955 = CARTESIAN_POINT ( 'NONE',  ( 112.3424481442453384, -3.505236298600246325, -18.68346056562440793 ) ) ;
#40956 = CARTESIAN_POINT ( 'NONE',  ( 112.2188952545247531, 0.8980012041604421569, -11.00651665394454071 ) ) ;
#40957 = LINE ( 'NONE', #41414, #13187 ) ;
#40958 = CARTESIAN_POINT ( 'NONE',  ( 116.0388171295248014, -10.62599879583958540, -13.39321520033831447 ) ) ;
#40959 = CARTESIAN_POINT ( 'NONE',  ( 124.2550481442452792, -9.988377603198980381, -10.36322818467138518 ) ) ;
#40960 = CARTESIAN_POINT ( 'NONE',  ( 120.5110881442453206, -6.344957434206665248, -7.627207830600338134 ) ) ;
#40961 = CARTESIAN_POINT ( 'NONE',  ( 114.7886608795247696, -8.938348069036441856, -9.318865927141425587 ) ) ;
#40962 = ADVANCED_FACE ( 'NONE', ( #26573 ), #9470, .T. ) ;
#40963 = CARTESIAN_POINT ( 'NONE',  ( 120.3976348109119812, -1.834011780172310813, -8.268836392978581529 ) ) ;
#40964 = CARTESIAN_POINT ( 'NONE',  ( 114.2711548109119803, -9.988377603198976828, -10.36322818467138340 ) ) ;
#40965 = ORIENTED_EDGE ( 'NONE', *, *, #2147, .T. ) ;
#40966 = CARTESIAN_POINT ( 'NONE',  ( 113.3635281442453504, -0.1624402480850797581, -16.17319339645315424 ) ) ;
#40967 = ADVANCED_FACE ( 'NONE', ( #36591 ), #33383, .T. ) ;
#40968 = CARTESIAN_POINT ( 'NONE',  ( 126.0703014775786102, -9.988377603198980381, -10.36322818467138518 ) ) ;
#40969 = CARTESIAN_POINT ( 'NONE',  ( 125.1059481442452750, -8.166667518702819706, -8.995218007635861213 ) ) ;
#40970 = CARTESIAN_POINT ( 'NONE',  ( 113.0798948109119948, -0.4660016031367893996, -10.09054647747474043 ) ) ;
#40971 = CARTESIAN_POINT ( 'NONE',  ( 113.9875214775786532, -8.899110576539710493, -16.42337572283490132 ) ) ;
#40972 = ORIENTED_EDGE ( 'NONE', *, *, #13500, .F. ) ;
#40973 = CARTESIAN_POINT ( 'NONE',  ( 117.3911214775786505, -7.894159318335828068, -9.358103419637847864 ) ) ;
#40974 =( BOUNDED_CURVE ( )  B_SPLINE_CURVE ( 2, ( #4528, #18451, #42842, #32339, #36208, #18669, #25739, #1329, #4975, #15023, #1106, #1774, #39645, #36429, #15242, #18886, #26184 ),
 .UNSPECIFIED., .F., .F. ) 
 B_SPLINE_CURVE_WITH_KNOTS ( ( 3, 2, 2, 2, 2, 2, 2, 2, 3 ),
 ( 0.008913552404467750892, 0.03125000000000000000, 0.06250000000000000000, 0.09375000000000000000, 0.1250000000000000000, 0.1562500000000000000, 0.1875000000000000000, 0.2187500000000000000, 0.2410864475955325215 ),
 .UNSPECIFIED. ) 
 CURVE ( )  GEOMETRIC_REPRESENTATION_ITEM ( )  RATIONAL_B_SPLINE_CURVE ( ( 0.9689618144536780164, 0.9455916533437099813, 1.000000000000000000, 0.9238795325112869605, 1.000000000000000000, 0.9238795325112869605, 1.000000000000000000, 0.9238795325112869605, 1.000000000000000000, 0.9238795325112869605, 1.000000000000000000, 0.9238795325112869605, 1.000000000000000000, 0.9238795325112869605, 1.000000000000000000, 0.9455916533437099813, 0.9689618144536780164 ) ) 
 REPRESENTATION_ITEM ( '' )  );
#40975 = VECTOR ( 'NONE', #36944, 1000.000000000000114 ) ;
#40976 = CARTESIAN_POINT ( 'NONE',  ( 90.41915846579418314, -16.87387181286558757, -6.893215200338315363 ) ) ;
#40977 = CARTESIAN_POINT ( 'NONE',  ( 110.3436608795247764, -1.325403438956436419, -16.93181055722141792 ) ) ;
#40978 = CARTESIAN_POINT ( 'NONE',  ( 124.3117748109119844, 0.1319031606808879209, -14.10382304977623669 ) ) ;
#40979 = DIRECTION ( 'NONE',  ( 1.000000000000000000, 0.000000000000000000, -0.000000000000000000 ) ) ;
#40980 = CARTESIAN_POINT ( 'NONE',  ( 111.8021765045248372, -7.250697342233347165, -19.15521520033831138 ) ) ;
#40981 = VERTEX_POINT ( 'NONE', #23155 ) ;
#40982 = EDGE_CURVE ( 'NONE', #1412, #16965, #39695, .T. ) ;
#40983 = AXIS2_PLACEMENT_3D ( 'NONE', #16738, #15257, #2017 ) ;
#40984 = CARTESIAN_POINT ( 'NONE',  ( 61.35533094128319931, -2.221534154745201217, -7.278987677919483978 ) ) ;
#40985 = CARTESIAN_POINT ( 'NONE',  ( 125.9001214775786224, -4.089484607189486809, -7.948022111789456723 ) ) ;
#40986 = CARTESIAN_POINT ( 'NONE',  ( 113.3995983795247895, -8.402594152722633325, -16.93181055722145345 ) ) ;
#40987 = AXIS2_PLACEMENT_3D ( 'NONE', #28519, #18018, #11188 ) ;
#40988 = CARTESIAN_POINT ( 'NONE',  ( 111.8319081442453182, -5.638512984488999180, -18.83840828888717311 ) ) ;
#40989 = B_SPLINE_CURVE_WITH_KNOTS ( 'NONE', 3,
 ( #28145, #14230, #3293, #17215, #34730, #17430, #7376, #24939, #42056, #25620 ),
 .UNSPECIFIED., .F., .F.,
 ( 4, 3, 3, 4 ),
 ( 0.000000000000000000, 0.0001671877548681274892, 0.0003343755096277665107, 0.0006463528481650629171 ),
 .UNSPECIFIED. ) ;
#40990 = CARTESIAN_POINT ( 'NONE',  ( 112.7395348109119766, -5.638512984488999180, -18.83840828888717311 ) ) ;
#40991 = CARTESIAN_POINT ( 'NONE',  ( 70.19189222814998175, -52.04917782255280656, -34.02249884819201498 ) ) ;
#40992 = CARTESIAN_POINT ( 'NONE',  ( 106.6626452545248611, -9.868328341294098749, -15.46607636864997204 ) ) ;
#40993 = CARTESIAN_POINT ( 'NONE',  ( 123.2724088976799948, -1.244021962887374544, -16.96476564598603076 ) ) ;
#40994 = CARTESIAN_POINT ( 'NONE',  ( 118.1285681442453068, -7.893985811506177619, -18.51759400769804742 ) ) ;
#40995 = CARTESIAN_POINT ( 'NONE',  ( 137.4923962881472903, -5.828094238520085568, -18.32084130032456315 ) ) ;
#40996 = CARTESIAN_POINT ( 'NONE',  ( -12.61278219666105826, -4.053125158562569830, -19.39321520033831447 ) ) ;
#40997 = CARTESIAN_POINT ( 'NONE',  ( 124.6083485609119776, -9.641336978641852795, -14.86869474514273648 ) ) ;
#40998 = CARTESIAN_POINT ( 'NONE',  ( 120.9081748109119872, -4.153390946401325223, -8.397313243818185668 ) ) ;
#40999 = CARTESIAN_POINT ( 'NONE',  ( 119.7434548109119703, -5.531992483615866263, -19.02952050076702051 ) ) ;
#41000 = ORIENTED_EDGE ( 'NONE', *, *, #44574, .T. ) ;
#41001 = CARTESIAN_POINT ( 'NONE',  ( 123.2906948109119867, -8.166667518702819706, -8.995218007635861213 ) ) ;
#41002 = CARTESIAN_POINT ( 'NONE',  ( 119.2631014775786298, 0.2603800115204892296, -16.42320221600525088 ) ) ;
#41003 = CARTESIAN_POINT ( 'NONE',  ( 83.44708369096697709, -25.99489077589524300, -13.39321520033831625 ) ) ;
#41004 = CARTESIAN_POINT ( 'NONE',  ( 113.5337081442453240, -9.261995988541698921, -16.69588392320188674 ) ) ;
#41006 = CARTESIAN_POINT ( 'NONE',  ( 124.1415948109119540, -6.344957434206665248, -7.627207830600338134 ) ) ;
#41005 = AXIS2_PLACEMENT_3D ( 'NONE', #15487, #12750, #15942 ) ;
#41007 = CARTESIAN_POINT ( 'NONE',  ( 111.7327233795247849, -8.938348069036489818, -17.46756447353520159 ) ) ;
#41008 = FACE_OUTER_BOUND ( 'NONE', #21048, .T. ) ;
#41009 = CARTESIAN_POINT ( 'NONE',  ( 82.94154871197187617, -31.82278776394949205, -23.23890551632149482 ) ) ;
#41010 = CARTESIAN_POINT ( 'NONE',  ( 117.8449348109119938, -1.833838273342659253, -17.42832698103878286 ) ) ;
#41011 = VECTOR ( 'NONE', #22425, 1000.000000000000000 ) ;
#41012 = CARTESIAN_POINT ( 'NONE',  ( 118.4689281442453250, -10.15424416112533912, -14.75197769757731336 ) ) ;
#41013 = DIRECTION ( 'NONE',  ( 0.000000000000000000, -0.9284778069183718952, -0.3713878862591650232 ) ) ;
#41014 = CARTESIAN_POINT ( 'NONE',  ( 114.7192077545248594, -2.791137627527939813, -18.39754474579286025 ) ) ;
#41015 = ORIENTED_EDGE ( 'NONE', *, *, #27018, .T. ) ;
#41016 = PLANE ( 'NONE',  #16767 ) ;
#41017 = CARTESIAN_POINT ( 'NONE',  ( 115.4624148109119943, -5.638512984488999180, -18.83840828888717311 ) ) ;
#41018 = CARTESIAN_POINT ( 'NONE',  ( 73.60369002873177635, -5.846784287000932778, -18.64321520033831803 ) ) ;
#41019 = CARTESIAN_POINT ( 'NONE',  ( 122.3132204359119868, -10.25716656981731489, -12.88942061488890545 ) ) ;
#41020 = CARTESIAN_POINT ( 'NONE',  ( 120.7852516859119731, -0.6942167230862511529, -9.935906262978006609 ) ) ;
#41021 = ORIENTED_EDGE ( 'NONE', *, *, #12796, .F. ) ;
#41022 = CARTESIAN_POINT ( 'NONE',  ( 123.5975415792130292, -3.161545974351341659, -14.41132075528343570 ) ) ;
#41023 = CARTESIAN_POINT ( 'NONE',  ( 111.4966152579028034, -1.277474013852379908, -16.92021923864711752 ) ) ;
#41024 = ORIENTED_EDGE ( 'NONE', *, *, #43948, .T. ) ;
#41025 = AXIS2_PLACEMENT_3D ( 'NONE', #8325, #42091, #22002 ) ;
#41026 = CARTESIAN_POINT ( 'NONE',  ( 116.7104014775786425, -0.4660016031367893996, -10.09054647747474043 ) ) ;
#41027 = CARTESIAN_POINT ( 'NONE',  ( 113.4769814775786330, -10.63000616557722466, -14.87417383870573495 ) ) ;
#41028 = CARTESIAN_POINT ( 'NONE',  ( 116.6536748109119941, -10.15424416112533912, -14.75197769757731336 ) ) ;
#41029 = CARTESIAN_POINT ( 'NONE',  ( 151.2860562277021472, -4.863998795839242995, -13.39321520033831447 ) ) ;
#41030 = CARTESIAN_POINT ( 'NONE',  ( 121.7023481442452777, -9.261995988541697145, -16.69588392320189030 ) ) ;
#41031 = CARTESIAN_POINT ( 'NONE',  ( 117.3343948109119737, -3.383040157471821630, -19.15922257007629170 ) ) ;
#41032 = EDGE_CURVE ( 'NONE', #529, #25300, #41340, .T. ) ;
#41033 = CARTESIAN_POINT ( 'NONE',  ( 106.6626452545248611, -9.868328341294098749, -15.46607636864997204 ) ) ;
#41034 = CARTESIAN_POINT ( 'NONE',  ( 114.3278814775786429, 0.1319031606808879209, -14.10382304977623669 ) ) ;
#41035 = DIRECTION ( 'NONE',  ( 1.000000000000000000, 0.000000000000000000, -0.000000000000000000 ) ) ;
#41036 = VERTEX_POINT ( 'NONE', #33162 ) ;
#41037 = CARTESIAN_POINT ( 'NONE',  ( 116.3133148109119759, -7.893985811506177619, -18.51759400769804742 ) ) ;
#41038 = CIRCLE ( 'NONE', #6057, 3.000000000000003997 ) ;
#41039 = CARTESIAN_POINT ( 'NONE',  ( 118.2795432127138611, -2.191907684172563986, -18.20049396185734025 ) ) ;
#41040 = CARTESIAN_POINT ( 'NONE',  ( 115.0653281442453277, -6.344957434206662583, -7.627207830600332805 ) ) ;
#41041 = ORIENTED_EDGE ( 'NONE', *, *, #3091, .F. ) ;
#41042 = CARTESIAN_POINT ( 'NONE',  ( 120.8514481442452961, -7.893985811506177619, -18.51759400769804742 ) ) ;
#41043 = DIRECTION ( 'NONE',  ( 0.000000000000000000, 0.000000000000000000, -1.000000000000000000 ) ) ;
#41044 = CARTESIAN_POINT ( 'NONE',  ( 87.44708369096657918, -29.99489077589588959, -18.39321520033831803 ) ) ;
#41045 = DIRECTION ( 'NONE',  ( 1.000000000000000000, 0.000000000000000000, -0.000000000000000000 ) ) ;
#41046 = EDGE_CURVE ( 'NONE', #21853, #27652, #12904, .T. ) ;
#41047 = CARTESIAN_POINT ( 'NONE',  ( 118.0151148109119816, 0.4262465694468514643, -12.03445270309931736 ) ) ;
#41048 = DIRECTION ( 'NONE',  ( 0.9609149988134837450, -0.1028163501681639419, 0.2570431154366518145 ) ) ;
#41049 = CARTESIAN_POINT ( 'NONE',  ( 118.7525614775786380, -1.833838273342659253, -17.42832698103878286 ) ) ;
#41050 = AXIS2_PLACEMENT_3D ( 'NONE', #37809, #41480, #3598 ) ;
#41051 = CARTESIAN_POINT ( 'NONE',  ( 69.36136150295220659, -65.88636423853262158, -36.45251753205559453 ) ) ;
#41052 = CARTESIAN_POINT ( 'NONE',  ( 115.7460481442453357, -10.15424416112533912, -14.75197769757731336 ) ) ;
#41053 = CARTESIAN_POINT ( 'NONE',  ( 114.8384214775786489, 0.9020085738987339008, -11.91225656197089222 ) ) ;
#41054 = CARTESIAN_POINT ( 'NONE',  ( 122.2437673109119629, -9.289237151508434209, -11.05642687123711276 ) ) ;
#41055 = CARTESIAN_POINT ( 'NONE',  ( 126.5241148109119393, -9.565557343593413364, -10.61323700422348004 ) ) ;
#41056 = CARTESIAN_POINT ( 'NONE',  ( 116.2565881442453133, -0.8288870151387760510, -10.36305467784173118 ) ) ;
#41057 = CARTESIAN_POINT ( 'NONE',  ( 112.8529881442453160, -7.894159318335828068, -9.358103419637847864 ) ) ;
#41058 = CARTESIAN_POINT ( 'NONE',  ( 117.9016614775786280, -0.1624402480850797581, -16.17319339645315424 ) ) ;
#41059 = VERTEX_POINT ( 'NONE', #37037 ) ;
#41060 = FACE_OUTER_BOUND ( 'NONE', #37579, .T. ) ;
#41061 = CARTESIAN_POINT ( 'NONE',  ( 108.1906140045248463, -10.62599879583958717, -11.00651665394454604 ) ) ;
#41062 = CARTESIAN_POINT ( 'NONE',  ( 69.69189222814998175, -41.76310523276723785, -20.39321520033831447 ) ) ;
#41063 = CARTESIAN_POINT ( 'NONE',  ( 105.3430358795248338, -8.402594152722688392, -9.854619843455216355 ) ) ;
#41064 = DIRECTION ( 'NONE',  ( -1.000000000000000000, 0.000000000000000000, 0.000000000000000000 ) ) ;
#41065 = CARTESIAN_POINT ( 'NONE',  ( 118.3554748109119998, 0.2603800115204892296, -16.42320221600525088 ) ) ;
#41066 = ORIENTED_EDGE ( 'NONE', *, *, #7862, .F. ) ;
#41067 = CARTESIAN_POINT ( 'NONE',  ( 124.7655881442452852, 0.5811942927096110934, -14.16772938898807510 ) ) ;
#41068 = CARTESIAN_POINT ( 'NONE',  ( 121.0024232127138504, -2.191907684172563986, -18.20049396185734025 ) ) ;
#41069 = CARTESIAN_POINT ( 'NONE',  ( 118.6958348109119754, -3.505236298600246325, -18.68346056562440793 ) ) ;
#41070 = CARTESIAN_POINT ( 'NONE',  ( 67.69189222814998175, -49.76310523276723785, -34.89321520033831092 ) ) ;
#41071 = CARTESIAN_POINT ( 'NONE',  ( 122.3263414775786373, -6.344957434206665248, -7.627207830600338134 ) ) ;
#41072 = AXIS2_PLACEMENT_3D ( 'NONE', #5668, #30524, #9330 ) ;
#41073 = CARTESIAN_POINT ( 'NONE',  ( 115.8999108795247821, -1.325403438956436419, -16.93181055722141792 ) ) ;
#41074 = CARTESIAN_POINT ( 'NONE',  ( 89.27809288332949222, -9.952843041749929398, -13.58709681493693644 ) ) ;
#41075 = ORIENTED_EDGE ( 'NONE', *, *, #4943, .F. ) ;
#41076 = CARTESIAN_POINT ( 'NONE',  ( 111.7751814775786556, -7.893985811506177619, -18.51759400769804742 ) ) ;
#41077 = CARTESIAN_POINT ( 'NONE',  ( 124.2550481442452792, -0.1624402480850797581, -16.17319339645315424 ) ) ;
#41078 = AXIS2_PLACEMENT_3D ( 'NONE', #22424, #19002, #8739 ) ;
#41079 = CARTESIAN_POINT ( 'NONE',  ( 121.1350814775786233, 0.5811942927096110934, -14.16772938898807510 ) ) ;
#41080 = CARTESIAN_POINT ( 'NONE',  ( 113.0231681442453180, -10.15424416112533912, -14.75197769757731336 ) ) ;
#41081 = CARTESIAN_POINT ( 'NONE',  ( 119.1496481442453046, -3.383040157471821630, -19.15922257007629170 ) ) ;
#41082 = CARTESIAN_POINT ( 'NONE',  ( 123.3116793777725064, -1.267766418764731728, -16.93314635290706605 ) ) ;
#41083 = CARTESIAN_POINT ( 'NONE',  ( 126.6211808763518576, -1.201114777694167746, -9.700051355915984885 ) ) ;
#41084 = CARTESIAN_POINT ( 'NONE',  ( 124.4252281442452812, -0.8288870151387760510, -10.36305467784173118 ) ) ;
#41085 = EDGE_LOOP ( 'NONE', ( #13690, #4992, #26066, #17325 ) ) ;
#41086 = CARTESIAN_POINT ( 'NONE',  ( 122.4521266859119635, -0.06289925094097943703, -9.412459353600674206 ) ) ;
#41087 = VECTOR ( 'NONE', #18142, 1000.000000000000000 ) ;
#41088 = CARTESIAN_POINT ( 'NONE',  ( 116.8238548109119819, -4.089484607189486809, -7.948022111789456723 ) ) ;
#41089 = CARTESIAN_POINT ( 'NONE',  ( 119.9438214775786378, -2.084020599724406786, -8.691656652584148546 ) ) ;
#41090 = ORIENTED_EDGE ( 'NONE', *, *, #43156, .F. ) ;
#41091 = CARTESIAN_POINT ( 'NONE',  ( 121.6186891859119896, -1.406689858478933353, -17.56299727309130887 ) ) ;
#41092 = CARTESIAN_POINT ( 'NONE',  ( 137.3802547664329552, -0.4074658335668200904, -10.83275452620230084 ) ) ;
#41093 = CARTESIAN_POINT ( 'NONE',  ( 118.9227414775786400, -10.63000616557722466, -14.87417383870573495 ) ) ;
#41094 = CARTESIAN_POINT ( 'NONE',  ( 112.1494421295248003, 0.8980012041604618078, -13.39321520033831447 ) ) ;
#41095 = CARTESIAN_POINT ( 'NONE',  ( 117.2776681442452968, -4.153390946401321671, -8.397313243818183892 ) ) ;
#41096 = ORIENTED_EDGE ( 'NONE', *, *, #32620, .F. ) ;
#41097 = VERTEX_POINT ( 'NONE', #5807 ) ;
#41098 = CARTESIAN_POINT ( 'NONE',  ( 112.5693548109119888, -10.63000616557722466, -14.87417383870573495 ) ) ;
#41099 = ADVANCED_FACE ( 'NONE', ( #26800, #6035, #43672 ), #40256, .F. ) ;
#41100 = CARTESIAN_POINT ( 'NONE',  ( 78.69189222814998175, -60.26310523276723785, -29.64311716074571379 ) ) ;
#41101 = DIRECTION ( 'NONE',  ( 0.9609149988134837450, -0.1028163501681639419, 0.2570431154366518145 ) ) ;
#41102 = DIRECTION ( 'NONE',  ( -0.000000000000000000, -0.9284778069183721172, -0.3713878862591650232 ) ) ;
#41103 = CARTESIAN_POINT ( 'NONE',  ( 122.8368814775786291, -1.561330072975668948, -17.79121239304076951 ) ) ;
#41104 = LINE ( 'NONE', #9862, #10231 ) ;
#41105 = CARTESIAN_POINT ( 'NONE',  ( 70.97035005826803911, 2.261436620216128013, -16.39321520033831447 ) ) ;
#41106 = CARTESIAN_POINT ( 'NONE',  ( 121.6456214775786293, -10.63000616557722466, -14.87417383870573495 ) ) ;
#41108 = CARTESIAN_POINT ( 'NONE',  ( 119.7169148109119874, -0.1624402480850797581, -16.17319339645315424 ) ) ;
#41107 = CARTESIAN_POINT ( 'NONE',  ( 118.1852948109119836, -5.638512984488999180, -18.83840828888717311 ) ) ;
#41109 = CARTESIAN_POINT ( 'NONE',  ( 123.8012348109119642, -9.565557343593413364, -10.61323700422348004 ) ) ;
#41110 = CARTESIAN_POINT ( 'NONE',  ( 112.3023386403692427, -1.196538596002803212, -17.02799684832027438 ) ) ;
#41111 = VERTEX_POINT ( 'NONE', #15635 ) ;
#41112 = CARTESIAN_POINT ( 'NONE',  ( 122.5532481442453019, 0.4262465694468514643, -12.03445270309931736 ) ) ;
#41113 = CARTESIAN_POINT ( 'NONE',  ( 122.1683934719562075, -1.125321370491285444, -17.12283323191017814 ) ) ;
#41114 = CARTESIAN_POINT ( 'NONE',  ( 120.9114422641554540, -8.548534124195553474, -17.65096007659764510 ) ) ;
#41115 = CARTESIAN_POINT ( 'NONE',  ( 109.9269421295247753, 0.8980012041604618078, -13.39321520033831447 ) ) ;
#41116 = CARTESIAN_POINT ( 'NONE',  ( 111.5243640045248412, 0.1403307496149616695, -15.46607636864997204 ) ) ;
#41117 = CARTESIAN_POINT ( 'NONE',  ( 116.0388171295248014, 0.1403307496149613920, -13.39321520033831447 ) ) ;
#41118 = CARTESIAN_POINT ( 'NONE',  ( 123.1205148109119563, -1.834011780172310813, -8.268836392978581529 ) ) ;
#41119 = CARTESIAN_POINT ( 'NONE',  ( 121.2485348109119769, -8.899110576539710493, -16.42337572283490132 ) ) ;
#41120 = ORIENTED_EDGE ( 'NONE', *, *, #41198, .F. ) ;
#41121 = CARTESIAN_POINT ( 'NONE',  ( 125.6732148109119862, 0.5811942927096110934, -14.16772938898807510 ) ) ;
#41122 = CARTESIAN_POINT ( 'NONE',  ( 112.5693548109119888, 0.4262465694468514643, -12.03445270309931736 ) ) ;
#41123 = CARTESIAN_POINT ( 'NONE',  ( 121.8725281442452939, -6.222761293078261424, -8.102969835052221015 ) ) ;
#41124 = CARTESIAN_POINT ( 'NONE',  ( 118.4689281442453392, 0.9020085738987339008, -11.91225656197089222 ) ) ;
#41125 = CARTESIAN_POINT ( 'NONE',  ( 121.0783548109119749, 0.2603800115204892296, -16.42320221600525088 ) ) ;
#41126 = CARTESIAN_POINT ( 'NONE',  ( 120.2990798109119766, -7.200787124940443817, -17.81845355600750835 ) ) ;
#41127 = CARTESIAN_POINT ( 'NONE',  ( 113.0798948109119948, -0.4660016031367893996, -10.09054647747474043 ) ) ;
#41128 = CARTESIAN_POINT ( 'NONE',  ( 122.4521266859119635, -9.033780868592240054, -16.85052413769862056 ) ) ;
#41129 = CARTESIAN_POINT ( 'NONE',  ( 115.5526452545247622, -9.868328341294098749, -15.46607636864997204 ) ) ;
#41130 = AXIS2_PLACEMENT_3D ( 'NONE', #29688, #43600, #40180 ) ;
#41131 = EDGE_LOOP ( 'NONE', ( #6476, #9387, #42928, #13792, #17351 ) ) ;
#41132 = DIRECTION ( 'NONE',  ( 0.9063289528979890930, 0.4225728684367167087, 0.000000000000000000 ) ) ;
#41133 = CARTESIAN_POINT ( 'NONE',  ( 118.7735460444391862, -1.267766418764730840, -16.93314635290706605 ) ) ;
#41134 = CARTESIAN_POINT ( 'NONE',  ( 125.2761281442453054, 0.4262465694468514643, -12.03445270309931736 ) ) ;
#41135 = CARTESIAN_POINT ( 'NONE',  ( 106.3848327545248651, -6.936859964151250502, -8.388885654883777576 ) ) ;
#41136 = CARTESIAN_POINT ( 'NONE',  ( 112.5661608795247872, -1.325403438956436419, -16.93181055722141792 ) ) ;
#41137 = CARTESIAN_POINT ( 'NONE',  ( 121.9292548109119849, -7.894159318335828068, -9.358103419637847864 ) ) ;
#41138 = CARTESIAN_POINT ( 'NONE',  ( 116.5402214775786405, -9.565557343593413364, -10.61323700422348004 ) ) ;
#41139 = CARTESIAN_POINT ( 'NONE',  ( 122.3830681442452857, -8.166667518702819706, -8.995218007635861213 ) ) ;
#41140 = ORIENTED_EDGE ( 'NONE', *, *, #19090, .F. ) ;
#41141 = AXIS2_PLACEMENT_3D ( 'NONE', #4511, #42155, #32544 ) ;
#41142 = CARTESIAN_POINT ( 'NONE',  ( 123.3474214775786209, -0.1624402480850797581, -16.17319339645315424 ) ) ;
#41143 = CARTESIAN_POINT ( 'NONE',  ( 116.9940348109119839, -9.988377603198976828, -10.36322818467138340 ) ) ;
#41144 = CARTESIAN_POINT ( 'NONE',  ( 123.9146881442452894, 0.9020085738987339008, -11.91225656197089222 ) ) ;
#41145 = CARTESIAN_POINT ( 'NONE',  ( 121.8725281442453223, -6.222761293078241884, -8.102969835052219238 ) ) ;
#41146 = ORIENTED_EDGE ( 'NONE', *, *, #43987, .T. ) ;
#41147 = CARTESIAN_POINT ( 'NONE',  ( 123.7253032127138397, -2.191907684172563986, -18.20049396185734025 ) ) ;
#41148 = CARTESIAN_POINT ( 'NONE',  ( 125.6732148109119862, 0.5811942927096110934, -14.16772938898807510 ) ) ;
#41149 = CARTESIAN_POINT ( 'NONE',  ( 113.7038881442453402, -6.222761293078241884, -8.102969835052219238 ) ) ;
#41150 = CARTESIAN_POINT ( 'NONE',  ( 124.2550481442452792, -9.988377603198980381, -10.36322818467138518 ) ) ;
#41151 = CARTESIAN_POINT ( 'NONE',  ( 123.8328548109119822, -4.863998795839244771, -13.39321520033831625 ) ) ;
#41152 = CARTESIAN_POINT ( 'NONE',  ( 122.7993923109119692, -0.4387604401700512802, -15.73000352943951619 ) ) ;
#41153 = ORIENTED_EDGE ( 'NONE', *, *, #11621, .F. ) ;
#41154 = DIRECTION ( 'NONE',  ( -0.000000000000000000, -0.9284778069183720062, -0.3713878862591650232 ) ) ;
#41155 = CARTESIAN_POINT ( 'NONE',  ( 125.2183010572621669, 2.324478367502957443, -12.03255835460978318 ) ) ;
#41156 = CARTESIAN_POINT ( 'NONE',  ( 115.8304577545247582, -7.250697342233347165, -7.631215200338321125 ) ) ;
#41157 = DIRECTION ( 'NONE',  ( 0.000000000000000000, -0.9242245927363029745, -0.3818493186865927758 ) ) ;
#41158 = CARTESIAN_POINT ( 'NONE',  ( 124.1983214775786166, -1.833838273342659697, -17.42832698103878286 ) ) ;
#41159 = CARTESIAN_POINT ( 'NONE',  ( 115.4056881442453459, -2.084020599724406786, -8.691656652584148546 ) ) ;
#41160 = CARTESIAN_POINT ( 'NONE',  ( 126.2184548109119788, -5.568102603702699049, -18.34339073538272302 ) ) ;
#41161 = ADVANCED_BREP_SHAPE_REPRESENTATION ( '', ( #6587, #12375 ), #21301 ) ;
#41162 = VERTEX_POINT ( 'NONE', #29539 ) ;
#41163 = CARTESIAN_POINT ( 'NONE',  ( 119.7434548109119703, -2.316996251443989241, -21.63995271010855248 ) ) ;
#41164 = AXIS2_PLACEMENT_3D ( 'NONE', #30034, #19095, #15911 ) ;
#41165 = CARTESIAN_POINT ( 'NONE',  ( 116.4597320646196863, 0.6269505268395592079, -14.64321520033831447 ) ) ;
#41166 = DIRECTION ( 'NONE',  ( 0.000000000000000000, 0.000000000000000000, -1.000000000000000000 ) ) ;
#41167 = CARTESIAN_POINT ( 'NONE',  ( 111.7751814775786556, -2.084020599724406786, -8.691656652584148546 ) ) ;
#41169 = CARTESIAN_POINT ( 'NONE',  ( 124.7088614775786226, 0.2603800115204892296, -16.42320221600525088 ) ) ;
#41168 = CARTESIAN_POINT ( 'NONE',  ( 92.32016463086877422, -25.99489077589524300, -13.39321520033831447 ) ) ;
#41170 = CARTESIAN_POINT ( 'NONE',  ( 125.5030348109119558, -6.222761293078241884, -8.102969835052219238 ) ) ;
#41171 = ORIENTED_EDGE ( 'NONE', *, *, #32554, .F. ) ;
#41172 = CARTESIAN_POINT ( 'NONE',  ( 114.1009748109119784, -4.089484607189486809, -7.948022111789456723 ) ) ;
#41173 = CARTESIAN_POINT ( 'NONE',  ( 127.0150841466606551, 0.2316552957976503180, -15.17538186860604732 ) ) ;
#41174 = CARTESIAN_POINT ( 'NONE',  ( 106.5237390045248418, -9.868328341294098749, -11.32035403202665869 ) ) ;
#41175 = CARTESIAN_POINT ( 'NONE',  ( 123.6877814775786533, -6.222761293078241884, -8.102969835052219238 ) ) ;
#41176 = CARTESIAN_POINT ( 'NONE',  ( 121.8158014775786171, -4.153390946401325223, -8.397313243818185668 ) ) ;
#41177 = DIRECTION ( 'NONE',  ( -0.000000000000000000, -0.9284778069183718952, -0.3713878862591649677 ) ) ;
#41178 = CARTESIAN_POINT ( 'NONE',  ( 114.2330358795247776, -8.402594152722688392, -9.854619843455216355 ) ) ;
#41179 = CARTESIAN_POINT ( 'NONE',  ( 111.9410827545248708, -2.477300249445798297, -19.15521520033830427 ) ) ;
#41180 = CARTESIAN_POINT ( 'NONE',  ( 67.30914723170953096, -56.02262229671700311, -36.50637067845163841 ) ) ;
#41181 = CARTESIAN_POINT ( 'NONE',  ( 113.8173414775786512, -9.565557343593413364, -10.61323700422348004 ) ) ;
#41182 = CARTESIAN_POINT ( 'NONE',  ( 106.4542858795248179, -0.7896495226426338832, -17.46756447353520159 ) ) ;
#41183 = AXIS2_PLACEMENT_3D ( 'NONE', #40487, #9246, #36362 ) ;
#41184 = LINE ( 'NONE', #10389, #42272 ) ;
#41185 = CARTESIAN_POINT ( 'NONE',  ( 114.5108483795247878, -0.7896495226426338832, -9.318865927141430916 ) ) ;
#41186 = CARTESIAN_POINT ( 'NONE',  ( 126.1837548109119211, -10.63000616557722466, -14.87417383870573495 ) ) ;
#41187 = CARTESIAN_POINT ( 'NONE',  ( 120.2841814775786276, 0.9020085738987339008, -11.91225656197089222 ) ) ;
#41188 = CARTESIAN_POINT ( 'NONE',  ( 110.2184548109119788, -5.044325091639137781, -11.90409383958792411 ) ) ;
#41189 = CARTESIAN_POINT ( 'NONE',  ( 120.1707281442453166, 0.2603800115204892296, -16.42320221600525088 ) ) ;
#41190 = ADVANCED_FACE ( 'NONE', ( #43455 ), #44639, .T. ) ;
#41191 = CARTESIAN_POINT ( 'NONE',  ( 112.9097148109120070, 0.2603800115204892296, -16.42320221600525088 ) ) ;
#41192 = ORIENTED_EDGE ( 'NONE', *, *, #10274, .F. ) ;
#41193 = VECTOR ( 'NONE', #14272, 1000.000000000000000 ) ;
#41194 = CARTESIAN_POINT ( 'NONE',  ( 125.2194014775786286, -10.30919188438810075, -12.61870101168855918 ) ) ;
#41195 = CARTESIAN_POINT ( 'NONE',  ( 124.6521348109119884, -1.561330072975668948, -17.79121239304076951 ) ) ;
#41196 = CARTESIAN_POINT ( 'NONE',  ( 114.1009748109119784, -4.089484607189486809, -7.948022111789456723 ) ) ;
#41197 = CARTESIAN_POINT ( 'NONE',  ( 126.0703014775786102, -9.988377603198980381, -10.36322818467138518 ) ) ;
#41198 = EDGE_CURVE ( 'NONE', #10961, #42332, #20115, .T. ) ;
#41199 = VERTEX_POINT ( 'NONE', #32944 ) ;
#41200 = CARTESIAN_POINT ( 'NONE',  ( 117.6180281442453150, -8.899110576539710493, -16.42337572283490132 ) ) ;
#41201 = CIRCLE ( 'NONE', #8400, 1.200000000000000622 ) ;
#41202 = CARTESIAN_POINT ( 'NONE',  ( 113.1933481442453058, -4.089484607189486809, -7.948022111789456723 ) ) ;
#41203 = CARTESIAN_POINT ( 'NONE',  ( 123.2339681442453241, -3.505236298600246325, -18.68346056562440793 ) ) ;
#41204 = CARTESIAN_POINT ( 'NONE',  ( 116.8537841442347656, -0.5650535969755431376, -16.42331166093997652 ) ) ;
#41205 = CARTESIAN_POINT ( 'NONE',  ( 115.4137390045248566, 0.8980012041604421569, -15.77991374673208469 ) ) ;
#41206 = EDGE_LOOP ( 'NONE', ( #29731, #29047, #6416, #41558, #41146, #36767, #8057, #10353 ) ) ;
#41207 = CARTESIAN_POINT ( 'NONE',  ( 62.38867158002533841, -1.739742509014211791, -9.130636672632755690 ) ) ;
#41208 = CARTESIAN_POINT ( 'NONE',  ( 112.9810566399283829, 0.4261359969231631739, -14.64321520033830026 ) ) ;
#41209 = EDGE_CURVE ( 'NONE', #40056, #27343, #33619, .T. ) ;
#41210 = CARTESIAN_POINT ( 'NONE',  ( 125.4584548109119737, -4.863998795839242995, -13.39321520033831447 ) ) ;
#41211 =( NAMED_UNIT ( * ) SI_UNIT ( $, .STERADIAN. ) SOLID_ANGLE_UNIT ( ) );
#41212 = CARTESIAN_POINT ( 'NONE',  ( 117.0960808822395478, 1.608673864571572798, -5.427676334679006231 ) ) ;
#41213 = CARTESIAN_POINT ( 'NONE',  ( 112.2289948109119848, -7.643976991954077427, -18.09477374809248928 ) ) ;
#41214 = EDGE_CURVE ( 'NONE', #7248, #2572, #21534, .T. ) ;
#41215 = CARTESIAN_POINT ( 'NONE',  ( 105.3430358795248338, -8.402594152722688392, -9.854619843455216355 ) ) ;
#41216 = CARTESIAN_POINT ( 'NONE',  ( 111.3598964071292841, 0.2518737723193609224, -14.64321520033828783 ) ) ;
#41217 = CARTESIAN_POINT ( 'NONE',  ( 119.8303681442453126, -10.63000616557722466, -14.87417383870573495 ) ) ;
#41218 = CARTESIAN_POINT ( 'NONE',  ( 137.0223538766786646, -4.519491365511462355, -18.82947256965501381 ) ) ;
#41219 = EDGE_CURVE ( 'NONE', #33252, #8541, #19965, .T. ) ;
#41220 = CONICAL_SURFACE ( 'NONE', #12108, 2.445500000000004448, 0.9599310885968757034 ) ;
#41221 = CARTESIAN_POINT ( 'NONE',  ( 125.0849635773846842, -2.467220198597905867, -17.83387418641800437 ) ) ;
#41222 = CARTESIAN_POINT ( 'NONE',  ( 123.6328298109119714, -7.200787124940195127, -17.81845355600763625 ) ) ;
#41223 = CARTESIAN_POINT ( 'NONE',  ( 120.7379948109119709, 0.4262465694468514643, -12.03445270309931736 ) ) ;
#41224 = ORIENTED_EDGE ( 'NONE', *, *, #32785, .T. ) ;
#41225 = DIRECTION ( 'NONE',  ( -0.1352586133457950590, -0.9908103287288504424, 0.000000000000000000 ) ) ;
#41226 = CARTESIAN_POINT ( 'NONE',  ( 118.2987481442453088, -1.561330072975668504, -17.79121239304076951 ) ) ;
#41227 = DIRECTION ( 'NONE',  ( 1.000000000000000000, 0.000000000000000000, -0.000000000000000000 ) ) ;
#41228 = CARTESIAN_POINT ( 'NONE',  ( 116.4834948109119779, -7.894159318335828068, -9.358103419637847864 ) ) ;
#41229 = ADVANCED_FACE ( 'NONE', ( #8795 ), #8447, .F. ) ;
#41230 = CARTESIAN_POINT ( 'NONE',  ( 113.4202548109119846, 0.1319031606808879209, -14.10382304977623669 ) ) ;
#41231 = CARTESIAN_POINT ( 'NONE',  ( 109.3713171295247832, -10.62599879583958540, -13.39321520033831447 ) ) ;
#41232 = CARTESIAN_POINT ( 'NONE',  ( 106.5931921295248372, -9.868328341294093420, -13.39321520033831447 ) ) ;
#41233 = CARTESIAN_POINT ( 'NONE',  ( 115.7610046295247912, -4.863998795839590272, -7.631215200338315796 ) ) ;
#41234 = CARTESIAN_POINT ( 'NONE',  ( 117.7882081442453170, -3.505236298600246325, -18.68346056562440793 ) ) ;
#41235 = CARTESIAN_POINT ( 'NONE',  ( 119.4900081442453086, -7.643976991954077427, -18.09477374809248928 ) ) ;
#41236 = CARTESIAN_POINT ( 'NONE',  ( 109.2294580127160941, -8.142638662055460941, -8.698686866961791608 ) ) ;
#41237 = CARTESIAN_POINT ( 'NONE',  ( 112.7491510812576934, -0.01829820670803256055, -12.14321520033831625 ) ) ;
#41238 = CARTESIAN_POINT ( 'NONE',  ( 108.5378796295247810, -4.863998795839590272, -8.388885654883775800 ) ) ;
#41239 = ORIENTED_EDGE ( 'NONE', *, *, #20325, .T. ) ;
#41240 = EDGE_CURVE ( 'NONE', #38837, #38458, #1721, .T. ) ;
#41241 = FACE_OUTER_BOUND ( 'NONE', #18822, .T. ) ;
#41242 = CARTESIAN_POINT ( 'NONE',  ( 112.5693548109119888, -10.63000616557722466, -14.87417383870573495 ) ) ;
#41243 = DIRECTION ( 'NONE',  ( 0.000000000000000000, 0.2950959089608259922, -0.9554676365605399013 ) ) ;
#41244 = CARTESIAN_POINT ( 'NONE',  ( 46.84966980880212617, -19.07391775237791620, -8.593215200338315540 ) ) ;
#41245 = CARTESIAN_POINT ( 'NONE',  ( 119.8823610609119754, -6.340755971794695078, -8.611740276972781771 ) ) ;
#41246 = ADVANCED_FACE ( 'NONE', ( #40718 ), #13132, .T. ) ;
#41247 = EDGE_CURVE ( 'NONE', #34939, #4744, #17891, .T. ) ;
#41248 = ORIENTED_EDGE ( 'NONE', *, *, #12380, .F. ) ;
#41249 = CARTESIAN_POINT ( 'NONE',  ( 123.5909359023132907, -3.144421331627774041, -14.43411955300261340 ) ) ;
#41250 = ORIENTED_EDGE ( 'NONE', *, *, #20325, .F. ) ;
#41251 = CARTESIAN_POINT ( 'NONE',  ( 123.2339681442453241, -6.344957434206665248, -7.627207830600338134 ) ) ;
#41252 = CARTESIAN_POINT ( 'NONE',  ( 113.0231681442453322, 0.9020085738987339008, -11.91225656197089222 ) ) ;
#41253 = CARTESIAN_POINT ( 'NONE',  ( 120.1707281442453166, -9.565557343593413364, -10.61323700422348004 ) ) ;
#41254 = CIRCLE ( 'NONE', #18670, 10.00000000000000178 ) ;
#41255 = SURFACE_STYLE_USAGE ( .BOTH. , #40792 ) ;
#41256 = CARTESIAN_POINT ( 'NONE',  ( 70.19189222814998175, -65.04786711941001442, -39.22192925582032785 ) ) ;
#41257 = CARTESIAN_POINT ( 'NONE',  ( 121.1918081442452859, 0.9020085738987339008, -11.91225656197089222 ) ) ;
#41258 = CARTESIAN_POINT ( 'NONE',  ( 119.3765548109119834, 0.9020085738987339008, -11.91225656197089222 ) ) ;
#41259 = AXIS2_PLACEMENT_3D ( 'NONE', #30940, #20005, #33891 ) ;
#41260 = CARTESIAN_POINT ( 'NONE',  ( 116.3166296295247832, -4.863998795839590272, -19.15521520033831493 ) ) ;
#41261 = CARTESIAN_POINT ( 'NONE',  ( 113.7038881442453402, -6.222761293078241884, -8.102969835052219238 ) ) ;
#41262 = PLANE ( 'NONE',  #41050 ) ;
#41263 = ORIENTED_EDGE ( 'NONE', *, *, #25117, .T. ) ;
#41264 = CARTESIAN_POINT ( 'NONE',  ( 116.8805814775786445, -6.344957434206662583, -7.627207830600332805 ) ) ;
#41265 = AXIS2_PLACEMENT_3D ( 'NONE', #18687, #33189, #15730 ) ;
#41266 = CARTESIAN_POINT ( 'NONE',  ( 121.3408766859119794, -0.06289925094097943703, -9.412459353600674206 ) ) ;
#41267 = CARTESIAN_POINT ( 'NONE',  ( 116.0864081442453113, -9.988377603198976828, -10.36322818467138340 ) ) ;
#41268 = VERTEX_POINT ( 'NONE', #43464 ) ;
#41269 = CARTESIAN_POINT ( 'NONE',  ( 126.0135748109119902, -8.166667518702819706, -8.995218007635861213 ) ) ;
#41270 = LINE ( 'NONE', #10030, #20169 ) ;
#41271 = DIRECTION ( 'NONE',  ( 0.5040994586965589219, 0.8636456077245088236, 0.000000000000000000 ) ) ;
#41272 = CARTESIAN_POINT ( 'NONE',  ( 119.7434548109119703, -4.863998795839242995, -13.39321520033831447 ) ) ;
#41273 = CARTESIAN_POINT ( 'NONE',  ( 114.8951481442453115, -8.899110576539710493, -16.42337572283490132 ) ) ;
#41274 = DIRECTION ( 'NONE',  ( -0.07634843047859418697, -0.9970811988817437355, 0.000000000000000000 ) ) ;
#41275 = CARTESIAN_POINT ( 'NONE',  ( 118.8092881442453290, -0.1624402480850797581, -16.17319339645315424 ) ) ;
#41276 = CARTESIAN_POINT ( 'NONE',  ( 70.19189222814998175, -60.97346038181336070, -37.59218076343751136 ) ) ;
#41277 = AXIS2_PLACEMENT_3D ( 'NONE', #33748, #27381, #24401 ) ;
#41278 = CARTESIAN_POINT ( 'NONE',  ( 115.1787814775786387, -0.1624402480850797581, -16.17319339645315424 ) ) ;
#41279 = CARTESIAN_POINT ( 'NONE',  ( 116.9373081442452929, -8.166667518702817929, -8.995218007635861213 ) ) ;
#41280 = CARTESIAN_POINT ( 'NONE',  ( 120.5768923109119868, -9.959231468620755479, -10.70263013195267199 ) ) ;
#41281 = CARTESIAN_POINT ( 'NONE',  ( 117.5045748109119756, 0.5811942927096110934, -14.16772938898807510 ) ) ;
#41282 = CARTESIAN_POINT ( 'NONE',  ( 112.2857214775786474, -5.574606645277164318, -18.38911715685844683 ) ) ;
#41283 = CARTESIAN_POINT ( 'NONE',  ( 117.1642148109119859, -0.8288870151387760510, -10.36305467784173118 ) ) ;
#41284 = ORIENTED_EDGE ( 'NONE', *, *, #22779, .F. ) ;
#41285 = CARTESIAN_POINT ( 'NONE',  ( 112.1722681442453222, -0.4660016031367893996, -10.09054647747474043 ) ) ;
#41286 = EDGE_CURVE ( 'NONE', #9213, #31092, #25892, .T. ) ;
#41287 = CARTESIAN_POINT ( 'NONE',  ( 106.8710046295248759, -4.863998795839590272, -7.631215200338315796 ) ) ;
#41288 = AXIS2_PLACEMENT_3D ( 'NONE', #32427, #10800, #24696 ) ;
#41289 = CARTESIAN_POINT ( 'NONE',  ( 105.0652233795248378, -1.325403438956436419, -9.854619843455211026 ) ) ;
#41290 = CARTESIAN_POINT ( 'NONE',  ( 105.5513952545248060, -9.868328341294098749, -15.46607636864997204 ) ) ;
#41291 = CARTESIAN_POINT ( 'NONE',  ( 64.46535740945334680, -37.09977221485072363, -5.366017974039236194 ) ) ;
#41292 = CARTESIAN_POINT ( 'NONE',  ( 118.9227414775786400, -10.63000616557722466, -14.87417383870573495 ) ) ;
#41293 = ORIENTED_EDGE ( 'NONE', *, *, #31181, .F. ) ;
#41294 = DIRECTION ( 'NONE',  ( 1.000000000000000000, 0.000000000000000000, 0.000000000000000000 ) ) ;
#41295 = CARTESIAN_POINT ( 'NONE',  ( 118.5823814775786360, -7.643976991954077427, -18.09477374809248928 ) ) ;
#41296 = CARTESIAN_POINT ( 'NONE',  ( 124.2666781415389039, -0.1020945015694913471, -15.74893487844866691 ) ) ;
#41297 = EDGE_CURVE ( 'NONE', #9382, #18860, #33159, .T. ) ;
#41298 = VECTOR ( 'NONE', #10910, 1000.000000000000000 ) ;
#41299 = CARTESIAN_POINT ( 'NONE',  ( 121.8158014775786171, -5.638512984488999180, -18.83840828888717311 ) ) ;
#41300 = CARTESIAN_POINT ( 'NONE',  ( 106.1070202545248407, -10.62599879583958717, -15.77991374673208469 ) ) ;
#41301 = CARTESIAN_POINT ( 'NONE',  ( 124.3640859692789462, -1.179503403430468333, -17.05068175419387089 ) ) ;
#41302 = ORIENTED_EDGE ( 'NONE', *, *, #41794, .F. ) ;
#41303 = DIRECTION ( 'NONE',  ( -1.000000000000000000, 0.000000000000000000, 0.000000000000000000 ) ) ;
#41304 = CARTESIAN_POINT ( 'NONE',  ( 122.8936081442453059, -9.565557343593413364, -10.61323700422348004 ) ) ;
#41305 = CARTESIAN_POINT ( 'NONE',  ( 125.1059481442452750, -8.166667518702819706, -8.995218007635861213 ) ) ;
#41306 = EDGE_CURVE ( 'NONE', #9168, #930, #38278, .T. ) ;
#41307 = CARTESIAN_POINT ( 'NONE',  ( 118.4689281442453392, -10.15424416112533912, -14.75197769757731336 ) ) ;
#41308 = CARTESIAN_POINT ( 'NONE',  ( 119.0929214775786278, -5.638512984488999180, -18.83840828888717311 ) ) ;
#41309 = CARTESIAN_POINT ( 'NONE',  ( 76.69189222814998175, -50.16718729050181480, -6.893215200338315363 ) ) ;
#41310 = EDGE_CURVE ( 'NONE', #35058, #19992, #36598, .T. ) ;
#41311 = CARTESIAN_POINT ( 'NONE',  ( 126.6827570900246656, -1.214894069026291934, -9.643484958278310870 ) ) ;
#41312 = CARTESIAN_POINT ( 'NONE',  ( 121.5888948109119809, 0.1319031606808879209, -14.10382304977623669 ) ) ;
#41313 = ORIENTED_EDGE ( 'NONE', *, *, #29837, .F. ) ;
#41314 = CARTESIAN_POINT ( 'NONE',  ( 116.5949565311550913, -9.864074739043591222, -13.32529961072451741 ) ) ;
#41315 = AXIS2_PLACEMENT_3D ( 'NONE', #7638, #17686, #31584 ) ;
#41316 = CARTESIAN_POINT ( 'NONE',  ( 116.7104014775786425, -0.4660016031367893996, -10.09054647747474043 ) ) ;
#41317 = CARTESIAN_POINT ( 'NONE',  ( 125.5597614775786326, -7.894159318335828068, -9.358103419637847864 ) ) ;
#41318 = VERTEX_POINT ( 'NONE', #44370 ) ;
#41319 = CARTESIAN_POINT ( 'NONE',  ( 123.4244704359119709, 1.345710702986147034, -13.97328579221134426 ) ) ;
#41320 = CARTESIAN_POINT ( 'NONE',  ( 135.4522060580625293, -1.191823701641487432, -8.648235046535946324 ) ) ;
#41321 = CARTESIAN_POINT ( 'NONE',  ( 123.0070614775786169, 0.9020085738987339008, -11.91225656197089222 ) ) ;
#41322 = CARTESIAN_POINT ( 'NONE',  ( 107.2877233795247776, -8.938348069036489818, -17.46756447353520159 ) ) ;
#41323 = CARTESIAN_POINT ( 'NONE',  ( 119.8870948109119752, -0.8288870151387760510, -10.36305467784173118 ) ) ;
#41324 = AXIS2_PLACEMENT_3D ( 'NONE', #36632, #5623, #26613 ) ;
#41325 = VERTEX_POINT ( 'NONE', #33390 ) ;
#41326 = VERTEX_POINT ( 'NONE', #33170 ) ;
#41327 = CARTESIAN_POINT ( 'NONE',  ( 125.9001214775786224, -5.574606645277164318, -18.38911715685844683 ) ) ;
#41328 = CARTESIAN_POINT ( 'NONE',  ( 124.1983214775786166, -1.833838273342659697, -17.42832698103878286 ) ) ;
#41329 = CARTESIAN_POINT ( 'NONE',  ( 69.69189222814998175, -41.76310523276723785, -6.393215200338315363 ) ) ;
#41330 = VECTOR ( 'NONE', #33212, 1000.000000000000000 ) ;
#41331 = DIRECTION ( 'NONE',  ( 0.000000000000000000, 0.000000000000000000, 1.000000000000000000 ) ) ;
#41332 = CARTESIAN_POINT ( 'NONE',  ( 121.9292548109119849, -1.561330072975668948, -17.79121239304076951 ) ) ;
#41333 = DIRECTION ( 'NONE',  ( 1.591814108749227602E-14, -1.000000000000000000, 0.000000000000000000 ) ) ;
#41334 = DIRECTION ( 'NONE',  ( 0.5735764363510498232, -0.3127926500124802445, 0.7570804645221007600 ) ) ;
#41335 = CARTESIAN_POINT ( 'NONE',  ( 119.7736414775786358, -10.30919188438810075, -12.61870101168855918 ) ) ;
#41337 = CARTESIAN_POINT ( 'NONE',  ( 120.8514481442452961, -2.084020599724406786, -8.691656652584148546 ) ) ;
#41336 = CARTESIAN_POINT ( 'NONE',  ( 118.8660148109119774, -10.30919188438810075, -12.61870101168855918 ) ) ;
#41338 = DIRECTION ( 'NONE',  ( 0.9609149988134843001, -0.1028163501681632064, 0.2570431154366505933 ) ) ;
#41339 = CARTESIAN_POINT ( 'NONE',  ( 116.3700414775786527, -5.638512984488999180, -18.83840828888717311 ) ) ;
#41340 = B_SPLINE_CURVE_WITH_KNOTS ( 'NONE', 3,
 ( #19050, #43226, #29760, #39799, #8568, #33611, #40710, #37264, #5366, #44139 ),
 .UNSPECIFIED., .F., .F.,
 ( 4, 3, 3, 4 ),
 ( 0.000000000000000000, 0.0002476487219222709845, 0.0004952974148303440237, 0.0009534114850261750764 ),
 .UNSPECIFIED. ) ;
#41341 = VERTEX_POINT ( 'NONE', #9029 ) ;
#41342 = ADVANCED_FACE ( 'NONE', ( #37044 ), #40495, .T. ) ;
#41343 = CARTESIAN_POINT ( 'NONE',  ( 122.8368814775786291, -7.894159318335828068, -9.358103419637847864 ) ) ;
#41344 = DIRECTION ( 'NONE',  ( -0.5735764363510446051, 0.3127926500124816878, -0.7570804645221042017 ) ) ;
#41345 = CARTESIAN_POINT ( 'NONE',  ( 109.7185827545247889, -2.477300249445798297, -19.15521520033831138 ) ) ;
#41346 = CARTESIAN_POINT ( 'NONE',  ( 113.1912390045248031, -9.868328341294098749, -11.32035403202665869 ) ) ;
#41347 = CARTESIAN_POINT ( 'NONE',  ( 106.2459265045248173, -7.250697342233347165, -19.15521520033831138 ) ) ;
#41348 = AXIS2_PLACEMENT_3D ( 'NONE', #32043, #811, #21342 ) ;
#41349 = CARTESIAN_POINT ( 'NONE',  ( 121.8725281442453223, -3.383040157471821630, -19.15922257007629170 ) ) ;
#41350 = CARTESIAN_POINT ( 'NONE',  ( 121.8725281442453223, -6.222761293078241884, -8.102969835052219238 ) ) ;
#41351 = VERTEX_POINT ( 'NONE', #9477 ) ;
#41352 = CARTESIAN_POINT ( 'NONE',  ( 124.4252281442452812, -9.261995988541697145, -16.69588392320189030 ) ) ;
#41353 = CARTESIAN_POINT ( 'NONE',  ( 109.8574890045247940, 0.8980012041604421569, -15.77991374673208469 ) ) ;
#41354 = CARTESIAN_POINT ( 'NONE',  ( 59.92024162955036104, -14.76985142791844829, -18.18981465713234158 ) ) ;
#41355 = CARTESIAN_POINT ( 'NONE',  ( 122.4397948109119767, -9.988377603198976828, -10.36322818467138340 ) ) ;
#41356 = CARTESIAN_POINT ( 'NONE',  ( 121.5321681442453183, -9.988377603198976828, -10.36322818467138340 ) ) ;
#41357 = DIRECTION ( 'NONE',  ( -0.000000000000000000, -0.9284778069183721172, -0.3713878862591650232 ) ) ;
#41358 = CARTESIAN_POINT ( 'NONE',  ( 113.3635281442453504, -9.988377603198976828, -10.36322818467138340 ) ) ;
#41359 = CARTESIAN_POINT ( 'NONE',  ( 59.06582835810969812, -15.05120494781123597, -18.19321520033831519 ) ) ;
#41360 = CARTESIAN_POINT ( 'NONE',  ( 105.5513952545248060, 0.8980012041604421569, -11.00651665394454071 ) ) ;
#41361 = EDGE_LOOP ( 'NONE', ( #33027, #40227, #34820, #17854 ) ) ;
#41362 = LINE ( 'NONE', #10119, #4824 ) ;
#41363 = CARTESIAN_POINT ( 'NONE',  ( 114.2327140574772670, -2.443475742715324639, -17.86549347949428679 ) ) ;
#41364 = CARTESIAN_POINT ( 'NONE',  ( 124.7655881442452852, -9.859900752359378018, -12.68260735090039759 ) ) ;
#41365 = EDGE_CURVE ( 'NONE', #33919, #6291, #8800, .T. ) ;
#41366 = CARTESIAN_POINT ( 'NONE',  ( 108.7462390045248242, -9.868328341294098749, -11.32035403202665869 ) ) ;
#41367 = CARTESIAN_POINT ( 'NONE',  ( 108.5378796295247810, -4.863998795839590272, -8.388885654883775800 ) ) ;
#41368 = CARTESIAN_POINT ( 'NONE',  ( 123.2339681442453241, -3.505236298600246325, -18.68346056562440793 ) ) ;
#41369 = CARTESIAN_POINT ( 'NONE',  ( 117.8449348109119938, -1.833838273342659253, -17.42832698103878286 ) ) ;
#41370 = CARTESIAN_POINT ( 'NONE',  ( 111.5482748109120053, -0.1624402480850797581, -16.17319339645315424 ) ) ;
#41371 = ORIENTED_EDGE ( 'NONE', *, *, #10840, .F. ) ;
#41372 = AXIS2_PLACEMENT_3D ( 'NONE', #29314, #12220, #26119 ) ;
#41373 = CARTESIAN_POINT ( 'NONE',  ( 120.6463454359119822, 0.5291689781388270175, -13.89700978578772705 ) ) ;
#41374 = CARTESIAN_POINT ( 'NONE',  ( 119.3765548109119834, 0.9020085738987339008, -11.91225656197089222 ) ) ;
#41375 = FACE_OUTER_BOUND ( 'NONE', #4205, .T. ) ;
#41376 = ORIENTED_EDGE ( 'NONE', *, *, #34063, .F. ) ;
#41377 =( BOUNDED_CURVE ( )  B_SPLINE_CURVE ( 2, ( #21980, #32454, #39540, #32677, #14919, #28375, #11723, #32232, #42515, #18563, #11275, #28829, #35649, #1445, #4423, #11505, #1229 ),
 .UNSPECIFIED., .F., .T. ) 
 B_SPLINE_CURVE_WITH_KNOTS ( ( 3, 2, 2, 2, 2, 2, 2, 2, 3 ),
 ( 0.003509120678721945087, 0.01250000000000000069, 0.02500000000000000139, 0.03749999999999999861, 0.04999999999999999584, 0.06250000000000000000, 0.07499999999999999722, 0.08749999999999999445, 0.09649087932127788092 ),
 .UNSPECIFIED. ) 
 CURVE ( )  GEOMETRIC_REPRESENTATION_ITEM ( )  RATIONAL_B_SPLINE_CURVE ( ( 0.9692594319298230010, 0.9452488050343769155, 1.000000000000000000, 0.9238795325112869605, 1.000000000000000000, 0.9238795325112869605, 1.000000000000000000, 0.9238795325112869605, 1.000000000000000000, 0.9238795325112869605, 1.000000000000000000, 0.9238795325112869605, 1.000000000000000000, 0.9238795325112869605, 1.000000000000000000, 0.9452488050343769155, 0.9692594319298220018 ) ) 
 REPRESENTATION_ITEM ( '' )  );
#41378 = VERTEX_POINT ( 'NONE', #9940 ) ;
#41379 = ADVANCED_FACE ( 'NONE', ( #20649 ), #13802, .F. ) ;
#41380 = CARTESIAN_POINT ( 'NONE',  ( 114.5547881442453217, -4.153390946401321671, -8.397313243818183892 ) ) ;
#41381 = CARTESIAN_POINT ( 'NONE',  ( 112.2289948109119848, -7.643976991954077427, -18.09477374809248928 ) ) ;
#41382 = DIRECTION ( 'NONE',  ( -0.000000000000000000, -0.9284778069183718952, -0.3713878862591649677 ) ) ;
#41383 = CARTESIAN_POINT ( 'NONE',  ( 120.1601735609119856, 0.6414057260225851653, -11.69287257290600657 ) ) ;
#41384 = ORIENTED_EDGE ( 'NONE', *, *, #41766, .F. ) ;
#41385 = DIRECTION ( 'NONE',  ( -0.8636456077245080465, 0.5040994586965603652, 0.000000000000000000 ) ) ;
#41386 = FACE_OUTER_BOUND ( 'NONE', #28870, .T. ) ;
#41387 = CARTESIAN_POINT ( 'NONE',  ( 115.9693640045247776, -10.62599879583958717, -11.00651665394454604 ) ) ;
#41388 = CARTESIAN_POINT ( 'NONE',  ( 108.7294421295247844, -9.051693226400931991, -21.89321520033831447 ) ) ;
#41389 = CARTESIAN_POINT ( 'NONE',  ( 121.9859814775786333, -9.565557343593413364, -10.61323700422348004 ) ) ;
#41390 = CARTESIAN_POINT ( 'NONE',  ( 114.2711548109119803, -0.1624402480850797581, -16.17319339645315424 ) ) ;
#41391 = CARTESIAN_POINT ( 'NONE',  ( 124.8837246474731728, -7.285888985094468140, -20.69937111904969385 ) ) ;
#41392 = ORIENTED_EDGE ( 'NONE', *, *, #25873, .T. ) ;
#41393 = LINE ( 'NONE', #23605, #34589 ) ;
#41394 = CARTESIAN_POINT ( 'NONE',  ( 116.1758551332721936, 0.2334052082820642360, -14.64321520033831447 ) ) ;
#41395 = CARTESIAN_POINT ( 'NONE',  ( 113.0523327545247838, -2.477300249445798297, -19.15521520033830427 ) ) ;
#41396 = CARTESIAN_POINT ( 'NONE',  ( -2.519837040009542228, -7.040662428133670048, -19.27661969603944669 ) ) ;
#41398 = CARTESIAN_POINT ( 'NONE',  ( 121.9470836909669913, -25.99489077589524300, -13.39321520033831447 ) ) ;
#41397 = CARTESIAN_POINT ( 'NONE',  ( 66.21962885992722647, -37.11159810974177731, -4.893215200338314474 ) ) ;
#41399 = CARTESIAN_POINT ( 'NONE',  ( 112.4559014775786494, -9.988377603198976828, -10.36322818467138340 ) ) ;
#41400 = VERTEX_POINT ( 'NONE', #41847 ) ;
#41401 = CARTESIAN_POINT ( 'NONE',  ( 112.9664414775786412, 0.5811942927096154232, -14.16772938898807155 ) ) ;
#41402 = CARTESIAN_POINT ( 'NONE',  ( 107.2294421295247844, -9.051693226400931991, -21.89321520033831447 ) ) ;
#41403 = CARTESIAN_POINT ( 'NONE',  ( 115.7610046295247912, -4.863998795839590272, -7.631215200338315796 ) ) ;
#41404 = CARTESIAN_POINT ( 'NONE',  ( 125.9568481442452850, -3.505236298600246325, -18.68346056562440793 ) ) ;
#41405 = CARTESIAN_POINT ( 'NONE',  ( 123.7445081442452874, -7.894159318335828068, -9.358103419637847864 ) ) ;
#41406 = CARTESIAN_POINT ( 'NONE',  ( 86.34560043013698305, -9.320000780048239619, -18.64321520033831803 ) ) ;
#41407 = CARTESIAN_POINT ( 'NONE',  ( 108.4684265045248424, -2.791137627527939813, -8.388885654883777576 ) ) ;
#41408 = CARTESIAN_POINT ( 'NONE',  ( 112.1114130180079798, 0.7607806665037644134, -14.64321520033833046 ) ) ;
#41409 = CARTESIAN_POINT ( 'NONE',  ( 109.2294421295247844, -1.388378309844742642, -16.99368411936019641 ) ) ;
#41410 = CARTESIAN_POINT ( 'NONE',  ( 113.0231681442453180, -10.15424416112533912, -14.75197769757731336 ) ) ;
#41411 = EDGE_CURVE ( 'NONE', #4363, #27773, #25187, .T. ) ;
#41412 = CARTESIAN_POINT ( 'NONE',  ( 106.3153796295248412, -4.863998795839590272, -19.15521520033831493 ) ) ;
#41413 = AXIS2_PLACEMENT_3D ( 'NONE', #24830, #21409, #17764 ) ;
#41414 = CARTESIAN_POINT ( 'NONE',  ( 87.44708369096657918, -21.99489077589588604, -4.893215200338314474 ) ) ;
#41415 = CARTESIAN_POINT ( 'NONE',  ( 111.4549108795247747, -8.938348069036489818, -9.318865927141430916 ) ) ;
#41416 = CARTESIAN_POINT ( 'NONE',  ( 124.4819548109119722, -7.893985811506177619, -18.51759400769804742 ) ) ;
#41417 = CARTESIAN_POINT ( 'NONE',  ( 112.0588148109119828, -9.859900752359374465, -12.68260735090039404 ) ) ;
#41418 = CARTESIAN_POINT ( 'NONE',  ( 112.0630644685027875, 0.6938714319018670640, -14.64321520033829671 ) ) ;
#41419 = CARTESIAN_POINT ( 'NONE',  ( 121.3052614775786111, -1.834011780172310813, -8.268836392978581529 ) ) ;
#41420 = CARTESIAN_POINT ( 'NONE',  ( 117.1074881442453233, -10.63000616557722466, -14.87417383870573495 ) ) ;
#41421 = ORIENTED_EDGE ( 'NONE', *, *, #7045, .F. ) ;
#41422 = CARTESIAN_POINT ( 'NONE',  ( 111.7184548109119788, -0.8288870151387760510, -10.36305467784173118 ) ) ;
#41423 = CARTESIAN_POINT ( 'NONE',  ( 123.2339681442453241, -6.344957434206665248, -7.627207830600338134 ) ) ;
#41424 = CARTESIAN_POINT ( 'NONE',  ( 115.7460481442453357, 0.9020085738987339008, -11.91225656197089222 ) ) ;
#41425 = CARTESIAN_POINT ( 'NONE',  ( 116.5969481442453031, -9.859900752359374465, -12.68260735090039404 ) ) ;
#41426 = ORIENTED_EDGE ( 'NONE', *, *, #3028, .F. ) ;
#41427 = CARTESIAN_POINT ( 'NONE',  ( 117.3343948109119737, -6.222761293078241884, -8.102969835052219238 ) ) ;
#41428 = CARTESIAN_POINT ( 'NONE',  ( 115.1220548109119761, -8.166667518702817929, -8.995218007635861213 ) ) ;
#41429 = CARTESIAN_POINT ( 'NONE',  ( 122.7234281442452755, -4.153390946401325223, -8.397313243818185668 ) ) ;
#41430 = CARTESIAN_POINT ( 'NONE',  ( 116.8411265865987332, -0.9886851213817485773, -16.93018519047561554 ) ) ;
#41431 = CARTESIAN_POINT ( 'NONE',  ( 115.4831921295247952, 0.8980012041604618078, -13.39321520033831447 ) ) ;
#41432 = EDGE_LOOP ( 'NONE', ( #34842, #37599, #17929, #23451 ) ) ;
#41433 = CARTESIAN_POINT ( 'NONE',  ( 66.83296847043716582, 0.3323961765722378003, -8.951213684657119529 ) ) ;
#41434 = CARTESIAN_POINT ( 'NONE',  ( 125.5597614775786326, -1.561330072975669392, -17.79121239304076951 ) ) ;
#41435 = DIRECTION ( 'NONE',  ( -1.000000000000000000, 0.000000000000000000, -0.000000000000000000 ) ) ;
#41436 = LINE ( 'NONE', #17039, #5616 ) ;
#41437 = CARTESIAN_POINT ( 'NONE',  ( 116.8772542192391199, 1.929060082349297822, -5.778250657087603770 ) ) ;
#41438 = CARTESIAN_POINT ( 'NONE',  ( 124.6040088552590959, -9.657516929632931735, -14.85109078001513083 ) ) ;
#41439 = CARTESIAN_POINT ( 'NONE',  ( 106.8710046295248759, -4.863998795839590272, -18.39754474579285315 ) ) ;
#41440 = CARTESIAN_POINT ( 'NONE',  ( 69.29215060918571112, -66.20770173783323287, -36.32231744093705572 ) ) ;
#41441 = CARTESIAN_POINT ( 'NONE',  ( 117.3343948109119737, -3.383040157471821630, -19.15922257007629170 ) ) ;
#41442 = CARTESIAN_POINT ( 'NONE',  ( 123.0772048109119652, -2.527210466738039063, -8.967976844669125924 ) ) ;
#41443 = CARTESIAN_POINT ( 'NONE',  ( 115.5695697905468933, 0.6938714319018670640, -12.14321520033833579 ) ) ;
#41444 = CARTESIAN_POINT ( 'NONE',  ( 96.46827370896536991, -26.80223900086530264, -12.78781649172082879 ) ) ;
#41445 = CARTESIAN_POINT ( 'NONE',  ( 122.6667014775786413, -2.084020599724406786, -8.691656652584148546 ) ) ;
#41446 = ORIENTED_EDGE ( 'NONE', *, *, #3382, .F. ) ;
#41447 = CARTESIAN_POINT ( 'NONE',  ( 122.3011713555256534, -8.364211927971188842, -17.30190421972978143 ) ) ;
#41448 = CARTESIAN_POINT ( 'NONE',  ( 117.9016614775786280, -9.988377603198976828, -10.36322818467138340 ) ) ;
#41449 = CARTESIAN_POINT ( 'NONE',  ( 126.2404814775786264, -9.261995988541697145, -16.69588392320189030 ) ) ;
#41450 = CARTESIAN_POINT ( 'NONE',  ( 114.0442481442453300, -7.643976991954077427, -18.09477374809248928 ) ) ;
#41451 = CARTESIAN_POINT ( 'NONE',  ( 112.5693548109119888, 0.4262465694468514643, -12.03445270309931736 ) ) ;
#41452 = CARTESIAN_POINT ( 'NONE',  ( 112.2883483795247770, -0.7896495226426338832, -9.318865927141430916 ) ) ;
#41453 = B_SPLINE_CURVE_WITH_KNOTS ( 'NONE', 3,
 ( #4903, #18819, #14954, #32710, #39795, #8564, #5129, #19046, #28866, #21569, #32933, #1708, #35456, #32044, #11540, #40019 ),
 .UNSPECIFIED., .F., .F.,
 ( 4, 2, 2, 2, 2, 2, 2, 4 ),
 ( 6.992893892674702526E-18, 0.001905203037969943657, 0.002857804556954912124, 0.003810406075939880375, 0.004763007594924848626, 0.005715609113909817310, 0.006668210632894785127, 0.007620812151879753811 ),
 .UNSPECIFIED. ) ;
#41454 = DIRECTION ( 'NONE',  ( 0.000000000000000000, 0.9242245927363028635, 0.3818493186865930533 ) ) ;
#41455 = CARTESIAN_POINT ( 'NONE',  ( 116.6536748109119941, -10.15424416112533912, -14.75197769757731336 ) ) ;
#41456 = CARTESIAN_POINT ( 'NONE',  ( 121.0216281442452981, -7.894159318335828068, -9.358103419637847864 ) ) ;
#41457 = CARTESIAN_POINT ( 'NONE',  ( 70.89841814381148311, -68.89136543047671069, -37.69090763720760151 ) ) ;
#41458 = CARTESIAN_POINT ( 'NONE',  ( 120.2990798109119766, -2.173413727453600508, -8.297982527556802879 ) ) ;
#41459 = CARTESIAN_POINT ( 'NONE',  ( 107.8433483795247838, -8.402594152722688392, -16.93181055722141792 ) ) ;
#41460 = CARTESIAN_POINT ( 'NONE',  ( 109.2294424423713650, -0.4563628856859095473, -15.90327673384510376 ) ) ;
#41461 = CARTESIAN_POINT ( 'NONE',  ( 114.0442481442453300, -1.834011780172310813, -8.268836392978581529 ) ) ;
#41462 = CARTESIAN_POINT ( 'NONE',  ( 116.5969481442453031, 0.5811942927096154232, -14.16772938898807155 ) ) ;
#41463 = CARTESIAN_POINT ( 'NONE',  ( 122.7299391859119737, -1.406689858478933353, -17.56299727309130887 ) ) ;
#41464 = CARTESIAN_POINT ( 'NONE',  ( 121.4797829359119987, -5.367793381288652910, -18.78638297431638904 ) ) ;
#41465 = ORIENTED_EDGE ( 'NONE', *, *, #27287, .F. ) ;
#41466 = CARTESIAN_POINT ( 'NONE',  ( 123.4588159614330749, -2.807939993087918751, -14.88215444561602219 ) ) ;
#41467 = EDGE_CURVE ( 'NONE', #39048, #26194, #28159, .T. ) ;
#41468 = ORIENTED_EDGE ( 'NONE', *, *, #27538, .T. ) ;
#41469 = CARTESIAN_POINT ( 'NONE',  ( 121.9292548109119849, -1.561330072975668948, -17.79121239304076951 ) ) ;
#41470 = CARTESIAN_POINT ( 'NONE',  ( 114.3278814775786429, -10.30919188438810075, -12.61870101168855918 ) ) ;
#41471 = CARTESIAN_POINT ( 'NONE',  ( 119.7169148109119874, -0.1624402480850797581, -16.17319339645315424 ) ) ;
#41472 =( NAMED_UNIT ( * ) PLANE_ANGLE_UNIT ( ) SI_UNIT ( $, .RADIAN. ) );
#41473 = FACE_OUTER_BOUND ( 'NONE', #7184, .T. ) ;
#41474 = AXIS2_PLACEMENT_3D ( 'NONE', #18554, #1880, #32885 ) ;
#41475 = CARTESIAN_POINT ( 'NONE',  ( 123.0637881442452937, -0.4660016031367893996, -10.09054647747474043 ) ) ;
#41476 = CARTESIAN_POINT ( 'NONE',  ( 117.2776681442452968, -5.638512984488999180, -18.83840828888717311 ) ) ;
#41477 = EDGE_CURVE ( 'NONE', #37342, #37016, #23399, .T. ) ;
#41478 = CARTESIAN_POINT ( 'NONE',  ( 115.9693640045247776, -10.62599879583958717, -11.00651665394454604 ) ) ;
#41479 = CARTESIAN_POINT ( 'NONE',  ( 112.0588148109119828, -9.859900752359374465, -12.68260735090039404 ) ) ;
#41480 = DIRECTION ( 'NONE',  ( 0.000000000000000000, 0.000000000000000000, -1.000000000000000000 ) ) ;
#41481 = ORIENTED_EDGE ( 'NONE', *, *, #5828, .F. ) ;
#41482 = CARTESIAN_POINT ( 'NONE',  ( 116.6536748109119941, 0.9020085738987339008, -11.91225656197089222 ) ) ;
#41483 = CARTESIAN_POINT ( 'NONE',  ( 119.8823610609119754, -3.163656168406935087, -18.89861972220014508 ) ) ;
#41484 = CARTESIAN_POINT ( 'NONE',  ( 116.9373081442452929, -8.166667518702817929, -8.995218007635861213 ) ) ;
#41485 = ORIENTED_EDGE ( 'NONE', *, *, #45112, .F. ) ;
#41486 = CARTESIAN_POINT ( 'NONE',  ( 114.5803015045248117, -2.477300249445798297, -7.631215200338321125 ) ) ;
#41487 = CARTESIAN_POINT ( 'NONE',  ( 124.9924948109119924, -4.089484607189486809, -7.948022111789456723 ) ) ;
#41488 = DIRECTION ( 'NONE',  ( 0.000000000000000000, 0.3818493186865927203, -0.9242245927363029745 ) ) ;
#41489 = DIRECTION ( 'NONE',  ( 0.4649787261689616868, 0.8853218534579894161, 0.000000000000000000 ) ) ;
#41490 = EDGE_CURVE ( 'NONE', #36673, #44158, #18127, .T. ) ;
#41491 = CARTESIAN_POINT ( 'NONE',  ( 78.69189222814995333, -59.47240852290178026, 0.2605592176021376827 ) ) ;
#41492 = CARTESIAN_POINT ( 'NONE',  ( 115.7460481442453357, -10.15424416112533912, -14.75197769757731336 ) ) ;
#41493 = EDGE_CURVE ( 'NONE', #33632, #25485, #24465, .T. ) ;
#41494 = EDGE_CURVE ( 'NONE', #166, #5970, #36101, .T. ) ;
#41495 = DIRECTION ( 'NONE',  ( -0.000000000000000000, -0.9284778069183721172, -0.3713878862591650232 ) ) ;
#41496 = CARTESIAN_POINT ( 'NONE',  ( 116.8238548109119819, -5.574606645277164318, -18.38911715685844683 ) ) ;
#41497 = VECTOR ( 'NONE', #11204, 1000.000000000000000 ) ;
#41498 = CARTESIAN_POINT ( 'NONE',  ( 72.69189222814998175, -41.76310523276723785, -24.89321520033831447 ) ) ;
#41499 = CARTESIAN_POINT ( 'NONE',  ( 115.6325948109119821, -9.565557343593413364, -10.61323700422348004 ) ) ;
#41500 = FACE_OUTER_BOUND ( 'NONE', #13037, .T. ) ;
#41501 = CARTESIAN_POINT ( 'NONE',  ( 114.0442481442453300, -1.834011780172310813, -8.268836392978581529 ) ) ;
#41502 = CARTESIAN_POINT ( 'NONE',  ( 126.1270281442452870, -10.30919188438810075, -12.61870101168855918 ) ) ;
#41503 = B_SPLINE_CURVE_WITH_KNOTS ( 'NONE', 3,
 ( #23610, #36587, #15860, #5362 ),
 .UNSPECIFIED., .F., .F.,
 ( 4, 4 ),
 ( 0.000000000000000000, 1.000000000000000000 ),
 .UNSPECIFIED. ) ;
#41504 = CARTESIAN_POINT ( 'NONE',  ( 116.0864081442453113, -0.1624402480850797581, -16.17319339645315424 ) ) ;
#41505 = ORIENTED_EDGE ( 'NONE', *, *, #15842, .T. ) ;
#41506 = CARTESIAN_POINT ( 'NONE',  ( 115.2922348109119781, -10.63000616557722466, -14.87417383870573495 ) ) ;
#41507 = CARTESIAN_POINT ( 'NONE',  ( 109.0935046295247872, -4.863998795839590272, -7.631215200338315796 ) ) ;
#41508 = CARTESIAN_POINT ( 'NONE',  ( 107.2877233795247776, -1.325403438956436419, -9.854619843455211026 ) ) ;
#41509 = CARTESIAN_POINT ( 'NONE',  ( 110.2184548109119788, -1.904930392188239452, -16.08466725871020842 ) ) ;
#41510 = CARTESIAN_POINT ( 'NONE',  ( 127.9673516049440138, -4.191936442424658793, -15.53703219575882954 ) ) ;
#41511 = CARTESIAN_POINT ( 'NONE',  ( 121.3619881442452879, -4.089484607189486809, -7.948022111789456723 ) ) ;
#41512 = ORIENTED_EDGE ( 'NONE', *, *, #39891, .T. ) ;
#41513 = VECTOR ( 'NONE', #13284, 1000.000000000000000 ) ;
#41514 = DIRECTION ( 'NONE',  ( 0.9609149988134843001, -0.1028163501681632064, 0.2570431154366505933 ) ) ;
#41515 = CARTESIAN_POINT ( 'NONE',  ( 116.3700414775786527, -4.153390946401321671, -8.397313243818183892 ) ) ;
#41516 = CARTESIAN_POINT ( 'NONE',  ( 123.7717360609119623, -6.564341423271550902, -7.887810678476487425 ) ) ;
#41517 = CARTESIAN_POINT ( 'NONE',  ( 123.0637881442452937, -0.4660016031367893996, -10.09054647747474043 ) ) ;
#41518 = CARTESIAN_POINT ( 'NONE',  ( 115.4137390045248566, -9.868328341294098749, -11.32035403202665869 ) ) ;
#41519 = CARTESIAN_POINT ( 'NONE',  ( 124.6713397424434078, -0.9924539043446091169, -17.29976612834908423 ) ) ;
#41520 = ORIENTED_EDGE ( 'NONE', *, *, #35777, .F. ) ;
#41521 = CARTESIAN_POINT ( 'NONE',  ( 112.7395348109119766, -5.638512984488999180, -18.83840828888717311 ) ) ;
#41522 = CARTESIAN_POINT ( 'NONE',  ( 112.1722681442453222, -0.4660016031367893996, -10.09054647747474043 ) ) ;
#41523 = CARTESIAN_POINT ( 'NONE',  ( 123.0070614775786169, 0.9020085738987339008, -11.91225656197089222 ) ) ;
#41524 = CARTESIAN_POINT ( 'NONE',  ( 117.1074881442453233, 0.4262465694468514643, -12.03445270309931736 ) ) ;
#41525 = DIRECTION ( 'NONE',  ( 0.000000000000000000, -0.3818493186865927203, 0.9242245927363029745 ) ) ;
#41526 = CARTESIAN_POINT ( 'NONE',  ( 118.8092881442453290, -9.988377603198976828, -10.36322818467138340 ) ) ;
#41527 = DIRECTION ( 'NONE',  ( 0.000000000000000000, 0.3818493186865928868, -0.9242245927363027524 ) ) ;
#41528 = CARTESIAN_POINT ( 'NONE',  ( 123.4608748109119745, 0.4262465694468514643, -12.03445270309931736 ) ) ;
#41529 = ORIENTED_EDGE ( 'NONE', *, *, #32432, .F. ) ;
#41530 = DIRECTION ( 'NONE',  ( 1.000000000000000000, 0.000000000000000000, 0.000000000000000000 ) ) ;
#41531 = AXIS2_PLACEMENT_3D ( 'NONE', #15700, #11831, #14798 ) ;
#41532 = CARTESIAN_POINT ( 'NONE',  ( 115.4056881442453459, -7.893985811506177619, -18.51759400769804742 ) ) ;
#41533 = CARTESIAN_POINT ( 'NONE',  ( 124.0848681442452772, -5.574606645277164318, -18.38911715685844683 ) ) ;
#41534 = ORIENTED_EDGE ( 'NONE', *, *, #41286, .F. ) ;
#41535 = CARTESIAN_POINT ( 'NONE',  ( 120.5768923109119868, -9.959231468620755479, -10.70263013195267199 ) ) ;
#41536 = CARTESIAN_POINT ( 'NONE',  ( 137.0105207745634743, -1.266623274720264369, -9.287743120492423898 ) ) ;
#41537 = CARTESIAN_POINT ( 'NONE',  ( 121.0783548109119749, 0.2603800115204892296, -16.42320221600525088 ) ) ;
#41538 = CARTESIAN_POINT ( 'NONE',  ( 106.8710046295248759, -4.863998795839590272, -7.631215200338315796 ) ) ;
#41539 = CARTESIAN_POINT ( 'NONE',  ( 120.6245414775786458, -0.1624402480850797581, -16.17319339645315424 ) ) ;
#41540 = ORIENTED_EDGE ( 'NONE', *, *, #6611, .T. ) ;
#41541 = ORIENTED_EDGE ( 'NONE', *, *, #10088, .T. ) ;
#41542 = CIRCLE ( 'NONE', #2190, 3.000000000000003997 ) ;
#41543 = CARTESIAN_POINT ( 'NONE',  ( 114.8951481442453115, -0.4660016031367893996, -10.09054647747474043 ) ) ;
#41544 = LINE ( 'NONE', #37657, #4446 ) ;
#41545 = AXIS2_PLACEMENT_3D ( 'NONE', #32, #21004, #34879 ) ;
#41546 = DIRECTION ( 'NONE',  ( 1.000000000000000000, 0.000000000000000000, 0.000000000000000000 ) ) ;
#41547 = EDGE_CURVE ( 'NONE', #22388, #15377, #41946, .T. ) ;
#41548 = DIRECTION ( 'NONE',  ( 0.000000000000000000, -0.6998542122237657592, -0.7142857142857138575 ) ) ;
#41549 = CARTESIAN_POINT ( 'NONE',  ( 123.3474214775786209, -9.988377603198976828, -10.36322818467138340 ) ) ;
#41550 = CARTESIAN_POINT ( 'NONE',  ( 111.6428307106015438, -9.187052517560628573, -16.66868250367536319 ) ) ;
#41551 = FACE_OUTER_BOUND ( 'NONE', #23878, .T. ) ;
#41552 = CARTESIAN_POINT ( 'NONE',  ( 119.9438214775786378, -7.893985811506177619, -18.51759400769804742 ) ) ;
#41554 = CARTESIAN_POINT ( 'NONE',  ( 120.6812681442452941, 0.1319031606808879209, -14.10382304977623669 ) ) ;
#41553 = CARTESIAN_POINT ( 'NONE',  ( 118.4689281442453392, 0.9020085738987339008, -11.91225656197089222 ) ) ;
#41555 = ADVANCED_FACE ( 'NONE', ( #24510 ), #26675, .T. ) ;
#41556 = CARTESIAN_POINT ( 'NONE',  ( 125.4924948109119924, -4.159894987976798575, -8.443039665293765594 ) ) ;
#41557 = CARTESIAN_POINT ( 'NONE',  ( 116.0296814775786345, -8.166667518702817929, -8.995218007635861213 ) ) ;
#41558 = ORIENTED_EDGE ( 'NONE', *, *, #20384, .T. ) ;
#41559 = CARTESIAN_POINT ( 'NONE',  ( 112.5693548109119888, -10.63000616557722466, -14.87417383870573495 ) ) ;
#41560 = DIRECTION ( 'NONE',  ( -0.2768435750659263839, -0.3568721902840679139, 0.8921882507333128709 ) ) ;
#41561 = CARTESIAN_POINT ( 'NONE',  ( 108.8156921295247912, 0.8980012041604618078, -13.39321520033831447 ) ) ;
#41562 = CARTESIAN_POINT ( 'NONE',  ( 108.3295202545248657, 0.1403307496149616695, -11.32035403202665336 ) ) ;
#41563 = CARTESIAN_POINT ( 'NONE',  ( 108.2600671295247992, -10.62599879583958540, -13.39321520033831447 ) ) ;
#41564 = AXIS2_PLACEMENT_3D ( 'NONE', #29827, #36875, #19566 ) ;
#41565 = CARTESIAN_POINT ( 'NONE',  ( 125.2761281442453054, -10.63000616557722466, -14.87417383870573495 ) ) ;
#41566 = CARTESIAN_POINT ( 'NONE',  ( 111.7751814775786556, -7.893985811506177619, -18.51759400769804742 ) ) ;
#41567 = ORIENTED_EDGE ( 'NONE', *, *, #40719, .F. ) ;
#41568 = CARTESIAN_POINT ( 'NONE',  ( 126.1837548109119211, -10.63000616557722466, -14.87417383870573495 ) ) ;
#41569 = CARTESIAN_POINT ( 'NONE',  ( 109.5796765045248122, -7.250697342233347165, -19.15521520033831138 ) ) ;
#41570 = CARTESIAN_POINT ( 'NONE',  ( 123.0070614775786169, 0.9020085738987339008, -11.91225656197089222 ) ) ;
#41571 = CARTESIAN_POINT ( 'NONE',  ( 123.9146881442452894, 0.9020085738987339008, -11.91225656197089222 ) ) ;
#41572 = CARTESIAN_POINT ( 'NONE',  ( 119.3961891859119930, -1.406689858478933353, -17.56299727309130887 ) ) ;
#41573 = CARTESIAN_POINT ( 'NONE',  ( 112.1155414775786454, 0.9020085738987339008, -11.91225656197089222 ) ) ;
#41574 = CARTESIAN_POINT ( 'NONE',  ( 122.7299391859119737, -1.406689858478933353, -17.56299727309130887 ) ) ;
#41575 = CARTESIAN_POINT ( 'NONE',  ( 107.1488171295247867, -10.62599879583958540, -13.39321520033831447 ) ) ;
#41576 = EDGE_LOOP ( 'NONE', ( #628, #10519, #37391, #13462, #34327 ) ) ;
#41577 = DIRECTION ( 'NONE',  ( -0.000000000000000000, -0.9284778069183721172, -0.3713878862591650232 ) ) ;
#41578 = VECTOR ( 'NONE', #36552, 1000.000000000000000 ) ;
#41579 = CARTESIAN_POINT ( 'NONE',  ( 113.8740681442453138, -9.859900752359374465, -12.68260735090039404 ) ) ;
#41580 = CARTESIAN_POINT ( 'NONE',  ( 113.5337081442453240, -9.261995988541697145, -16.69588392320189030 ) ) ;
#41581 = CARTESIAN_POINT ( 'NONE',  ( 115.6915515045247531, -2.477300249445798297, -7.631215200338321125 ) ) ;
#41582 = CARTESIAN_POINT ( 'NONE',  ( 106.9404577545248145, -2.791137627527939813, -18.39754474579286025 ) ) ;
#41583 = VECTOR ( 'NONE', #5591, 1000.000000000000227 ) ;
#41584 = CARTESIAN_POINT ( 'NONE',  ( 120.3976348109119812, -7.643976991954077427, -18.09477374809248928 ) ) ;
#41585 = UNCERTAINTY_MEASURE_WITH_UNIT (LENGTH_MEASURE( 1.000000000000000082E-05 ), #23464, 'distance_accuracy_value', 'NONE');
#41586 = CARTESIAN_POINT ( 'NONE',  ( 116.3133148109120043, -2.084020599724406786, -8.691656652584148546 ) ) ;
#41587 = CARTESIAN_POINT ( 'NONE',  ( 113.2500748109119968, -3.505236298600246325, -18.68346056562440793 ) ) ;
#41588 = ORIENTED_EDGE ( 'NONE', *, *, #15156, .F. ) ;
#41589 = CARTESIAN_POINT ( 'NONE',  ( 121.6881423109119709, -0.4387604401700512802, -15.73000352943951619 ) ) ;
#41590 = CARTESIAN_POINT ( 'NONE',  ( 119.8870948109119752, -9.261995988541697145, -16.69588392320189030 ) ) ;
#41591 = DIRECTION ( 'NONE',  ( -0.2407039305251456596, 0.3604685577742790525, -0.9011792478113757054 ) ) ;
#41592 = CARTESIAN_POINT ( 'NONE',  ( 113.3068014775786594, -1.833838273342658809, -17.42832698103878286 ) ) ;
#41593 = ORIENTED_EDGE ( 'NONE', *, *, #31983, .F. ) ;
#41594 = CARTESIAN_POINT ( 'NONE',  ( 70.19189222814998175, -58.18802696105826300, -36.47801710466001879 ) ) ;
#41595 = EDGE_CURVE ( 'NONE', #35460, #38024, #19588, .T. ) ;
#41596 = ORIENTED_EDGE ( 'NONE', *, *, #29187, .F. ) ;
#41597 = CARTESIAN_POINT ( 'NONE',  ( 119.7169148109119874, -0.1624402480850797581, -16.17319339645315424 ) ) ;
#41598 = CARTESIAN_POINT ( 'NONE',  ( 112.5126281442453120, 0.1319031606808879209, -14.10382304977623669 ) ) ;
#41599 = FACE_OUTER_BOUND ( 'NONE', #12142, .T. ) ;
#41600 = CARTESIAN_POINT ( 'NONE',  ( 120.5768923109119868, -9.959231468620755479, -10.70263013195267199 ) ) ;
#41601 = ORIENTED_EDGE ( 'NONE', *, *, #43691, .F. ) ;
#41602 = CARTESIAN_POINT ( 'NONE',  ( 59.77099224207091055, -14.81899841792058226, -8.593215200338313764 ) ) ;
#41603 = CARTESIAN_POINT ( 'NONE',  ( 125.1028739313161964, 2.504666235963327381, -12.16890819705307614 ) ) ;
#41604 = CARTESIAN_POINT ( 'NONE',  ( 114.2330358795247776, -0.7896495226426338832, -17.46756447353520159 ) ) ;
#41605 = AXIS2_PLACEMENT_3D ( 'NONE', #43869, #26766, #10726 ) ;
#41606 = EDGE_CURVE ( 'NONE', #43185, #35115, #1003, .T. ) ;
#41607 = EDGE_CURVE ( 'NONE', #9213, #44499, #769, .T. ) ;
#41608 = CYLINDRICAL_SURFACE ( 'NONE', #43796, 5.000000000000002665 ) ;
#41609 = VECTOR ( 'NONE', #43095, 1000.000000000000000 ) ;
#41610 = CARTESIAN_POINT ( 'NONE',  ( 122.7801548109119665, -6.222761293078241884, -8.102969835052219238 ) ) ;
#41611 = CARTESIAN_POINT ( 'NONE',  ( 118.5823814775786360, -7.643976991954077427, -18.09477374809248928 ) ) ;
#41612 = CYLINDRICAL_SURFACE ( 'NONE', #18480, 1.999999999999998890 ) ;
#41613 = ORIENTED_EDGE ( 'NONE', *, *, #21674, .T. ) ;
#41614 = CARTESIAN_POINT ( 'NONE',  ( 127.5515732256049262, -2.090882025624695384, -18.33502473074995720 ) ) ;
#41615 = CARTESIAN_POINT ( 'NONE',  ( 115.4624148109119943, -4.153390946401321671, -8.397313243818183892 ) ) ;
#41616 = CARTESIAN_POINT ( 'NONE',  ( 84.39081516114413262, -30.32262605124143562, -12.39321520033831447 ) ) ;
#41617 = DIRECTION ( 'NONE',  ( 0.000000000000000000, -0.3818493186865936084, 0.9242245927363024194 ) ) ;
#41618 = CARTESIAN_POINT ( 'NONE',  ( 124.8790414775786246, -8.899110576539710493, -16.42337572283490132 ) ) ;
#41619 = ORIENTED_EDGE ( 'NONE', *, *, #10549, .F. ) ;
#41620 = CARTESIAN_POINT ( 'NONE',  ( 114.7816948109119863, 0.5811942927096154232, -14.16772938898807155 ) ) ;
#41621 = CARTESIAN_POINT ( 'NONE',  ( 126.8396850857678970, 0.1815689017518152260, -15.05047689119776422 ) ) ;
#41622 = CARTESIAN_POINT ( 'NONE',  ( 106.7320983795247855, -8.402594152722688392, -16.93181055722141792 ) ) ;
#41623 = CARTESIAN_POINT ( 'NONE',  ( 113.5904348109119866, -7.893985811506177619, -18.51759400769804742 ) ) ;
#41624 = CARTESIAN_POINT ( 'NONE',  ( 115.6325948109119821, 0.2603800115204892296, -16.42320221600525088 ) ) ;
#41625 = CARTESIAN_POINT ( 'NONE',  ( 123.8579614775786126, -9.859900752359378018, -12.68260735090039759 ) ) ;
#41626 = FACE_OUTER_BOUND ( 'NONE', #36063, .T. ) ;
#41627 = CARTESIAN_POINT ( 'NONE',  ( 110.1353015045248469, -6.936859964151250502, -18.39754474579286025 ) ) ;
#41628 = CARTESIAN_POINT ( 'NONE',  ( 111.1282721536728104, 0.3967854368540359999, -10.50530088663808925 ) ) ;
#41629 = DIRECTION ( 'NONE',  ( 0.9489384314806882381, 0.3124801273375108490, -0.04326688431241968585 ) ) ;
#41630 = AXIS2_PLACEMENT_3D ( 'NONE', #43211, #33368, #25880 ) ;
#41631 = CARTESIAN_POINT ( 'NONE',  ( 117.6180281442453150, -8.899110576539710493, -16.42337572283490132 ) ) ;
#41632 = CARTESIAN_POINT ( 'NONE',  ( 107.9822546295247889, -4.863998795839590272, -7.631215200338315796 ) ) ;
#41633 = DIRECTION ( 'NONE',  ( 1.000000000000000000, 0.000000000000000000, -0.000000000000000000 ) ) ;
#41634 = CARTESIAN_POINT ( 'NONE',  ( 109.2324108795247923, -8.938348069036489818, -9.318865927141430916 ) ) ;
#41635 = CARTESIAN_POINT ( 'NONE',  ( 126.1270281442452870, -10.30919188438810075, -12.61870101168855918 ) ) ;
#41636 = CARTESIAN_POINT ( 'NONE',  ( 125.9568481442452850, -6.344957434206665248, -7.627207830600338134 ) ) ;
#41637 = CARTESIAN_POINT ( 'NONE',  ( 120.0005481442453146, -4.153390946401307460, -8.397313243818183892 ) ) ;
#41638 =( BOUNDED_CURVE ( )  B_SPLINE_CURVE ( 2, ( #15710, #40103, #26196, #8863, #22765, #33010, #1785, #43528, #12957, #19105, #36420, #33899, #41004, #2445, #1996, #43511, #9758 ),
 .UNSPECIFIED., .F., .T. ) 
 B_SPLINE_CURVE_WITH_KNOTS ( ( 3, 2, 2, 2, 2, 2, 2, 2, 3 ),
 ( 0.07950466748089210500, 0.08593750000000000000, 0.09375000000000000000, 0.1015625000000000000, 0.1093750000000000000, 0.1171875000000000000, 0.1250000000000000000, 0.1328125000000000000, 0.1392453325190584068 ),
 .UNSPECIFIED. ) 
 CURVE ( )  GEOMETRIC_REPRESENTATION_ITEM ( )  RATIONAL_B_SPLINE_CURVE ( ( 0.9778625265006459788, 0.9373222120152200354, 1.000000000000000000, 0.9238795325112869605, 1.000000000000000000, 0.9238795325112869605, 1.000000000000000000, 0.9238795325112869605, 1.000000000000000000, 0.9238795325112869605, 1.000000000000000000, 0.9238795325112869605, 1.000000000000000000, 0.9238795325112869605, 1.000000000000000000, 0.9373222120157019832, 0.9778625265000240319 ) ) 
 REPRESENTATION_ITEM ( '' )  );
#41639 = CARTESIAN_POINT ( 'NONE',  ( 119.8303681442453126, -10.63000616557722466, -14.87417383870573495 ) ) ;
#41640 = CARTESIAN_POINT ( 'NONE',  ( 117.7882081442453170, -6.344957434206665248, -7.627207830600338134 ) ) ;
#41641 = ORIENTED_EDGE ( 'NONE', *, *, #21172, .T. ) ;
#41642 = CARTESIAN_POINT ( 'NONE',  ( 114.8384214775786489, -10.15424416112533912, -14.75197769757731336 ) ) ;
#41643 = AXIS2_PLACEMENT_3D ( 'NONE', #43571, #35810, #12340 ) ;
#41644 = CARTESIAN_POINT ( 'NONE',  ( 124.3117748109119844, -10.30919188438810075, -12.61870101168855918 ) ) ;
#41645 = CARTESIAN_POINT ( 'NONE',  ( 112.9097148109120070, 0.2603800115204892296, -16.42320221600525088 ) ) ;
#41646 = CARTESIAN_POINT ( 'NONE',  ( 116.5402214775786405, -9.565557343593413364, -10.61323700422348004 ) ) ;
#41647 = ORIENTED_EDGE ( 'NONE', *, *, #28963, .F. ) ;
#41648 = CARTESIAN_POINT ( 'NONE',  ( 120.7379948109119709, 0.4262465694468514643, -12.03445270309931736 ) ) ;
#41649 = CARTESIAN_POINT ( 'NONE',  ( 117.9583881442453048, -10.30919188438810075, -12.61870101168855918 ) ) ;
#41650 = CARTESIAN_POINT ( 'NONE',  ( 116.8404992881385311, -1.011272923461008499, -16.95395943642953540 ) ) ;
#41651 = CARTESIAN_POINT ( 'NONE',  ( 115.8304577545247582, -7.250697342233347165, -7.631215200338321125 ) ) ;
#41652 = ORIENTED_EDGE ( 'NONE', *, *, #25481, .T. ) ;
#41653 = CARTESIAN_POINT ( 'NONE',  ( 62.78991778472225604, -1.552662796812879664, -7.442402790401765778 ) ) ;
#41654 = DIRECTION ( 'NONE',  ( 0.000000000000000000, 0.000000000000000000, 1.000000000000000000 ) ) ;
#41655 = DIRECTION ( 'NONE',  ( -0.3135808629537518155, -0.9495615000563051300, -0.000000000000000000 ) ) ;
#41656 = AXIS2_PLACEMENT_3D ( 'NONE', #39207, #4545, #28956 ) ;
#41657 = CARTESIAN_POINT ( 'NONE',  ( 114.6115148109119986, -3.383040157471821630, -19.15922257007629170 ) ) ;
#41658 = EDGE_CURVE ( 'NONE', #8943, #20803, #39037, .T. ) ;
#41659 = CARTESIAN_POINT ( 'NONE',  ( 89.78938736644981589, -25.23119213852205789, -15.24166438581092109 ) ) ;
#41660 = CARTESIAN_POINT ( 'NONE',  ( 112.3424481442453384, -3.505236298600246325, -18.68346056562440793 ) ) ;
#41661 = B_SPLINE_CURVE_WITH_KNOTS ( 'NONE', 3,
 ( #21526, #28601, #11501, #999, #39304, #32001, #21976, #32450, #28370, #22198, #32227, #38843, #36094, #17883, #7847, #42735, #42283, #35864, #4637, #11045, #1441, #39752, #8521, #11719, #18558, #32673, #1224, #25179, #15138, #18108 ),
 .UNSPECIFIED., .F., .F.,
 ( 4, 2, 2, 1, 1, 1, 2, 2, 2, 1, 1, 1, 2, 2, 1, 1, 2, 2, 4 ),
 ( 0.000000000000000000, 0.2499999999999658606, 0.3749999999999484857, 0.4374999999999535372, 0.4687499999999424349, 0.4843749999999234501, 0.4921874999999282796, 0.4999999999999330536, 0.6249999999999854561, 0.6875000000000218714, 0.7187500000000519584, 0.7343750000000555112, 0.7421875000000458522, 0.7500000000000361933, 0.8125000000000430767, 0.8437500000000454081, 0.8593750000000381917, 0.8750000000000309752, 1.000000000000000000 ),
 .UNSPECIFIED. ) ;
#41662 = CARTESIAN_POINT ( 'NONE',  ( 70.19189222814998175, -50.76020450571126474, -33.50691401458669105 ) ) ;
#41663 = LINE ( 'NONE', #24327, #2534 ) ;
#41664 = CARTESIAN_POINT ( 'NONE',  ( 114.5803015045248117, -6.936859964151250502, -18.39754474579286025 ) ) ;
#41665 = CARTESIAN_POINT ( 'NONE',  ( 119.7169148109119874, -9.988377603198976828, -10.36322818467138340 ) ) ;
#41666 = VECTOR ( 'NONE', #422, 1000.000000000000000 ) ;
#41667 = CARTESIAN_POINT ( 'NONE',  ( 115.6179021944298881, 0.6269505268395592079, -12.14321520033831625 ) ) ;
#41668 = CARTESIAN_POINT ( 'NONE',  ( 124.6746266859119743, -9.033780868592048208, -16.85052413769886215 ) ) ;
#41669 = CARTESIAN_POINT ( 'NONE',  ( 120.7947214775786193, -0.8288870151387760510, -10.36305467784173118 ) ) ;
#41670 = ORIENTED_EDGE ( 'NONE', *, *, #45135, .T. ) ;
#41671 = CARTESIAN_POINT ( 'NONE',  ( 125.7866681442452688, -0.4660016031367893996, -10.09054647747474043 ) ) ;
#41672 = CARTESIAN_POINT ( 'NONE',  ( 118.1285681442453068, -7.893985811506177619, -18.51759400769804742 ) ) ;
#41673 = DIRECTION ( 'NONE',  ( -0.2768435750659253847, -0.3568721902840677473, 0.8921882507333133150 ) ) ;
#41674 = CARTESIAN_POINT ( 'NONE',  ( 115.1787814775786387, -0.1624402480850797581, -16.17319339645315424 ) ) ;
#41675 = CARTESIAN_POINT ( 'NONE',  ( 113.9875214775786532, -8.899110576539710493, -16.42337572283490132 ) ) ;
#41676 = CARTESIAN_POINT ( 'NONE',  ( 105.2041296295248287, -4.863998795839590272, -8.388885654883775800 ) ) ;
#41677 = CARTESIAN_POINT ( 'NONE',  ( 111.1076452545248259, 0.8980012041604421569, -11.00651665394454071 ) ) ;
#41678 = CARTESIAN_POINT ( 'NONE',  ( 118.5256548109119876, -8.899110576539710493, -16.42337572283490132 ) ) ;
#41679 = CARTESIAN_POINT ( 'NONE',  ( 121.9292548109119849, -7.894159318335828068, -9.358103419637847864 ) ) ;
#41680 = CARTESIAN_POINT ( 'NONE',  ( 121.4103298109119748, -2.173413727453600508, -8.297982527556802879 ) ) ;
#41681 = CARTESIAN_POINT ( 'NONE',  ( 107.4960827545248350, -6.936859964151250502, -8.388885654883777576 ) ) ;
#41682 = CARTESIAN_POINT ( 'NONE',  ( 61.69189222814998175, -69.76310523276724496, -16.89321520033831447 ) ) ;
#41683 = CARTESIAN_POINT ( 'NONE',  ( 112.6260814775786514, -9.261995988541697145, -16.69588392320189030 ) ) ;
#41684 = CARTESIAN_POINT ( 'NONE',  ( 115.5191414775786569, -3.383040157471821630, -19.15922257007629170 ) ) ;
#41685 = DIRECTION ( 'NONE',  ( -1.000000000000000000, 0.000000000000000000, 0.000000000000000000 ) ) ;
#41686 = ORIENTED_EDGE ( 'NONE', *, *, #34184, .T. ) ;
#41687 = LINE ( 'NONE', #24352, #26115 ) ;
#41688 = CARTESIAN_POINT ( 'NONE',  ( 120.9649014775786355, -3.383040157471821630, -19.15922257007629170 ) ) ;
#41689 = CARTESIAN_POINT ( 'NONE',  ( 112.3424481442453384, -6.344957434206662583, -7.627207830600332805 ) ) ;
#41690 = CARTESIAN_POINT ( 'NONE',  ( 118.9227414775786542, 0.4262465694468514643, -12.03445270309931736 ) ) ;
#41691 =( NAMED_UNIT ( * ) SI_UNIT ( $, .STERADIAN. ) SOLID_ANGLE_UNIT ( ) );
#41692 = CARTESIAN_POINT ( 'NONE',  ( 123.4608748109119745, -10.63000616557722466, -14.87417383870573495 ) ) ;
#41693 = CARTESIAN_POINT ( 'NONE',  ( 119.0929214775786278, -5.638512984488999180, -18.83840828888717311 ) ) ;
#41694 = CARTESIAN_POINT ( 'NONE',  ( 106.3848327545248651, -6.936859964151250502, -8.388885654883777576 ) ) ;
#41695 = CARTESIAN_POINT ( 'NONE',  ( 111.4915481442453142, -1.833838273342658365, -17.42832698103878286 ) ) ;
#41696 = PRODUCT_RELATED_PRODUCT_CATEGORY ( 'part', '', ( #10294 ) ) ;
#41697 = DIRECTION ( 'NONE',  ( 1.000000000000000000, 0.000000000000000000, -0.000000000000000000 ) ) ;
#41698 = VERTEX_POINT ( 'NONE', #36098 ) ;
#41699 = CARTESIAN_POINT ( 'NONE',  ( 119.3198281442452924, 0.5811942927096110934, -14.16772938898807510 ) ) ;
#41700 = CARTESIAN_POINT ( 'NONE',  ( 61.05647571779960003, -46.63990697477660063, -14.39321520033831625 ) ) ;
#41701 = CARTESIAN_POINT ( 'NONE',  ( 116.8805814775786445, -6.344957434206662583, -7.627207830600332805 ) ) ;
#41702 = ORIENTED_EDGE ( 'NONE', *, *, #25429, .F. ) ;
#41703 = CARTESIAN_POINT ( 'NONE',  ( 114.9275671295247889, -10.62599879583958540, -13.39321520033831447 ) ) ;
#41704 = CARTESIAN_POINT ( 'NONE',  ( 126.0703014775786102, -9.988377603198980381, -10.36322818467138518 ) ) ;
#41705 = DIRECTION ( 'NONE',  ( -0.3445294493088569276, -0.9387755102040827859, 0.000000000000000000 ) ) ;
#41706 = CARTESIAN_POINT ( 'NONE',  ( 125.3400398954497632, -6.228147054556873563, -18.69629702666285809 ) ) ;
#41707 =( BOUNDED_CURVE ( )  B_SPLINE_CURVE ( 3, ( #16928, #19487, #41105, #7096 ),
 .UNSPECIFIED., .F., .F. ) 
 B_SPLINE_CURVE_WITH_KNOTS ( ( 4, 4 ),
 ( 0.000000000000000000, 1.570796326794895004 ),
 .UNSPECIFIED. ) 
 CURVE ( )  GEOMETRIC_REPRESENTATION_ITEM ( )  RATIONAL_B_SPLINE_CURVE ( ( 1.000000000000000000, 0.8047378541243659367, 0.8047378541243659367, 1.000000000000000000 ) ) 
 REPRESENTATION_ITEM ( '' )  );
#41708 = CARTESIAN_POINT ( 'NONE',  ( 77.38862445244474486, -56.64805777995697156, -1.793693935343831258 ) ) ;
#41709 = CARTESIAN_POINT ( 'NONE',  ( 119.7169148109119874, -0.1624402480850797581, -16.17319339645315424 ) ) ;
#41710 = DIRECTION ( 'NONE',  ( 0.000000000000000000, 0.000000000000000000, -1.000000000000000000 ) ) ;
#41711 = VECTOR ( 'NONE', #2239, 1000.000000000000000 ) ;
#41712 = CARTESIAN_POINT ( 'NONE',  ( 117.3343948109119737, -6.222761293078241884, -8.102969835052219238 ) ) ;
#41713 = AXIS2_PLACEMENT_3D ( 'NONE', #25633, #40438, #15812 ) ;
#41714 = CARTESIAN_POINT ( 'NONE',  ( 121.0751082044368303, -6.247802574075781656, -18.73351920797576042 ) ) ;
#41715 = CARTESIAN_POINT ( 'NONE',  ( 120.6812681442452941, 0.1319031606808879209, -14.10382304977623669 ) ) ;
#41716 = CARTESIAN_POINT ( 'NONE',  ( 116.2565881442452991, -9.261995988541697145, -16.69588392320189030 ) ) ;
#41717 = B_SPLINE_CURVE_WITH_KNOTS ( 'NONE', 3,
 ( #1527, #22289, #43268, #25266, #4505, #12034, #18427, #25936, #22508, #42372, #19088, #11133, #7699, #38928, #11582, #32319, #1084, #14998, #24269, #3279, #26385, #24046, #16756, #37939, #1978, #15674, #29803, #31094, #17202, #5402, #30652, #13336, #27240 ),
 .UNSPECIFIED., .F., .F.,
 ( 4, 2, 2, 2, 1, 1, 1, 1, 2, 2, 2, 2, 1, 1, 1, 1, 1, 2, 2, 2, 4 ),
 ( 0.000000000000000000, 0.2500000000003253509, 0.3750000000004861112, 0.4375000000005684342, 0.4687500000006095124, 0.4843750000006301071, 0.4921875000006404322, 0.4960937500006456502, 0.4980468750006464274, 0.5000000000006471490, 0.6250000000005297984, 0.6875000000004711787, 0.7187500000004417577, 0.7343750000004271028, 0.7421875000004197753, 0.7460937500004142242, 0.7480468750004114487, 0.7490234375004118927, 0.7500000000004123368, 0.8750000000002061684, 1.000000000000000000 ),
 .UNSPECIFIED. ) ;
#41718 = CARTESIAN_POINT ( 'NONE',  ( 117.2776681442452968, -4.153390946401321671, -8.397313243818183892 ) ) ;
#41719 = EDGE_LOOP ( 'NONE', ( #43108, #33704, #5100, #5434 ) ) ;
#41720 = CARTESIAN_POINT ( 'NONE',  ( 115.1220548109119761, -8.166667518702817929, -8.995218007635861213 ) ) ;
#41721 = CARTESIAN_POINT ( 'NONE',  ( 115.9693640045247776, 0.1403307496149616695, -15.46607636864997204 ) ) ;
#41722 = CARTESIAN_POINT ( 'NONE',  ( 116.0086969107182142, -2.467220198592777525, -17.83387418641524391 ) ) ;
#41723 = CIRCLE ( 'NONE', #19153, 0.2499999999999990841 ) ;
#41724 = CARTESIAN_POINT ( 'NONE',  ( 105.4124890045248293, -9.868328341294098749, -11.32035403202665869 ) ) ;
#41725 = CARTESIAN_POINT ( 'NONE',  ( 123.1815811593281751, -8.517053830703076756, -17.59134500557230396 ) ) ;
#41726 = CARTESIAN_POINT ( 'NONE',  ( 123.9146881442452894, 0.9020085738987339008, -11.91225656197089222 ) ) ;
#41727 = VERTEX_POINT ( 'NONE', #4641 ) ;
#41728 = CARTESIAN_POINT ( 'NONE',  ( 127.1653849502245350, -8.988304812967710333, -9.794650042750394192 ) ) ;
#41729 = CARTESIAN_POINT ( 'NONE',  ( 117.0507614775786465, 0.1319031606808879209, -14.10382304977623669 ) ) ;
#41730 = LINE ( 'NONE', #17771, #193 ) ;
#41731 = CARTESIAN_POINT ( 'NONE',  ( 59.36680634945872725, -12.84644995903807896, -17.39321520033831447 ) ) ;
#41732 = CARTESIAN_POINT ( 'NONE',  ( 122.0994348109119443, 0.9020085738987339008, -11.91225656197089222 ) ) ;
#41733 = CARTESIAN_POINT ( 'NONE',  ( 113.3301452545248083, -9.868328341294098749, -15.46607636864997204 ) ) ;
#41734 = CARTESIAN_POINT ( 'NONE',  ( 89.28805143673710631, -9.905285955282378652, -13.44403546754823786 ) ) ;
#41735 = ORIENTED_EDGE ( 'NONE', *, *, #13758, .F. ) ;
#41736 = DIRECTION ( 'NONE',  ( 0.000000000000000000, 0.9242245927363041957, 0.3818493186865896116 ) ) ;
#41737 = CARTESIAN_POINT ( 'NONE',  ( 112.6828081442453282, -7.893985811506177619, -18.51759400769804742 ) ) ;
#41738 = CARTESIAN_POINT ( 'NONE',  ( 123.4608748109119745, -10.63000616557722466, -14.87417383870573495 ) ) ;
#41739 = CARTESIAN_POINT ( 'NONE',  ( 116.9373081442452929, -1.833838273342659253, -17.42832698103878286 ) ) ;
#41740 = CARTESIAN_POINT ( 'NONE',  ( 70.19189222814998175, -66.20485342690169261, -45.06987807991856698 ) ) ;
#41741 = CARTESIAN_POINT ( 'NONE',  ( 117.5613014775786525, 0.9020085738987339008, -11.91225656197089222 ) ) ;
#41742 = DIRECTION ( 'NONE',  ( -1.165517335421915886E-15, -1.000000000000000000, -1.010925141707166031E-30 ) ) ;
#41743 = CARTESIAN_POINT ( 'NONE',  ( 123.7445081442452874, -7.894159318335828068, -9.358103419637847864 ) ) ;
#41744 = ORIENTED_EDGE ( 'NONE', *, *, #9989, .T. ) ;
#41745 = EDGE_CURVE ( 'NONE', #31784, #7134, #4065, .T. ) ;
#41746 = EDGE_CURVE ( 'NONE', #38238, #24192, #11951, .T. ) ;
#41747 = AXIS2_PLACEMENT_3D ( 'NONE', #36356, #5127, #19043 ) ;
#41748 = CARTESIAN_POINT ( 'NONE',  ( 116.5952498694597921, -9.864550231015533299, -13.34038451353460886 ) ) ;
#41749 = AXIS2_PLACEMENT_3D ( 'NONE', #42953, #35645, #35184 ) ;
#41750 = CARTESIAN_POINT ( 'NONE',  ( 118.3554748109119998, 0.2603800115204892296, -16.42320221600525088 ) ) ;
#41751 = CARTESIAN_POINT ( 'NONE',  ( 124.1983214775786166, -1.833838273342659697, -17.42832698103878286 ) ) ;
#41752 = VERTEX_POINT ( 'NONE', #8079 ) ;
#41753 = CARTESIAN_POINT ( 'NONE',  ( 123.9106423109119675, -9.959231468620755479, -10.70263013195267199 ) ) ;
#41754 = CARTESIAN_POINT ( 'NONE',  ( 137.2865145795275339, -1.213646807504741520, -9.647614279156686123 ) ) ;
#41755 = CARTESIAN_POINT ( 'NONE',  ( 121.1350814775786233, 0.5811942927096110934, -14.16772938898807510 ) ) ;
#41756 = CARTESIAN_POINT ( 'NONE',  ( 106.3153796295248412, -4.863998795839590272, -19.15521520033831493 ) ) ;
#41757 = CARTESIAN_POINT ( 'NONE',  ( 121.1918081442452859, -10.15424416112533912, -14.75197769757731336 ) ) ;
#41758 = ORIENTED_EDGE ( 'NONE', *, *, #33350, .T. ) ;
#41759 = ORIENTED_EDGE ( 'NONE', *, *, #3745, .F. ) ;
#41760 = CARTESIAN_POINT ( 'NONE',  ( 115.7460481442453357, 0.9020085738987339008, -11.91225656197089222 ) ) ;
#41761 = B_SPLINE_CURVE_WITH_KNOTS ( 'NONE', 3,
 ( #23782, #36973, #44523, #16712, #13287, #40424, #41113, #17536, #23314, #7262 ),
 .UNSPECIFIED., .F., .F.,
 ( 4, 3, 3, 4 ),
 ( 1.939479807224430197E-18, 0.0001671877548681299829, 0.0003343755096277730159, 0.0006463528481650649771 ),
 .UNSPECIFIED. ) ;
#41762 = CARTESIAN_POINT ( 'NONE',  ( 124.7088614775786226, -9.565557343593413364, -10.61323700422348004 ) ) ;
#41763 = DIRECTION ( 'NONE',  ( -0.9970811988817435134, 0.07634843047859724008, 0.000000000000000000 ) ) ;
#41764 = CARTESIAN_POINT ( 'NONE',  ( 87.44708369096657918, -21.99489077589588604, -18.39321520033831803 ) ) ;
#41765 = CARTESIAN_POINT ( 'NONE',  ( 120.5110881442453206, -6.344957434206665248, -7.627207830600338134 ) ) ;
#41766 = EDGE_CURVE ( 'NONE', #7363, #31995, #26615, .T. ) ;
#41767 = CARTESIAN_POINT ( 'NONE',  ( 63.69189222814998175, -55.76602098829192755, -2.607500914624014232 ) ) ;
#41768 = DIRECTION ( 'NONE',  ( 0.9908103287288504424, -0.1352586133457950590, 0.000000000000000000 ) ) ;
#41769 = CARTESIAN_POINT ( 'NONE',  ( 123.8579614775786126, 0.5811942927096110934, -14.16772938898807510 ) ) ;
#41771 = CARTESIAN_POINT ( 'NONE',  ( 121.9859814775786333, -9.565557343593413364, -10.61323700422348004 ) ) ;
#41770 = CARTESIAN_POINT ( 'NONE',  ( 117.5045748109119756, 0.5811942927096110934, -14.16772938898807510 ) ) ;
#41772 = CARTESIAN_POINT ( 'NONE',  ( 121.5321681442453183, -0.1624402480850797581, -16.17319339645315424 ) ) ;
#41773 = CARTESIAN_POINT ( 'NONE',  ( 69.63874157094764428, -25.41500789246203951, -5.785566283887345840 ) ) ;
#41774 = CARTESIAN_POINT ( 'NONE',  ( 114.3846081442453197, -10.63000616557722466, -14.87417383870573495 ) ) ;
#41775 = EDGE_CURVE ( 'NONE', #44431, #18777, #17915, .T. ) ;
#41776 = ORIENTED_EDGE ( 'NONE', *, *, #8870, .T. ) ;
#41777 = AXIS2_PLACEMENT_3D ( 'NONE', #39661, #42414, #38975 ) ;
#41778 = EDGE_CURVE ( 'NONE', #26284, #25225, #39082, .T. ) ;
#41779 = DIRECTION ( 'NONE',  ( 0.9609149988134839671, -0.1028163501681660097, 0.2570431154366504822 ) ) ;
#41780 = CARTESIAN_POINT ( 'NONE',  ( 107.9822546295247889, -4.863998795839590272, -7.631215200338315796 ) ) ;
#41781 = AXIS2_PLACEMENT_3D ( 'NONE', #19233, #33116, #36764 ) ;
#41782 = CARTESIAN_POINT ( 'NONE',  ( 106.9404577545248145, -2.791137627527939813, -18.39754474579286025 ) ) ;
#41783 = CARTESIAN_POINT ( 'NONE',  ( 115.9693640045247776, 0.1403307496149616695, -15.46607636864997204 ) ) ;
#41784 = CARTESIAN_POINT ( 'NONE',  ( 124.9252281442453238, -8.862178061931794915, -16.39564131203325559 ) ) ;
#41785 = CARTESIAN_POINT ( 'NONE',  ( 126.6942948109119840, -8.899110576539710493, -16.42337572283490132 ) ) ;
#41786 = EDGE_LOOP ( 'NONE', ( #34493, #6446, #40686, #12086, #18530 ) ) ;
#41787 = CARTESIAN_POINT ( 'NONE',  ( 123.2339681442453241, -6.344957434206665248, -7.627207830600338134 ) ) ;
#41788 = CARTESIAN_POINT ( 'NONE',  ( 110.2047546295247855, -4.863998795839590272, -7.631215200338315796 ) ) ;
#41789 = CARTESIAN_POINT ( 'NONE',  ( 73.53114257624162065, -54.10809544429395856, -19.39321520033831447 ) ) ;
#41790 = CARTESIAN_POINT ( 'NONE',  ( 123.0637881442452937, -0.4660016031367893996, -10.09054647747474043 ) ) ;
#41791 = CARTESIAN_POINT ( 'NONE',  ( 126.2404814775786264, -9.261995988541697145, -16.69588392320189030 ) ) ;
#41792 = FACE_OUTER_BOUND ( 'NONE', #33407, .T. ) ;
#41793 = CARTESIAN_POINT ( 'NONE',  ( 112.5693548109119888, -10.63000616557722466, -14.87417383870573495 ) ) ;
#41794 = EDGE_CURVE ( 'NONE', #3780, #14434, #31785, .T. ) ;
#41795 = CARTESIAN_POINT ( 'NONE',  ( 113.8163171295247764, -10.62599879583958540, -13.39321520033831447 ) ) ;
#41796 = CARTESIAN_POINT ( 'NONE',  ( 106.3848327545248651, -2.477300249445798297, -19.15521520033831138 ) ) ;
#41797 = ORIENTED_EDGE ( 'NONE', *, *, #40661, .T. ) ;
#41798 = CIRCLE ( 'NONE', #39604, 2.999999999999999556 ) ;
#41799 = CARTESIAN_POINT ( 'NONE',  ( 83.83554121260367253, -25.99489077589524300, -13.39321520033831625 ) ) ;
#41800 = CARTESIAN_POINT ( 'NONE',  ( 115.1220548109119761, -1.833838273342658809, -17.42832698103878286 ) ) ;
#41801 = CARTESIAN_POINT ( 'NONE',  ( 114.0442481442453300, -1.834011780172310813, -8.268836392978581529 ) ) ;
#41802 = CARTESIAN_POINT ( 'NONE',  ( 114.2330358795247776, -0.7896495226426338832, -17.46756447353520159 ) ) ;
#41803 = CARTESIAN_POINT ( 'NONE',  ( 106.1764733795248219, -1.325403438956436419, -9.854619843455211026 ) ) ;
#41804 = EDGE_CURVE ( 'NONE', #4353, #22394, #40519, .T. ) ;
#41805 = CARTESIAN_POINT ( 'NONE',  ( 121.3052614775786111, -7.643976991954077427, -18.09477374809248928 ) ) ;
#41806 = CARTESIAN_POINT ( 'NONE',  ( 118.0718414775786442, -0.8288870151387760510, -10.36305467784173118 ) ) ;
#41807 = CARTESIAN_POINT ( 'NONE',  ( 113.3635281442453504, -0.1624402480850797581, -16.17319339645315424 ) ) ;
#41808 = ORIENTED_EDGE ( 'NONE', *, *, #36446, .F. ) ;
#41809 = EDGE_CURVE ( 'NONE', #3847, #10734, #41377, .T. ) ;
#41810 = EDGE_CURVE ( 'NONE', #42505, #20212, #39755, .T. ) ;
#41811 = CARTESIAN_POINT ( 'NONE',  ( 120.2990798109119766, -7.200787124940443817, -17.81845355600750835 ) ) ;
#41812 = CARTESIAN_POINT ( 'NONE',  ( 78.69189222814998175, -46.76310523276723785, -4.893215200338314474 ) ) ;
#41813 = CARTESIAN_POINT ( 'NONE',  ( 113.9875214775786532, -8.899110576539710493, -16.42337572283490132 ) ) ;
#41814 = EDGE_LOOP ( 'NONE', ( #22383, #17412, #43611, #35532, #40853 ) ) ;
#41815 = DIRECTION ( 'NONE',  ( -1.000000000000000000, 0.000000000000000000, 0.000000000000000000 ) ) ;
#41816 = VECTOR ( 'NONE', #5732, 1000.000000000000114 ) ;
#41817 = CARTESIAN_POINT ( 'NONE',  ( 111.1770983795247787, -8.402594152722688392, -16.93181055722141792 ) ) ;
#41818 = VERTEX_POINT ( 'NONE', #37219 ) ;
#41819 = CARTESIAN_POINT ( 'NONE',  ( 118.2987481442453088, -7.894159318335828068, -9.358103419637847864 ) ) ;
#41820 = CARTESIAN_POINT ( 'NONE',  ( 114.0442481442453300, -7.643976991954077427, -18.09477374809248928 ) ) ;
#41821 = CARTESIAN_POINT ( 'NONE',  ( 124.2579079359120016, -4.360204210389833968, -8.000047426360245240 ) ) ;
#41822 = VERTEX_POINT ( 'NONE', #26531 ) ;
#41823 = CARTESIAN_POINT ( 'NONE',  ( 90.67797751089673852, -17.83979763915464289, -20.89321520033831447 ) ) ;
#41824 = CARTESIAN_POINT ( 'NONE',  ( 123.9584548109119737, 0.04957186715663468302, -7.079989135975798042 ) ) ;
#41825 = CARTESIAN_POINT ( 'NONE',  ( 106.9404577545248145, -2.791137627527939813, -18.39754474579286025 ) ) ;
#41826 = CARTESIAN_POINT ( 'NONE',  ( 118.2062230939976644, -2.236191541394346061, -18.14152338500401029 ) ) ;
#41827 = CARTESIAN_POINT ( 'NONE',  ( 121.9292548109119849, -7.894159318335828068, -9.358103419637847864 ) ) ;
#41828 = CARTESIAN_POINT ( 'NONE',  ( 119.1496481442453046, -6.222761293078241884, -8.102969835052219238 ) ) ;
#41829 = DIRECTION ( 'NONE',  ( 0.000000000000000000, 0.9284778069183720062, 0.3713878862591650232 ) ) ;
#41830 = ORIENTED_EDGE ( 'NONE', *, *, #16682, .T. ) ;
#41831 = CARTESIAN_POINT ( 'NONE',  ( 116.6766162288780890, -8.450459793919360862, -16.99402653318119505 ) ) ;
#41832 = CARTESIAN_POINT ( 'NONE',  ( 117.2209414775786485, -2.084020599724406786, -8.691656652584148546 ) ) ;
#41833 = DIRECTION ( 'NONE',  ( 0.9063289528979890930, 0.4225728684367167087, 0.000000000000000000 ) ) ;
#41834 = CARTESIAN_POINT ( 'NONE',  ( 85.19105201044544629, -29.19355814263353821, -9.935028317583610047 ) ) ;
#41835 = CARTESIAN_POINT ( 'NONE',  ( 116.2659068881580708, -12.01880880694303855, -4.893215200338314474 ) ) ;
#41836 = CARTESIAN_POINT ( 'NONE',  ( 115.9729548109119861, -6.344957434206662583, -7.627207830600332805 ) ) ;
#41837 = ORIENTED_EDGE ( 'NONE', *, *, #30909, .F. ) ;
#41838 = CARTESIAN_POINT ( 'NONE',  ( 113.4769814775786330, -10.63000616557722466, -14.87417383870573495 ) ) ;
#41839 = DIRECTION ( 'NONE',  ( 1.000000000000000000, 0.000000000000000000, 0.000000000000000000 ) ) ;
#41840 = CARTESIAN_POINT ( 'NONE',  ( 110.1353015045248469, -2.477300249445798297, -7.631215200338321125 ) ) ;
#41841 = CARTESIAN_POINT ( 'NONE',  ( 113.9875214775786532, -0.4660016031367893996, -10.09054647747474043 ) ) ;
#41842 = EDGE_CURVE ( 'NONE', #17452, #2933, #31746, .T. ) ;
#41843 = CARTESIAN_POINT ( 'NONE',  ( 113.7038881442453402, -3.383040157471821630, -19.15922257007629170 ) ) ;
#41844 = CARTESIAN_POINT ( 'NONE',  ( 125.3895814775786448, -2.084020599724406786, -8.691656652584148546 ) ) ;
#41845 = DIRECTION ( 'NONE',  ( 0.9609149988134833009, -0.1028163501681649411, 0.2570431154366530913 ) ) ;
#41846 = CARTESIAN_POINT ( 'NONE',  ( 108.8156921295247912, -9.868328341294093420, -13.39321520033831447 ) ) ;
#41847 = CARTESIAN_POINT ( 'NONE',  ( 111.0001630180080809, 0.7607806665038616689, -14.64321520033831447 ) ) ;
#41848 = CARTESIAN_POINT ( 'NONE',  ( 109.2294481158511275, -7.112626342048868899, -18.18810309623751564 ) ) ;
#41849 = CARTESIAN_POINT ( 'NONE',  ( 115.5758681442453053, -7.894159318335828068, -9.358103419637847864 ) ) ;
#41850 = LINE ( 'NONE', #10610, #11639 ) ;
#41851 = CARTESIAN_POINT ( 'NONE',  ( 117.0111608795247946, -1.325403438956436419, -16.93181055722141792 ) ) ;
#41852 = CARTESIAN_POINT ( 'NONE',  ( 107.9822546295247889, -4.863998795839590272, -7.631215200338315796 ) ) ;
#41853 = CARTESIAN_POINT ( 'NONE',  ( 126.5041214912238416, -4.774006015657890067, -8.251167430307914330 ) ) ;
#41854 = CARTESIAN_POINT ( 'NONE',  ( 125.5597614775786326, -1.561330072975669392, -17.79121239304076951 ) ) ;
#41855 = CARTESIAN_POINT ( 'NONE',  ( 136.4689272580744444, 0.8652765085456386451, -12.77968882490968561 ) ) ;
#41856 = CARTESIAN_POINT ( 'NONE',  ( 121.4187148109119789, -6.344957434206665248, -7.627207830600338134 ) ) ;
#41857 = CARTESIAN_POINT ( 'NONE',  ( 116.3133148109119759, -7.893985811506177619, -18.51759400769804742 ) ) ;
#41858 = EDGE_LOOP ( 'NONE', ( #14826, #20837, #25815, #1486, #22306, #33758 ) ) ;
#41859 = CARTESIAN_POINT ( 'NONE',  ( 116.2565881442453133, -0.8288870151387760510, -10.36305467784173118 ) ) ;
#41860 = CARTESIAN_POINT ( 'NONE',  ( 122.5532481442453019, -10.63000616557722466, -14.87417383870573495 ) ) ;
#41861 = CARTESIAN_POINT ( 'NONE',  ( 118.2420214775786320, -3.383040157471821630, -19.15922257007629170 ) ) ;
#41862 = CARTESIAN_POINT ( 'NONE',  ( 115.2922348109119781, 0.4262465694468514643, -12.03445270309931736 ) ) ;
#41863 = ORIENTED_EDGE ( 'NONE', *, *, #30988, .F. ) ;
#41864 = EDGE_CURVE ( 'NONE', #36515, #38150, #8481, .T. ) ;
#41865 = CARTESIAN_POINT ( 'NONE',  ( 119.5467348109119712, -5.574606645277164318, -18.38911715685844683 ) ) ;
#41866 = AXIS2_PLACEMENT_3D ( 'NONE', #27529, #24549, #42327 ) ;
#41867 = CARTESIAN_POINT ( 'NONE',  ( 115.7460481442453357, 0.9020085738987339008, -11.91225656197089222 ) ) ;
#41868 = CARTESIAN_POINT ( 'NONE',  ( 136.9144124994549259, 0.3076051572492725650, -15.33370174593263435 ) ) ;
#41869 = CARTESIAN_POINT ( 'NONE',  ( 113.0523327545247838, -2.477300249445798297, -19.15521520033831138 ) ) ;
#41870 = CARTESIAN_POINT ( 'NONE',  ( 61.76986277844709861, -39.32091226840162079, -4.893215200338314474 ) ) ;
#41871 = DIRECTION ( 'NONE',  ( -0.8949343913984424415, 0.4123869368673875324, 0.1703803081152070742 ) ) ;
#41872 = DIRECTION ( 'NONE',  ( 0.000000000000000000, -0.3818493186865927203, 0.9242245927363029745 ) ) ;
#41873 = CARTESIAN_POINT ( 'NONE',  ( 116.3700414775786527, -5.638512984488999180, -18.83840828888717311 ) ) ;
#41874 = CARTESIAN_POINT ( 'NONE',  ( 136.7082020370515636, -10.48511845154063593, -13.91967875158812973 ) ) ;
#41875 = CYLINDRICAL_SURFACE ( 'NONE', #314, 3.000000000000001776 ) ;
#41876 = CARTESIAN_POINT ( 'NONE',  ( 64.08833547316721990, -12.91438983140282559, -15.87665273277405831 ) ) ;
#41877 = CARTESIAN_POINT ( 'NONE',  ( 67.19031194842951038, -1.707697914625855296, -14.39321520033831625 ) ) ;
#41878 = CARTESIAN_POINT ( 'NONE',  ( 113.8163171295247764, 0.1403307496149613920, -13.39321520033831447 ) ) ;
#41879 = CARTESIAN_POINT ( 'NONE',  ( 118.2420214775786320, -3.383040157471821630, -19.15922257007629170 ) ) ;
#41880 = DIRECTION ( 'NONE',  ( -0.5040994586965557023, -0.8636456077245108220, 0.000000000000000000 ) ) ;
#41881 = CARTESIAN_POINT ( 'NONE',  ( 121.9470836909669913, -24.14644159042263993, -12.62951656296512937 ) ) ;
#41882 = CARTESIAN_POINT ( 'NONE',  ( 119.1871698793805194, -2.191907684172563986, -18.20049396185734025 ) ) ;
#41883 = FACE_OUTER_BOUND ( 'NONE', #24920, .T. ) ;
#41884 = CARTESIAN_POINT ( 'NONE',  ( 120.9081748109119872, -4.153390946401325223, -8.397313243818185668 ) ) ;
#41885 = ORIENTED_EDGE ( 'NONE', *, *, #2425, .F. ) ;
#41886 = CARTESIAN_POINT ( 'NONE',  ( 125.1626748109119802, -9.988377603198980381, -10.36322818467138518 ) ) ;
#41887 = CARTESIAN_POINT ( 'NONE',  ( 122.4965214775786251, -10.30919188438810075, -12.61870101168855918 ) ) ;
#41888 = CARTESIAN_POINT ( 'NONE',  ( 91.77400275106518279, -27.84333996136784961, -14.15691383771150136 ) ) ;
#41889 = CARTESIAN_POINT ( 'NONE',  ( 114.7816948109119863, -9.859900752359374465, -12.68260735090039404 ) ) ;
#41890 =( BOUNDED_SURFACE ( )  B_SPLINE_SURFACE ( 3, 2, ( 
 ( #20143, #44988, #23792 ),
 ( #41354, #26752, #40659 ),
 ( #10110, #13747, #23567 ),
 ( #44316, #24014, #37902 ) ),
 .UNSPECIFIED., .F., .F., .T. ) 
 B_SPLINE_SURFACE_WITH_KNOTS ( ( 4, 4 ),
 ( 3, 3 ),
 ( 1.522649623061655300, 1.570796326794896558 ),
 ( 0.000000000000000000, 1.000000000000000000 ),
 .UNSPECIFIED. ) 
 GEOMETRIC_REPRESENTATION_ITEM ( )  RATIONAL_B_SPLINE_SURFACE ( (
 ( 1.000000000000000000, 0.7145271066604789167, 1.000000000000000000),
 ( 1.000000000000000000, 0.7120684114869153536, 1.000000000000000000),
 ( 1.000000000000000000, 0.7095941637304922223, 1.000000000000000000),
 ( 1.000000000000000000, 0.7071067811865475727, 1.000000000000000000) ) ) 
 REPRESENTATION_ITEM ( '' )  SURFACE ( )  );
#41891 = CARTESIAN_POINT ( 'NONE',  ( 114.3278814775786429, 0.1319031606808879209, -14.10382304977623669 ) ) ;
#41892 = CARTESIAN_POINT ( 'NONE',  ( 106.7320983795247855, -8.402594152722688392, -16.93181055722141792 ) ) ;
#41893 = CARTESIAN_POINT ( 'NONE',  ( 110.7603796295247918, -4.863998795839590272, -19.15521520033831493 ) ) ;
#41894 = CARTESIAN_POINT ( 'NONE',  ( 119.7736414775786358, 0.1319031606808879209, -14.10382304977623669 ) ) ;
#41895 = CARTESIAN_POINT ( 'NONE',  ( 121.5321681442453183, -0.1624402480850797581, -16.17319339645315424 ) ) ;
#41896 = CARTESIAN_POINT ( 'NONE',  ( 151.2860562277021472, -4.863998795839242995, -13.39321520033831447 ) ) ;
#41897 = CARTESIAN_POINT ( 'NONE',  ( 109.2294421295247844, 0.2400687412228638684, -12.14321520033831625 ) ) ;
#41898 = CARTESIAN_POINT ( 'NONE',  ( 119.8129079359119942, -5.444069387712269226, -19.60292469916370450 ) ) ;
#41899 = CARTESIAN_POINT ( 'NONE',  ( 106.9404577545248145, -2.791137627527939813, -18.39754474579286025 ) ) ;
#41900 = CARTESIAN_POINT ( 'NONE',  ( 117.1221491469711964, 1.552509864743009782, -21.40721312732405934 ) ) ;
#41901 = CARTESIAN_POINT ( 'NONE',  ( 112.1722681442453222, -0.4660016031367893996, -10.09054647747474043 ) ) ;
#41902 = CARTESIAN_POINT ( 'NONE',  ( 113.1366214775786432, -1.834011780172310813, -8.268836392978581529 ) ) ;
#41903 = CARTESIAN_POINT ( 'NONE',  ( 112.7745202545247878, -10.62599879583958717, -15.77991374673208469 ) ) ;
#41904 = CARTESIAN_POINT ( 'NONE',  ( 121.9659548109119811, -2.527210466738041728, -8.967976844669124148 ) ) ;
#41905 = ORIENTED_EDGE ( 'NONE', *, *, #32827, .F. ) ;
#41906 = CARTESIAN_POINT ( 'NONE',  ( 94.20708369096698220, -25.99489077589524300, -13.39321520033831447 ) ) ;
#41907 = CONICAL_SURFACE ( 'NONE', #44090, 1.610000000000000986, 0.9599310885968765916 ) ;
#41908 = CARTESIAN_POINT ( 'NONE',  ( 120.4543614775786295, -4.089484607189486809, -7.948022111789456723 ) ) ;
#41909 = CARTESIAN_POINT ( 'NONE',  ( 113.8173414775786512, 0.2603800115204892296, -16.42320221600525088 ) ) ;
#41910 = EDGE_CURVE ( 'NONE', #42200, #26749, #36366, .T. ) ;
#41911 = CARTESIAN_POINT ( 'NONE',  ( 122.9503348109119827, -9.859900752359378018, -12.68260735090039759 ) ) ;
#41912 =( NAMED_UNIT ( * ) SI_UNIT ( $, .STERADIAN. ) SOLID_ANGLE_UNIT ( ) );
#41913 = CARTESIAN_POINT ( 'NONE',  ( 111.7184548109119788, -0.8288870151387760510, -10.36305467784173118 ) ) ;
#41914 = CARTESIAN_POINT ( 'NONE',  ( 117.1074881442453233, -10.63000616557722466, -14.87417383870573495 ) ) ;
#41915 = CARTESIAN_POINT ( 'NONE',  ( 107.7738952545248310, -9.868328341294098749, -15.46607636864997204 ) ) ;
#41916 = CARTESIAN_POINT ( 'NONE',  ( 113.3068014775786594, -1.833838273342658809, -17.42832698103878286 ) ) ;
#41917 = ORIENTED_EDGE ( 'NONE', *, *, #25319, .F. ) ;
#41918 = CARTESIAN_POINT ( 'NONE',  ( 119.9438214775786378, -7.893985811506177619, -18.51759400769804742 ) ) ;
#41919 = DIRECTION ( 'NONE',  ( 0.000000000000000000, 0.000000000000000000, -1.000000000000000000 ) ) ;
#41920 = CARTESIAN_POINT ( 'NONE',  ( 117.3343948109119737, -3.383040157471821630, -19.15922257007629170 ) ) ;
#41921 = AXIS2_PLACEMENT_3D ( 'NONE', #38319, #3006, #44514 ) ;
#41922 = ORIENTED_EDGE ( 'NONE', *, *, #19165, .F. ) ;
#41923 = CARTESIAN_POINT ( 'NONE',  ( 106.3848327545248651, -6.936859964151250502, -8.388885654883777576 ) ) ;
#41924 = CARTESIAN_POINT ( 'NONE',  ( 124.5386814775786206, -5.638512984488999180, -18.83840828888717311 ) ) ;
#41925 = EDGE_CURVE ( 'NONE', #31472, #23145, #17216, .T. ) ;
#41926 = FACE_OUTER_BOUND ( 'NONE', #27329, .T. ) ;
#41927 = CARTESIAN_POINT ( 'NONE',  ( 112.7395348109119766, -4.153390946401321671, -8.397313243818183892 ) ) ;
#41928 = CARTESIAN_POINT ( 'NONE',  ( 77.01163399656647357, -56.15206630274370525, -2.229255299424385939 ) ) ;
#41929 = CARTESIAN_POINT ( 'NONE',  ( 120.9081748109119872, -4.153390946401325223, -8.397313243818185668 ) ) ;
#41930 = DIRECTION ( 'NONE',  ( -0.9970811988817434024, 0.07634843047859753151, 0.000000000000000000 ) ) ;
#41931 = AXIS2_PLACEMENT_3D ( 'NONE', #31809, #17689, #35673 ) ;
#41932 = CARTESIAN_POINT ( 'NONE',  ( 121.1350814775786233, -9.859900752359378018, -12.68260735090039759 ) ) ;
#41933 = AXIS2_PLACEMENT_3D ( 'NONE', #899, #4543, #24852 ) ;
#41934 = CARTESIAN_POINT ( 'NONE',  ( 125.0849378844219046, -10.94598263288078321, -9.020557899002023206 ) ) ;
#41935 = CARTESIAN_POINT ( 'NONE',  ( 120.9081748109119872, -4.153390946401325223, -8.397313243818185668 ) ) ;
#41936 = CARTESIAN_POINT ( 'NONE',  ( 123.8411891859119862, -8.844754642576884152, -8.592115655440050404 ) ) ;
#41937 = CARTESIAN_POINT ( 'NONE',  ( 116.8805814775786445, -6.344957434206662583, -7.627207830600332805 ) ) ;
#41938 = CARTESIAN_POINT ( 'NONE',  ( 123.2906948109119867, -8.166667518702798390, -8.995218007635845225 ) ) ;
#41939 = CARTESIAN_POINT ( 'NONE',  ( 120.3409081442453044, -8.899110576539710493, -16.42337572283490132 ) ) ;
#41940 = ORIENTED_EDGE ( 'NONE', *, *, #14761, .F. ) ;
#41941 = CARTESIAN_POINT ( 'NONE',  ( 116.3133148109119759, -7.893985811506177619, -18.51759400769804742 ) ) ;
#41942 = CARTESIAN_POINT ( 'NONE',  ( 109.3713171295247832, -10.62599879583958540, -13.39321520033831447 ) ) ;
#41943 = DIRECTION ( 'NONE',  ( 0.9986099732815399976, 0.05270788615228315377, 0.000000000000000000 ) ) ;
#41944 = CARTESIAN_POINT ( 'NONE',  ( 123.9584548109119737, 2.250047331442289966, -9.733932798157443500 ) ) ;
#41945 = CARTESIAN_POINT ( 'NONE',  ( 113.7698838361194760, 0.1075849324168598464, -12.14321520033829849 ) ) ;
#41946 = CIRCLE ( 'NONE', #9205, 5.635000000000000675 ) ;
#41947 = CARTESIAN_POINT ( 'NONE',  ( 122.7801548109119665, -3.383040157471821630, -19.15922257007629170 ) ) ;
#41948 = VERTEX_POINT ( 'NONE', #8976 ) ;
#41949 = CARTESIAN_POINT ( 'NONE',  ( 118.3969758961590486, -2.263366209404196638, -18.10533625161307114 ) ) ;
#41950 = CARTESIAN_POINT ( 'NONE',  ( 118.2420214775786320, -6.222761293078241884, -8.102969835052219238 ) ) ;
#41951 = CARTESIAN_POINT ( 'NONE',  ( 85.75809888461174069, -18.45227461768569199, -4.893215200338314474 ) ) ;
#41952 = CARTESIAN_POINT ( 'NONE',  ( 60.51499503671957569, -14.57400245158741114, -18.15781989776658989 ) ) ;
#41953 = CARTESIAN_POINT ( 'NONE',  ( 85.83930302032702286, -9.140269361470597431, -14.14321520033831625 ) ) ;
#41954 = CARTESIAN_POINT ( 'NONE',  ( 111.4549108795247747, -1.325403438956436419, -16.93181055722141792 ) ) ;
#41955 = LINE ( 'NONE', #16899, #20622 ) ;
#41956 = ORIENTED_EDGE ( 'NONE', *, *, #30873, .F. ) ;
#41957 = CARTESIAN_POINT ( 'NONE',  ( 115.8595014775786609, -1.834011780172310813, -8.268836392978581529 ) ) ;
#41958 = CARTESIAN_POINT ( 'NONE',  ( 126.1837548109119496, 0.4262465694468514643, -12.03445270309931736 ) ) ;
#41959 = CARTESIAN_POINT ( 'NONE',  ( 122.3263414775786373, -6.344957434206665248, -7.627207830600338134 ) ) ;
#41960 = CARTESIAN_POINT ( 'NONE',  ( 116.0296814775786345, -1.833838273342658809, -17.42832698103878286 ) ) ;
#41961 = DIRECTION ( 'NONE',  ( 0.000000000000000000, -0.3818493186865936084, 0.9242245927363024194 ) ) ;
#41962 = CARTESIAN_POINT ( 'NONE',  ( 117.6747548109119919, -1.834011780172310813, -8.268836392978581529 ) ) ;
#41963 = LINE ( 'NONE', #13706, #32957 ) ;
#41964 = FACE_OUTER_BOUND ( 'NONE', #27238, .T. ) ;
#41965 = CYLINDRICAL_SURFACE ( 'NONE', #32474, 3.000000000000003997 ) ;
#41966 = CARTESIAN_POINT ( 'NONE',  ( 123.9146881442452894, -10.15424416112533912, -14.75197769757731336 ) ) ;
#41967 = ORIENTED_EDGE ( 'NONE', *, *, #35055, .T. ) ;
#41968 = CIRCLE ( 'NONE', #41265, 6.479565957685751165 ) ;
#41969 = CARTESIAN_POINT ( 'NONE',  ( 94.20708369096698220, -24.88943055980569241, -13.49371108670732333 ) ) ;
#41970 = CARTESIAN_POINT ( 'NONE',  ( 117.7314814775786260, -4.089484607189486809, -7.948022111789456723 ) ) ;
#41971 = CARTESIAN_POINT ( 'NONE',  ( 123.9146881442452894, -10.15424416112533912, -14.75197769757731336 ) ) ;
#41972 = ORIENTED_EDGE ( 'NONE', *, *, #12819, .F. ) ;
#41973 = PRODUCT_DEFINITION_SHAPE ( 'NONE', 'NONE',  #33583 ) ;
#41974 = CARTESIAN_POINT ( 'NONE',  ( 135.8497638153261278, 0.6772939217498697984, -11.19057417008355770 ) ) ;
#41975 = CARTESIAN_POINT ( 'NONE',  ( 122.3830681442452857, -8.166667518702819706, -8.995218007635861213 ) ) ;
#41976 = CARTESIAN_POINT ( 'NONE',  ( 107.5655358795247736, -0.7896495226426338832, -17.46756447353520159 ) ) ;
#41977 = CARTESIAN_POINT ( 'NONE',  ( 121.5888948109119809, 0.1319031606808879209, -14.10382304977623669 ) ) ;
#41978 = ORIENTED_EDGE ( 'NONE', *, *, #9793, .T. ) ;
#41979 = EDGE_LOOP ( 'NONE', ( #37815, #10132, #39719, #18010, #6463 ) ) ;
#41980 = CARTESIAN_POINT ( 'NONE',  ( 112.9664414775786412, 0.5811942927096154232, -14.16772938898807155 ) ) ;
#41981 = CARTESIAN_POINT ( 'NONE',  ( 124.2550481442452792, -0.1624402480850797581, -16.17319339645315424 ) ) ;
#41982 = CARTESIAN_POINT ( 'NONE',  ( 120.3976348109119812, -1.834011780172310591, -8.268836392978581529 ) ) ;
#41983 = DIRECTION ( 'NONE',  ( -0.9908103287288503314, 0.1352586133457956419, 0.000000000000000000 ) ) ;
#41984 = CARTESIAN_POINT ( 'NONE',  ( 125.3328548109119964, -9.261995988541697145, -16.69588392320189030 ) ) ;
#41985 = CIRCLE ( 'NONE', #39046, 4.000000000000000888 ) ;
#41986 = CARTESIAN_POINT ( 'NONE',  ( 119.7434548109119703, -4.863998795839242995, -13.39321520033831447 ) ) ;
#41987 = CARTESIAN_POINT ( 'NONE',  ( 87.80477198183443477, -26.75858941326842810, -11.54476601486570964 ) ) ;
#41988 = CARTESIAN_POINT ( 'NONE',  ( 124.7088614775786226, 0.2603800115204892296, -16.42320221600525088 ) ) ;
#41990 = CARTESIAN_POINT ( 'NONE',  ( 125.1626748109119802, -0.1624402480850797581, -16.17319339645315424 ) ) ;
#41989 = CARTESIAN_POINT ( 'NONE',  ( 121.0216281442452981, -1.561330072975668948, -17.79121239304076951 ) ) ;
#41991 = CARTESIAN_POINT ( 'NONE',  ( 121.1918081442452859, -10.15424416112533912, -14.75197769757731336 ) ) ;
#41992 = CARTESIAN_POINT ( 'NONE',  ( 125.8328548109119964, -8.862178061931773598, -16.39564131203328401 ) ) ;
#41993 = CARTESIAN_POINT ( 'NONE',  ( 115.1220548109119761, -8.166667518702817929, -8.995218007635861213 ) ) ;
#41994 = ADVANCED_FACE ( 'NONE', ( #36546 ), #22874, .T. ) ;
#41995 = ORIENTED_EDGE ( 'NONE', *, *, #3802, .F. ) ;
#41996 = CIRCLE ( 'NONE', #10684, 20.00000000000000355 ) ;
#41997 = CARTESIAN_POINT ( 'NONE',  ( 124.8790414775786388, -8.899110576539117190, -16.42337572283568647 ) ) ;
#41998 = CARTESIAN_POINT ( 'NONE',  ( 114.1635827545248389, -6.936859964151250502, -8.388885654883777576 ) ) ;
#41999 = CARTESIAN_POINT ( 'NONE',  ( 107.6349890045248401, -9.868328341294098749, -11.32035403202665869 ) ) ;
#42000 = CARTESIAN_POINT ( 'NONE',  ( 113.3995983795247895, -8.402594152722688392, -16.93181055722141792 ) ) ;
#42001 = CARTESIAN_POINT ( 'NONE',  ( 124.3117748109119844, -10.30919188438810075, -12.61870101168855918 ) ) ;
#42002 = CARTESIAN_POINT ( 'NONE',  ( 126.1837548109119496, 0.4262465694468514643, -12.03445270309931736 ) ) ;
#42003 = EDGE_LOOP ( 'NONE', ( #41601, #19302, #38074, #34334, #11009 ) ) ;
#42004 = CARTESIAN_POINT ( 'NONE',  ( 114.6682414775786469, -7.894159318335828068, -9.358103419637847864 ) ) ;
#42005 = CARTESIAN_POINT ( 'NONE',  ( 109.7185827545247889, -2.477300249445798297, -19.15521520033831138 ) ) ;
#42006 = DIRECTION ( 'NONE',  ( -1.000000000000000000, -1.671245155169139691E-16, 0.000000000000000000 ) ) ;
#42007 = CARTESIAN_POINT ( 'NONE',  ( 124.3117748109119844, -10.30919188438810075, -12.61870101168855918 ) ) ;
#42008 = CARTESIAN_POINT ( 'NONE',  ( 124.0848681442452772, -4.089484607189486809, -7.948022111789456723 ) ) ;
#42009 = CARTESIAN_POINT ( 'NONE',  ( 62.83933201006748703, -13.37155033267121595, -18.76174004378365012 ) ) ;
#42010 = CARTESIAN_POINT ( 'NONE',  ( 112.3991748109119868, -8.166667518702817929, -8.995218007635859436 ) ) ;
#42011 = CARTESIAN_POINT ( 'NONE',  ( 105.6208483795248299, -0.7896495226426338832, -9.318865927141430916 ) ) ;
#42012 = ORIENTED_EDGE ( 'NONE', *, *, #16982, .F. ) ;
#42013 = FACE_OUTER_BOUND ( 'NONE', #11917, .T. ) ;
#42014 = CARTESIAN_POINT ( 'NONE',  ( 116.5969481442453031, -9.859900752359374465, -12.68260735090039404 ) ) ;
#42015 = CARTESIAN_POINT ( 'NONE',  ( 113.8740681442453138, 0.5811942927096154232, -14.16772938898807155 ) ) ;
#42016 = CARTESIAN_POINT ( 'NONE',  ( 115.4831921295247952, 0.8980012041604618078, -13.39321520033831447 ) ) ;
#42017 = CARTESIAN_POINT ( 'NONE',  ( 107.8433483795247838, -8.402594152722688392, -16.93181055722141792 ) ) ;
#42018 = CARTESIAN_POINT ( 'NONE',  ( 121.7023481442452777, -0.8288870151387760510, -10.36305467784173118 ) ) ;
#42019 = UNCERTAINTY_MEASURE_WITH_UNIT (LENGTH_MEASURE( 1.000000000000000082E-05 ), #14534, 'distance_accuracy_value', 'NONE');
#42020 = CARTESIAN_POINT ( 'NONE',  ( 119.2631014775786298, -9.565557343593413364, -10.61323700422348004 ) ) ;
#42021 = CARTESIAN_POINT ( 'NONE',  ( 111.6050014775786536, 0.1319031606808879209, -14.10382304977623669 ) ) ;
#42022 = ORIENTED_EDGE ( 'NONE', *, *, #33091, .T. ) ;
#42023 = ADVANCED_FACE ( 'NONE', ( #36319 ), #5089, .F. ) ;
#42024 = AXIS2_PLACEMENT_3D ( 'NONE', #44709, #18396, #42564 ) ;
#42025 = CARTESIAN_POINT ( 'NONE',  ( 121.4797829359119987, -5.367793381288652910, -18.78638297431638904 ) ) ;
#42026 = DIRECTION ( 'NONE',  ( -0.7962509850245453880, -0.6049664196031389052, 0.000000000000000000 ) ) ;
#42027 = CARTESIAN_POINT ( 'NONE',  ( 115.3489614775786407, -0.8288870151387760510, -10.36305467784173118 ) ) ;
#42028 = ORIENTED_EDGE ( 'NONE', *, *, #31744, .F. ) ;
#42029 = CARTESIAN_POINT ( 'NONE',  ( 96.54708369096698561, -24.20446030063578391, -12.09626349990295147 ) ) ;
#42030 = EDGE_CURVE ( 'NONE', #15033, #6780, #12097, .T. ) ;
#42031 = CARTESIAN_POINT ( 'NONE',  ( 112.2289948109119848, -1.834011780172310813, -8.268836392978581529 ) ) ;
#42032 = COLOUR_RGB ( '',0.7921568627450980005, 0.8196078431372548767, 0.9333333333333333481 ) ;
#42033 = ADVANCED_FACE ( 'NONE', ( #29493 ), #3377, .T. ) ;
#42034 = CARTESIAN_POINT ( 'NONE',  ( 109.2324108795247923, -1.325403438956436419, -16.93181055722141792 ) ) ;
#42035 = ORIENTED_EDGE ( 'NONE', *, *, #21963, .T. ) ;
#42036 = CARTESIAN_POINT ( 'NONE',  ( 119.2631014775786298, -9.565557343593413364, -10.61323700422348004 ) ) ;
#42037 = CARTESIAN_POINT ( 'NONE',  ( 114.3846081442453197, 0.4262465694468514643, -12.03445270309931736 ) ) ;
#42038 = FACE_OUTER_BOUND ( 'NONE', #37576, .T. ) ;
#42039 = CARTESIAN_POINT ( 'NONE',  ( 124.1884548109119777, -7.554583864224885481, -18.48844787311982785 ) ) ;
#42040 = ORIENTED_EDGE ( 'NONE', *, *, #39061, .F. ) ;
#42041 = CARTESIAN_POINT ( 'NONE',  ( 86.48169505875749508, -25.99489077589524300, -13.39321520033831625 ) ) ;
#42042 = CARTESIAN_POINT ( 'NONE',  ( 119.7434548109119703, -2.527210466738042172, -8.967976844669124148 ) ) ;
#42043 = CARTESIAN_POINT ( 'NONE',  ( 114.7886608795247696, -8.938348069036489818, -9.318865927141430916 ) ) ;
#42044 = CIRCLE ( 'NONE', #11456, 2.000000000000000444 ) ;
#42045 = CARTESIAN_POINT ( 'NONE',  ( 114.2711548109119803, -9.988377603198976828, -10.36322818467138340 ) ) ;
#42046 = EDGE_CURVE ( 'NONE', #39949, #166, #26075, .T. ) ;
#42047 = CARTESIAN_POINT ( 'NONE',  ( 122.2128881442453263, -7.643976991954077427, -18.09477374809248928 ) ) ;
#42048 = CARTESIAN_POINT ( 'NONE',  ( 119.4900081442453086, -7.643976991954077427, -18.09477374809248928 ) ) ;
#42049 = CARTESIAN_POINT ( 'NONE',  ( 113.7038881442453260, -6.222761293078232114, -8.102969835052212133 ) ) ;
#42050 = ADVANCED_FACE ( 'NONE', ( #31068 ), #34475, .T. ) ;
#42051 = EDGE_CURVE ( 'NONE', #32220, #45010, #13082, .T. ) ;
#42052 = ORIENTED_EDGE ( 'NONE', *, *, #17527, .T. ) ;
#42053 = CARTESIAN_POINT ( 'NONE',  ( 117.2776681442452968, -4.153390946401321671, -8.397313243818183892 ) ) ;
#42054 = CARTESIAN_POINT ( 'NONE',  ( 119.7434548109119561, -1.948846192371206598, -9.275183199048456117 ) ) ;
#42055 = CARTESIAN_POINT ( 'NONE',  ( 84.70844274511026128, -29.45715287386303061, -10.31656915580773948 ) ) ;
#42056 = CARTESIAN_POINT ( 'NONE',  ( 116.5760198611596081, -1.036737761566197014, -17.24079555149560861 ) ) ;
#42057 = CARTESIAN_POINT ( 'NONE',  ( 114.4980614775786592, -7.893985811506177619, -18.51759400769804742 ) ) ;
#42058 = ORIENTED_EDGE ( 'NONE', *, *, #33820, .T. ) ;
#42059 = CARTESIAN_POINT ( 'NONE',  ( 116.3133148109119759, -7.893985811506177619, -18.51759400769804742 ) ) ;
#42060 = DIRECTION ( 'NONE',  ( 0.000000000000000000, 1.000000000000000000, 0.000000000000000000 ) ) ;
#42061 = CARTESIAN_POINT ( 'NONE',  ( 109.8574890045247940, 0.8980012041604421569, -15.77991374673208469 ) ) ;
#42062 = CARTESIAN_POINT ( 'NONE',  ( 114.4980614775786592, -7.893985811506177619, -18.51759400769804742 ) ) ;
#42063 = CARTESIAN_POINT ( 'NONE',  ( 113.1366214775786432, -1.834011780172310813, -8.268836392978581529 ) ) ;
#42064 = VECTOR ( 'NONE', #16996, 1000.000000000000000 ) ;
#42065 = CARTESIAN_POINT ( 'NONE',  ( 124.0848681442452772, -5.574606645277164318, -18.38911715685844683 ) ) ;
#42066 = CARTESIAN_POINT ( 'NONE',  ( 63.92618626571611173, -15.01321783771253138, -16.50148821192263426 ) ) ;
#42067 = CARTESIAN_POINT ( 'NONE',  ( 108.1211608795247798, -1.325403438956436419, -16.93181055722141792 ) ) ;
#42068 = ORIENTED_EDGE ( 'NONE', *, *, #7164, .T. ) ;
#42069 = CARTESIAN_POINT ( 'NONE',  ( 120.5495288976800055, -1.244021962887374544, -16.96476564598603076 ) ) ;
#42070 = CARTESIAN_POINT ( 'NONE',  ( 109.2294421270962914, -8.142351692595484636, -17.62070062977968021 ) ) ;
#42071 = CARTESIAN_POINT ( 'NONE',  ( 117.2776681442452968, -4.153390946401321671, -8.397313243818183892 ) ) ;
#42072 = CARTESIAN_POINT ( 'NONE',  ( 107.3571765045248299, -7.250697342233347165, -19.15521520033831138 ) ) ;
#42073 = CARTESIAN_POINT ( 'NONE',  ( 122.6995153496756501, -1.087735405160626723, -17.17288456429612964 ) ) ;
#42074 = CARTESIAN_POINT ( 'NONE',  ( 109.0935046295247872, -4.863998795839590272, -7.631215200338315796 ) ) ;
#42075 = CARTESIAN_POINT ( 'NONE',  ( 127.0264730702696028, -5.161070523558970891, -7.997376402438204579 ) ) ;
#42076 = CARTESIAN_POINT ( 'NONE',  ( 126.1270281442452870, -10.30919188438810075, -12.61870101168855918 ) ) ;
#42077 = DIRECTION ( 'NONE',  ( 0.000000000000000000, 0.000000000000000000, -1.000000000000000000 ) ) ;
#42078 = CARTESIAN_POINT ( 'NONE',  ( 125.2761281442453054, -10.63000616557722466, -14.87417383870573495 ) ) ;
#42079 = CARTESIAN_POINT ( 'NONE',  ( 114.8384214775786489, 0.9020085738987339008, -11.91225656197089222 ) ) ;
#42080 = ORIENTED_EDGE ( 'NONE', *, *, #16655, .T. ) ;
#42081 = CARTESIAN_POINT ( 'NONE',  ( 114.7249681442453237, -9.565557343593413364, -10.61323700422348004 ) ) ;
#42082 = DIRECTION ( 'NONE',  ( 0.000000000000000000, 0.3818493186865927203, -0.9242245927363029745 ) ) ;
#42083 = CARTESIAN_POINT ( 'NONE',  ( 119.2063748109119814, -1.561330072975668504, -17.79121239304076951 ) ) ;
#42084 = CARTESIAN_POINT ( 'NONE',  ( 115.9729548109119861, -3.505236298600246325, -18.68346056562440793 ) ) ;
#42085 = ORIENTED_EDGE ( 'NONE', *, *, #22951, .F. ) ;
#42086 = CARTESIAN_POINT ( 'NONE',  ( 123.0637881442452937, -8.899110576539710493, -16.42337572283490132 ) ) ;
#42087 = EDGE_CURVE ( 'NONE', #4906, #14703, #41254, .T. ) ;
#42088 = CARTESIAN_POINT ( 'NONE',  ( 115.1787814775786387, -9.988377603198976828, -10.36322818467138340 ) ) ;
#42089 = DIRECTION ( 'NONE',  ( -0.000000000000000000, -0.9284778069183721172, -0.3713878862591650232 ) ) ;
#42090 = CARTESIAN_POINT ( 'NONE',  ( 108.1211608795247798, -8.938348069036489818, -9.318865927141430916 ) ) ;
#42091 = DIRECTION ( 'NONE',  ( 1.000000000000000000, 0.000000000000000000, -0.000000000000000000 ) ) ;
#42092 = CARTESIAN_POINT ( 'NONE',  ( 126.8316248077902486, 0.4396069532502042687, -13.21529045708529182 ) ) ;
#42093 = LINE ( 'NONE', #10632, #13160 ) ;
#42094 = CARTESIAN_POINT ( 'NONE',  ( 113.8173414775786512, 0.2603800115204892296, -16.42320221600525088 ) ) ;
#42095 = CARTESIAN_POINT ( 'NONE',  ( 136.2267163768109981, -10.68226541249164896, -14.07034713969670747 ) ) ;
#42096 = CARTESIAN_POINT ( 'NONE',  ( 71.99789814782840836, -24.87091310681484657, -7.393215200338315363 ) ) ;
#42097 = CARTESIAN_POINT ( 'NONE',  ( 111.0762212410415799, 0.7607806665037644134, -12.14321520033829316 ) ) ;
#42098 = EDGE_CURVE ( 'NONE', #19823, #33002, #14311, .T. ) ;
#42099 = CARTESIAN_POINT ( 'NONE',  ( -12.36826994950264336, -4.374949827406453551, -7.393215200338315363 ) ) ;
#42100 = CARTESIAN_POINT ( 'NONE',  ( 113.6774108795247997, -1.325403438956436419, -16.93181055722141792 ) ) ;
#42101 = CARTESIAN_POINT ( 'NONE',  ( 112.4559014775786778, -0.1624402480850797581, -16.17319339645315424 ) ) ;
#42102 = CARTESIAN_POINT ( 'NONE',  ( 125.4584548109119737, -9.675291321254654520, -19.78473021908636298 ) ) ;
#42103 = CARTESIAN_POINT ( 'NONE',  ( 111.6669404873412077, -2.348512537728060234, -17.99195118506215962 ) ) ;
#42105 = CARTESIAN_POINT ( 'NONE',  ( 116.5969481442453031, 0.5811942927096154232, -14.16772938898807155 ) ) ;
#42104 = DIRECTION ( 'NONE',  ( 1.000000000000000000, 0.000000000000000000, 0.000000000000000000 ) ) ;
#42106 = AXIS2_PLACEMENT_3D ( 'NONE', #23267, #45145, #27368 ) ;
#42107 = B_SPLINE_CURVE_WITH_KNOTS ( 'NONE', 3,
 ( #36355, #22015, #18596, #40016, #32708, #29079, #8781, #26339, #22235, #4901 ),
 .UNSPECIFIED., .F., .F.,
 ( 4, 3, 3, 4 ),
 ( 2.453269466693399854E-18, 0.0001671877548681249956, 0.0003343755096277640170, 0.0006463528481650609656 ),
 .UNSPECIFIED. ) ;
#42108 = CARTESIAN_POINT ( 'NONE',  ( 90.99708770779186295, -25.99489077589524300, -13.39321520033831447 ) ) ;
#42109 = CARTESIAN_POINT ( 'NONE',  ( 119.3765548109119834, -10.15424416112533912, -14.75197769757731336 ) ) ;
#42110 = EDGE_LOOP ( 'NONE', ( #20101, #8235, #40865, #29629, #9653, #41421, #1195, #43454 ) ) ;
#42111 = CARTESIAN_POINT ( 'NONE',  ( 122.4767535264548854, -8.247323210606174015, -17.08054893949881858 ) ) ;
#42112 = EDGE_CURVE ( 'NONE', #36351, #10961, #39781, .T. ) ;
#42113 = CARTESIAN_POINT ( 'NONE',  ( 124.5386814775786206, -5.638512984488999180, -18.83840828888717311 ) ) ;
#42114 = CARTESIAN_POINT ( 'NONE',  ( 115.6915515045247531, -6.936859964151250502, -18.39754474579286025 ) ) ;
#42115 = CARTESIAN_POINT ( 'NONE',  ( 115.0653281442453277, -3.505236298600246325, -18.68346056562440793 ) ) ;
#42116 = CARTESIAN_POINT ( 'NONE',  ( 111.9453614775786434, -7.894159318335828068, -9.358103419637847864 ) ) ;
#42117 = CARTESIAN_POINT ( 'NONE',  ( 85.96066202508467313, -27.32956148653828876, -8.622328686912057449 ) ) ;
#42118 = CARTESIAN_POINT ( 'NONE',  ( 112.3578015045248861, -2.477300249445798297, -7.631215200338321125 ) ) ;
#42119 = CARTESIAN_POINT ( 'NONE',  ( 120.7379948109119709, 0.4262465694468514643, -12.03445270309931736 ) ) ;
#42120 = CARTESIAN_POINT ( 'NONE',  ( 118.8092881442453290, -0.1624402480850797581, -16.17319339645315424 ) ) ;
#42121 = CARTESIAN_POINT ( 'NONE',  ( 116.7671281442453193, -7.643976991954101408, -18.09477374809246797 ) ) ;
#42122 = CARTESIAN_POINT ( 'NONE',  ( 109.2294439528113230, -3.574589291641149025, -8.025114565246834530 ) ) ;
#42123 = DIRECTION ( 'NONE',  ( -0.9908103287288505534, 0.1352586133457944206, 0.000000000000000000 ) ) ;
#42124 = CARTESIAN_POINT ( 'NONE',  ( 110.0658483795247804, -8.402594152722688392, -16.93181055722141792 ) ) ;
#42125 = CARTESIAN_POINT ( 'NONE',  ( 85.70478001548416103, -25.99489077589524300, -13.39321520033831447 ) ) ;
#42126 = CARTESIAN_POINT ( 'NONE',  ( 115.9162281442453235, -4.089484607189486809, -7.948022111789456723 ) ) ;
#42127 = CARTESIAN_POINT ( 'NONE',  ( 115.8027748109119841, -0.4660016031367893996, -10.09054647747474043 ) ) ;
#42128 = CARTESIAN_POINT ( 'NONE',  ( 111.3854577545248645, -7.250697342233347165, -7.631215200338321125 ) ) ;
#42129 = CARTESIAN_POINT ( 'NONE',  ( 114.4980614775786592, -7.893985811506177619, -18.51759400769804742 ) ) ;
#42130 = ORIENTED_EDGE ( 'NONE', *, *, #13644, .T. ) ;
#42131 = CARTESIAN_POINT ( 'NONE',  ( 113.3277860444392076, -1.267766418764742165, -16.93314635290707315 ) ) ;
#42132 = CARTESIAN_POINT ( 'NONE',  ( 121.4754414775786131, -8.166667518702819706, -8.995218007635861213 ) ) ;
#42133 = CARTESIAN_POINT ( 'NONE',  ( 115.8595014775786609, -1.834011780172310813, -8.268836392978581529 ) ) ;
#42134 = CARTESIAN_POINT ( 'NONE',  ( 121.7023481442452919, -0.8288870151387760510, -10.36305467784173118 ) ) ;
#42135 = SURFACE_SIDE_STYLE ('',( #10454 ) ) ;
#42136 = CARTESIAN_POINT ( 'NONE',  ( 111.6050014775786536, 0.1319031606808879209, -14.10382304977623669 ) ) ;
#42137 = CARTESIAN_POINT ( 'NONE',  ( 123.0637881442452937, -0.4660016031367893996, -10.09054647747474043 ) ) ;
#42138 = CARTESIAN_POINT ( 'NONE',  ( 114.3719421295247827, 0.8980012041604618078, -13.39321520033831447 ) ) ;
#42139 = AXIS2_PLACEMENT_3D ( 'NONE', #37577, #2917, #16618 ) ;
#42140 = CARTESIAN_POINT ( 'NONE',  ( 116.1431348109119881, 0.1319031606808879209, -14.10382304977623669 ) ) ;
#42141 = DIRECTION ( 'NONE',  ( 1.000000000000000000, 0.000000000000000000, -0.000000000000000000 ) ) ;
#42142 = VERTEX_POINT ( 'NONE', #20599 ) ;
#42143 = CARTESIAN_POINT ( 'NONE',  ( 122.8936081442453059, 0.2603800115204892296, -16.42320221600525088 ) ) ;
#42144 = ADVANCED_FACE ( 'NONE', ( #34905 ), #20154, .F. ) ;
#42145 = DIRECTION ( 'NONE',  ( 0.9908103287288505534, -0.1352586133457944206, 0.000000000000000000 ) ) ;
#42146 = CARTESIAN_POINT ( 'NONE',  ( 119.2063748109119814, -1.561330072975668504, -17.79121239304076951 ) ) ;
#42147 = EDGE_LOOP ( 'NONE', ( #22046, #4327, #19402, #11315, #2456 ) ) ;
#42148 = CARTESIAN_POINT ( 'NONE',  ( 116.3166296295247832, -4.863998795839590272, -19.15521520033831493 ) ) ;
#42149 = CARTESIAN_POINT ( 'NONE',  ( 125.2761281442453054, -10.63000616557722466, -14.87417383870573495 ) ) ;
#42150 = CARTESIAN_POINT ( 'NONE',  ( 60.53937939559665438, -4.256997083809236138, -7.393215200338315363 ) ) ;
#42151 = CARTESIAN_POINT ( 'NONE',  ( 115.5758681442453053, -7.894159318335828068, -9.358103419637847864 ) ) ;
#42152 = CARTESIAN_POINT ( 'NONE',  ( 124.1916298109119765, -2.529232162390850913, -8.971805383624186447 ) ) ;
#42153 =( BOUNDED_SURFACE ( )  B_SPLINE_SURFACE ( 3, 2, ( 
 ( #5148, #11782, #15877 ),
 ( #18402, #11331, #29774 ),
 ( #32511, #40036, #32730 ),
 ( #25689, #4481, #39140 ),
 ( #22706, #43013, #8357 ),
 ( #19065, #22261, #42799 ),
 ( #15198, #32949, #1059 ),
 ( #39596, #22483, #32294 ),
 ( #1286, #1726, #12009 ),
 ( #14974, #8138, #4924 ),
 ( #18838, #15648, #1504 ),
 ( #29552, #11560, #22039 ),
 ( #15424, #25911, #25242 ),
 ( #5379, #7905, #26132 ) ),
 .UNSPECIFIED., .F., .F., .F. ) 
 B_SPLINE_SURFACE_WITH_KNOTS ( ( 4, 2, 2, 2, 2, 2, 4 ),
 ( 3, 3 ),
 ( 2.482289681851995056, 3.039814506485170043, 3.318576918801754871, 3.597339331118345029, 3.876101743434930302, 4.154864155751514687, 4.712388980384689674 ),
 ( 0.000000000000000000, 1.000000000000000000 ),
 .UNSPECIFIED. ) 
 GEOMETRIC_REPRESENTATION_ITEM ( )  RATIONAL_B_SPLINE_SURFACE ( (
 ( 1.000000000000000000, 0.6031903678053659457, 1.000000000000000000),
 ( 1.000000000000000000, 0.5868400859402069791, 1.000000000000000000),
 ( 1.000000000000000000, 0.5760967621943400285, 1.000000000000000000),
 ( 1.000000000000000000, 0.5718412329145610151, 1.000000000000000000),
 ( 1.000000000000000000, 0.5723757457118600067, 1.000000000000000000),
 ( 1.000000000000000000, 0.5772784653944200706, 1.000000000000000000),
 ( 1.000000000000000000, 0.5816430333813810138, 1.000000000000000000),
 ( 1.000000000000000000, 0.5936320506908580041, 1.000000000000000000),
 ( 1.000000000000000000, 0.6012496247163490182, 1.000000000000000000),
 ( 1.000000000000000000, 0.6188356767525979851, 1.000000000000000000),
 ( 1.000000000000000000, 0.6287978291299359812, 1.000000000000000000),
 ( 1.000000000000000000, 0.6606618940965899300, 1.000000000000000000),
 ( 1.000000000000000000, 0.6844987252709670011, 1.000000000000000000),
 ( 1.000000000000000000, 0.7071067811865470176, 1.000000000000000000) ) ) 
 REPRESENTATION_ITEM ( '' )  SURFACE ( )  );
#42154 = CARTESIAN_POINT ( 'NONE',  ( 121.5321681442453183, -0.1624402480850797581, -16.17319339645315424 ) ) ;
#42155 = DIRECTION ( 'NONE',  ( 1.000000000000000000, 0.000000000000000000, -0.000000000000000000 ) ) ;
#42156 = CARTESIAN_POINT ( 'NONE',  ( 120.4543614775786295, -5.574606645277164318, -18.38911715685844683 ) ) ;
#42157 = CARTESIAN_POINT ( 'NONE',  ( 125.0480389746926306, -10.95843241427508730, -8.969000644412037815 ) ) ;
#42158 = CARTESIAN_POINT ( 'NONE',  ( 120.2841814775786276, -10.15424416112533912, -14.75197769757731336 ) ) ;
#42159 = DIRECTION ( 'NONE',  ( 1.000000000000000000, 0.000000000000000000, -0.000000000000000000 ) ) ;
#42160 = CARTESIAN_POINT ( 'NONE',  ( 116.8238548109119819, -4.089484607189486809, -7.948022111789456723 ) ) ;
#42161 = CARTESIAN_POINT ( 'NONE',  ( 90.04708369096697140, -25.99489077589524300, -13.39321520033831447 ) ) ;
#42162 = CARTESIAN_POINT ( 'NONE',  ( 119.3198281442452924, -9.859900752359374465, -12.68260735090039404 ) ) ;
#42163 = ORIENTED_EDGE ( 'NONE', *, *, #7558, .F. ) ;
#42164 = CARTESIAN_POINT ( 'NONE',  ( 116.1431348109119881, -10.30919188438810075, -12.61870101168855918 ) ) ;
#42165 = CARTESIAN_POINT ( 'NONE',  ( 113.6774108795247997, -1.325403438956436419, -16.93181055722141792 ) ) ;
#42166 = LINE ( 'NONE', #35752, #31373 ) ;
#42167 = DIRECTION ( 'NONE',  ( -0.000000000000000000, -0.9284778069183721172, -0.3713878862591650232 ) ) ;
#42168 = AXIS2_PLACEMENT_3D ( 'NONE', #1293, #5155, #15205 ) ;
#42169 = CARTESIAN_POINT ( 'NONE',  ( 70.19189222814998175, -57.98054017398621340, -36.39502311309316696 ) ) ;
#42170 = CARTESIAN_POINT ( 'NONE',  ( 124.1415948109119540, -6.344957434206665248, -7.627207830600338134 ) ) ;
#42171 = VERTEX_POINT ( 'NONE', #23576 ) ;
#42172 = CARTESIAN_POINT ( 'NONE',  ( 127.3669547543381526, -9.122482256072121487, -9.796118959629435352 ) ) ;
#42173 = CARTESIAN_POINT ( 'NONE',  ( 120.6812681442452941, 0.1319031606808879209, -14.10382304977623669 ) ) ;
#42174 = CARTESIAN_POINT ( 'NONE',  ( 116.3133148109119759, -7.893985811506194494, -18.51759400769804031 ) ) ;
#42175 = CARTESIAN_POINT ( 'NONE',  ( 64.85962650386538542, -13.90972770790538071, -17.69353582949934278 ) ) ;
#42176 = DIRECTION ( 'NONE',  ( 0.000000000000000000, 1.000000000000000000, 0.000000000000000000 ) ) ;
#42177 = CARTESIAN_POINT ( 'NONE',  ( 110.1353015045248469, -6.936859964151250502, -18.39754474579286025 ) ) ;
#42178 = DIRECTION ( 'NONE',  ( 0.000000000000000000, 0.000000000000000000, -1.000000000000000000 ) ) ;
#42179 = ORIENTED_EDGE ( 'NONE', *, *, #401, .F. ) ;
#42180 = CARTESIAN_POINT ( 'NONE',  ( 115.2922348109119781, -10.63000616557722466, -14.87417383870573495 ) ) ;
#42181 = CARTESIAN_POINT ( 'NONE',  ( 124.4252281442452812, -0.8288870151387760510, -10.36305467784173118 ) ) ;
#42182 = CARTESIAN_POINT ( 'NONE',  ( 123.2906948109119867, -8.166667518702819706, -8.995218007635861213 ) ) ;
#42183 = CARTESIAN_POINT ( 'NONE',  ( 116.5402214775786405, -9.565557343593413364, -10.61323700422348004 ) ) ;
#42184 = CARTESIAN_POINT ( 'NONE',  ( 127.0150841466604277, -3.081832127571603408, -8.297561108701472676 ) ) ;
#42185 = CARTESIAN_POINT ( 'NONE',  ( 0.000000000000000000, 0.000000000000000000, 0.000000000000000000 ) ) ;
#42186 = CARTESIAN_POINT ( 'NONE',  ( 122.6099748109119929, -9.261995988541697145, -16.69588392320189030 ) ) ;
#42187 = DIRECTION ( 'NONE',  ( -0.2768435750659241079, -0.3568721902840695792, 0.8921882507333129819 ) ) ;
#42188 = DIRECTION ( 'NONE',  ( 0.000000000000000000, 0.000000000000000000, -1.000000000000000000 ) ) ;
#42189 = CARTESIAN_POINT ( 'NONE',  ( 110.5266510812576826, -0.01829820670803256055, -12.14321520033831625 ) ) ;
#42190 = CARTESIAN_POINT ( 'NONE',  ( 124.9357681442453014, -7.643976991954077427, -18.09477374809248928 ) ) ;
#42191 = VERTEX_POINT ( 'NONE', #2804 ) ;
#42192 = CARTESIAN_POINT ( 'NONE',  ( 70.19189222814998175, -52.40967333247598248, -34.16669579553818181 ) ) ;
#42193 = CARTESIAN_POINT ( 'NONE',  ( 119.6601881442453106, -8.166667518702819706, -8.995218007635861213 ) ) ;
#42194 = CARTESIAN_POINT ( 'NONE',  ( 124.9924948109119924, -5.574606645277164318, -18.38911715685844683 ) ) ;
#42195 = ORIENTED_EDGE ( 'NONE', *, *, #28095, .F. ) ;
#42196 = CARTESIAN_POINT ( 'NONE',  ( 136.8611794030201168, 0.2047575970914792265, -11.11870408231551899 ) ) ;
#42197 = CARTESIAN_POINT ( 'NONE',  ( 121.5321681442453183, -9.988377603198976828, -10.36322818467138340 ) ) ;
#42198 = CARTESIAN_POINT ( 'NONE',  ( 107.9822546295247889, -4.863998795839590272, -7.631215200338315796 ) ) ;
#42199 = CARTESIAN_POINT ( 'NONE',  ( 119.6601881442453106, -1.833838273342659253, -17.42832698103878286 ) ) ;
#42200 = VERTEX_POINT ( 'NONE', #9654 ) ;
#42201 = CARTESIAN_POINT ( 'NONE',  ( 115.4624148109119943, -5.638512984488999180, -18.83840828888717311 ) ) ;
#42202 = VECTOR ( 'NONE', #31045, 1000.000000000000000 ) ;
#42203 = CARTESIAN_POINT ( 'NONE',  ( 66.82415148905926117, -40.21211973637273474, -4.893215200338314474 ) ) ;
#42204 = CIRCLE ( 'NONE', #13089, 2.999999999999999556 ) ;
#42205 = CARTESIAN_POINT ( 'NONE',  ( 120.7947214775786193, -9.261995988541706026, -16.69588392320187964 ) ) ;
#42206 = CARTESIAN_POINT ( 'NONE',  ( 59.44377208703740223, -12.82110557137145967, -9.393546723914594665 ) ) ;
#42207 = CARTESIAN_POINT ( 'NONE',  ( 111.2646414775786496, -8.899110576539710493, -16.42337572283490132 ) ) ;
#42208 = DIRECTION ( 'NONE',  ( 0.000000000000000000, 0.000000000000000000, 1.000000000000000000 ) ) ;
#42209 = EDGE_CURVE ( 'NONE', #29623, #21444, #44893, .T. ) ;
#42210 = DIRECTION ( 'NONE',  ( 0.9609149988134837450, -0.1028163501681639419, 0.2570431154366518145 ) ) ;
#42211 = CARTESIAN_POINT ( 'NONE',  ( 122.6099748109119929, -9.261995988541697145, -16.69588392320189030 ) ) ;
#42213 = CARTESIAN_POINT ( 'NONE',  ( 123.5176014775786228, -0.8288870151387760510, -10.36305467784173118 ) ) ;
#42212 = CARTESIAN_POINT ( 'NONE',  ( 121.6456214775786293, -10.63000616557722466, -14.87417383870573495 ) ) ;
#42214 = CARTESIAN_POINT ( 'NONE',  ( 119.4332814775786318, -8.899110576539710493, -16.42337572283490132 ) ) ;
#42215 = DIRECTION ( 'NONE',  ( 0.000000000000000000, 0.000000000000000000, -1.000000000000000000 ) ) ;
#42216 = CARTESIAN_POINT ( 'NONE',  ( 116.6536748109119941, 0.9020085738987339008, -11.91225656197089222 ) ) ;
#42217 = EDGE_LOOP ( 'NONE', ( #33524, #40468, #14792, #35066, #2812 ) ) ;
#42218 = CARTESIAN_POINT ( 'NONE',  ( 69.69189222815028018, -41.76310523276638520, -10.89321520033831447 ) ) ;
#42219 = DIRECTION ( 'NONE',  ( -0.000000000000000000, -0.9284778069183718952, -0.3713878862591649677 ) ) ;
#42220 = CARTESIAN_POINT ( 'NONE',  ( 114.5108483795247878, -8.402594152722688392, -16.93181055722141792 ) ) ;
#42221 = CARTESIAN_POINT ( 'NONE',  ( 107.2877233795247776, -1.325403438956436419, -9.854619843455211026 ) ) ;
#42222 = CARTESIAN_POINT ( 'NONE',  ( 115.6220983795247861, -8.402594152722688392, -16.93181055722141792 ) ) ;
#42223 = CARTESIAN_POINT ( 'NONE',  ( 124.6521348109119884, -1.561330072975668948, -17.79121239304076951 ) ) ;
#42224 = CARTESIAN_POINT ( 'NONE',  ( 112.7962614775786676, -3.383040157471821630, -19.15922257007629170 ) ) ;
#42225 = VERTEX_POINT ( 'NONE', #3254 ) ;
#42226 = CARTESIAN_POINT ( 'NONE',  ( 113.6471614775786492, -4.153390946401321671, -8.397313243818183892 ) ) ;
#42227 = CARTESIAN_POINT ( 'NONE',  ( 111.4549108795247747, -8.938348069036489818, -9.318865927141430916 ) ) ;
#42228 = CARTESIAN_POINT ( 'NONE',  ( 121.9470836909669913, -24.14644159042263993, -12.62951656296512937 ) ) ;
#42229 = CARTESIAN_POINT ( 'NONE',  ( 123.7445081442452874, -1.561330072975668948, -17.79121239304076951 ) ) ;
#42230 = CARTESIAN_POINT ( 'NONE',  ( 124.3117748109119844, -10.30919188438810075, -12.61870101168855918 ) ) ;
#42231 = CARTESIAN_POINT ( 'NONE',  ( 79.23106798748115409, 4.957210186511446182, -6.038458229677214462 ) ) ;
#42232 = CARTESIAN_POINT ( 'NONE',  ( 114.6682414775786469, -1.561330072975668060, -17.79121239304076596 ) ) ;
#42233 = CARTESIAN_POINT ( 'NONE',  ( 114.7886608795247696, -8.938348069036489818, -9.318865927141430916 ) ) ;
#42234 = CARTESIAN_POINT ( 'NONE',  ( 111.5938171295247940, 0.1403307496149613920, -13.39321520033831447 ) ) ;
#42235 = VERTEX_POINT ( 'NONE', #17616 ) ;
#42236 = CARTESIAN_POINT ( 'NONE',  ( 126.4915402333594301, -7.429179904925708122, -8.943053816332739103 ) ) ;
#42237 = CARTESIAN_POINT ( 'NONE',  ( 114.0442481442453300, -7.643976991954077427, -18.09477374809248928 ) ) ;
#42238 = CARTESIAN_POINT ( 'NONE',  ( 112.9664414775786412, 0.5811942927096154232, -14.16772938898807155 ) ) ;
#42239 = CIRCLE ( 'NONE', #32026, 2.999999999999999556 ) ;
#42240 = CARTESIAN_POINT ( 'NONE',  ( 107.3571765045248299, -2.791137627527939813, -8.388885654883777576 ) ) ;
#42241 = DIRECTION ( 'NONE',  ( 0.000000000000000000, -0.9242245927363028635, -0.3818493186865930533 ) ) ;
#42242 = CARTESIAN_POINT ( 'NONE',  ( 121.1350814775786233, -9.859900752359378018, -12.68260735090039759 ) ) ;
#42243 = CARTESIAN_POINT ( 'NONE',  ( 112.9664414775786412, -9.859900752359374465, -12.68260735090039404 ) ) ;
#42244 = ORIENTED_EDGE ( 'NONE', *, *, #10043, .F. ) ;
#42245 = CARTESIAN_POINT ( 'NONE',  ( 120.7157985609119635, -0.08252387247370887580, -11.91645802438286417 ) ) ;
#42246 = AXIS2_PLACEMENT_3D ( 'NONE', #20924, #38020, #161 ) ;
#42247 = LINE ( 'NONE', #13982, #28813 ) ;
#42248 = CARTESIAN_POINT ( 'NONE',  ( 115.0653281442453277, -3.505236298600246325, -18.68346056562440793 ) ) ;
#42249 = ORIENTED_EDGE ( 'NONE', *, *, #238, .T. ) ;
#42250 = VECTOR ( 'NONE', #22409, 1000.000000000000000 ) ;
#42251 = CARTESIAN_POINT ( 'NONE',  ( 126.5621572004020408, -9.382143744326477020, -15.91102935692771680 ) ) ;
#42252 = CARTESIAN_POINT ( 'NONE',  ( 112.1722681442453222, -0.4660016031367893996, -10.09054647747474043 ) ) ;
#42253 = CARTESIAN_POINT ( 'NONE',  ( 108.6073327545248048, -6.936859964151250502, -8.388885654883777576 ) ) ;
#42254 = CARTESIAN_POINT ( 'NONE',  ( 125.3328548109119964, -0.8288870151387760510, -10.36305467784173118 ) ) ;
#42255 = ORIENTED_EDGE ( 'NONE', *, *, #14170, .T. ) ;
#42256 = CARTESIAN_POINT ( 'NONE',  ( 118.7525614775786380, -1.833838273342659253, -17.42832698103878286 ) ) ;
#42257 = CARTESIAN_POINT ( 'NONE',  ( 117.2209414775786485, -2.084020599724406786, -8.691656652584148546 ) ) ;
#42258 = DIRECTION ( 'NONE',  ( 0.9609149988134843001, -0.1028163501681632064, 0.2570431154366505933 ) ) ;
#42259 = CARTESIAN_POINT ( 'NONE',  ( 123.0077516859119839, -9.665098340737509730, -17.37397104707595474 ) ) ;
#42260 = ORIENTED_EDGE ( 'NONE', *, *, #782, .F. ) ;
#42261 = CARTESIAN_POINT ( 'NONE',  ( 72.54180985774836188, -57.87148204839928667, -35.62222722694667709 ) ) ;
#42262 = CARTESIAN_POINT ( 'NONE',  ( 92.26512299712632625, -23.76310523276723785, -20.89321520033831447 ) ) ;
#42263 = CARTESIAN_POINT ( 'NONE',  ( 109.2324108795247923, -8.938348069036489818, -9.318865927141430916 ) ) ;
#42264 = AXIS2_PLACEMENT_3D ( 'NONE', #30512, #19803, #40786 ) ;
#42265 = CARTESIAN_POINT ( 'NONE',  ( 114.0442481442453300, -1.834011780172310813, -8.268836392978581529 ) ) ;
#42266 = CARTESIAN_POINT ( 'NONE',  ( 112.2289948109119848, -1.834011780172310813, -8.268836392978581529 ) ) ;
#42267 = CARTESIAN_POINT ( 'NONE',  ( 118.0718414775786442, -0.8288870151387760510, -10.36305467784173118 ) ) ;
#42268 = CARTESIAN_POINT ( 'NONE',  ( 113.4202548109119846, 0.1319031606808870605, -14.10382304977625090 ) ) ;
#42269 = VERTEX_POINT ( 'NONE', #38345 ) ;
#42270 = CARTESIAN_POINT ( 'NONE',  ( 115.3489614775786407, -0.8288870151387760510, -10.36305467784173118 ) ) ;
#42271 = CARTESIAN_POINT ( 'NONE',  ( 70.19189222814998175, -100.0979043305785581, -53.24182196210380624 ) ) ;
#42272 = VECTOR ( 'NONE', #31122, 1000.000000000000000 ) ;
#42273 = CARTESIAN_POINT ( 'NONE',  ( 125.1613296207260078, -1.288565105604724703, -16.90544979172889484 ) ) ;
#42274 = CARTESIAN_POINT ( 'NONE',  ( 115.7610046295247912, -4.863998795839590272, -7.631215200338315796 ) ) ;
#42275 = CARTESIAN_POINT ( 'NONE',  ( 114.0442481442453300, -1.834011780172310813, -8.268836392978581529 ) ) ;
#42276 = ORIENTED_EDGE ( 'NONE', *, *, #43882, .T. ) ;
#42277 = CIRCLE ( 'NONE', #25516, 4.999999999999998224 ) ;
#42278 = CARTESIAN_POINT ( 'NONE',  ( 117.0507614775786465, -10.30919188438810075, -12.61870101168855918 ) ) ;
#42279 = CARTESIAN_POINT ( 'NONE',  ( 88.46631044337289040, -25.99489077589524300, -13.39321520033831625 ) ) ;
#42280 = CARTESIAN_POINT ( 'NONE',  ( 111.9410827545248708, -2.477300249445798297, -19.15521520033831138 ) ) ;
#42281 = CARTESIAN_POINT ( 'NONE',  ( 112.5126281442453120, -10.30919188438810075, -12.61870101168855918 ) ) ;
#42282 = CARTESIAN_POINT ( 'NONE',  ( 112.9664414775786412, 0.5811942927096154232, -14.16772938898807155 ) ) ;
#42283 = CARTESIAN_POINT ( 'NONE',  ( 126.5561942423865105, -10.03277835551166497, -13.35508656583795606 ) ) ;
#42284 = ADVANCED_FACE ( 'NONE', ( #16956 ), #27664, .T. ) ;
#42285 = DIRECTION ( 'NONE',  ( -0.000000000000000000, -0.9284778069183721172, -0.3713878862591650232 ) ) ;
#42286 = CARTESIAN_POINT ( 'NONE',  ( 109.1629577545248395, -2.791137627527939813, -18.39754474579286025 ) ) ;
#42287 = EDGE_LOOP ( 'NONE', ( #43425, #41075, #9504, #23680 ) ) ;
#42288 = CARTESIAN_POINT ( 'NONE',  ( 121.5428448253203015, -6.059724811980599313, -18.37735133589800540 ) ) ;
#42289 = CARTESIAN_POINT ( 'NONE',  ( 109.2294421421874375, -4.292925824281061509, -18.52829067132285346 ) ) ;
#42290 = CARTESIAN_POINT ( 'NONE',  ( 117.7314814775786260, -5.574606645277164318, -18.38911715685844683 ) ) ;
#42291 = CARTESIAN_POINT ( 'NONE',  ( 64.48003408175695483, -13.07484350022234132, -11.22706228626448421 ) ) ;
#42292 = CARTESIAN_POINT ( 'NONE',  ( 115.2053796295247849, -4.863998795839590272, -8.388885654883775800 ) ) ;
#42293 = CARTESIAN_POINT ( 'NONE',  ( 108.8156921295247912, 0.8980012041604618078, -13.39321520033831447 ) ) ;
#42294 = CARTESIAN_POINT ( 'NONE',  ( 126.2455040230451573, -4.383286045279406018, -8.401547924378691690 ) ) ;
#42295 = CARTESIAN_POINT ( 'NONE',  ( 124.5386814775786206, -5.638512984488999180, -18.83840828888717311 ) ) ;
#42296 = CARTESIAN_POINT ( 'NONE',  ( 119.8303681442452984, 0.4262465694468589028, -12.03445270309934578 ) ) ;
#42297 = CARTESIAN_POINT ( 'NONE',  ( 125.6732148109119862, 0.5811942927096110934, -14.16772938898807510 ) ) ;
#42298 = CARTESIAN_POINT ( 'NONE',  ( 116.5969481442453031, 0.5811942927096154232, -14.16772938898807155 ) ) ;
#42299 = ORIENTED_EDGE ( 'NONE', *, *, #36685, .F. ) ;
#42300 = CARTESIAN_POINT ( 'NONE',  ( 114.0442481442453300, -7.643976991954077427, -18.09477374809248928 ) ) ;
#42301 = CARTESIAN_POINT ( 'NONE',  ( 116.6536748109119941, 0.9020085738987339008, -11.91225656197089222 ) ) ;
#42302 = CARTESIAN_POINT ( 'NONE',  ( 114.4413348109119823, -0.8288870151387760510, -10.36305467784173118 ) ) ;
#42303 = ORIENTED_EDGE ( 'NONE', *, *, #21448, .T. ) ;
#42304 = EDGE_CURVE ( 'NONE', #7925, #43873, #34035, .T. ) ;
#42305 = CARTESIAN_POINT ( 'NONE',  ( 122.2696148109119889, -5.574606645277164318, -18.38911715685844683 ) ) ;
#42306 = EDGE_CURVE ( 'NONE', #30977, #6072, #15717, .T. ) ;
#42307 = EDGE_CURVE ( 'NONE', #28482, #43185, #7723, .T. ) ;
#42308 = VECTOR ( 'NONE', #30494, 1000.000000000000000 ) ;
#42309 = CARTESIAN_POINT ( 'NONE',  ( 118.4689281442453392, 0.9020085738987339008, -11.91225656197089222 ) ) ;
#42310 = CARTESIAN_POINT ( 'NONE',  ( 137.1522193784430499, 0.2019376872246030630, -15.10340397907687127 ) ) ;
#42311 = CARTESIAN_POINT ( 'NONE',  ( 107.7044421295247929, 0.8980012041604618078, -13.39321520033831447 ) ) ;
#42312 = CIRCLE ( 'NONE', #13193, 1.610000000000000986 ) ;
#42313 = CARTESIAN_POINT ( 'NONE',  ( 64.21381391893872603, -15.17632890891775510, -10.58270692696840598 ) ) ;
#42314 = CARTESIAN_POINT ( 'NONE',  ( 126.9164742704674609, 0.4800028309212418520, -13.16027790502670847 ) ) ;
#42315 = DIRECTION ( 'NONE',  ( -1.000000000000000000, 0.000000000000000000, -0.000000000000000000 ) ) ;
#42316 = CARTESIAN_POINT ( 'NONE',  ( 116.2565881442452991, -9.261995988541697145, -16.69588392320189030 ) ) ;
#42317 = CARTESIAN_POINT ( 'NONE',  ( 136.0617147589309752, -10.72514783119565074, -14.09777631113067287 ) ) ;
#42318 = CARTESIAN_POINT ( 'NONE',  ( 114.8384214775786489, -10.15424416112533912, -14.75197769757731336 ) ) ;
#42319 = CARTESIAN_POINT ( 'NONE',  ( 70.19189222814998175, -58.54852247098141049, -36.62221405200617141 ) ) ;
#42320 = CARTESIAN_POINT ( 'NONE',  ( 112.4773541094426719, 0.3591747506842615789, -12.14321520033833046 ) ) ;
#42321 = CARTESIAN_POINT ( 'NONE',  ( 114.6497546295247929, -4.863998795839590272, -18.39754474579285315 ) ) ;
#42322 = CARTESIAN_POINT ( 'NONE',  ( 114.0442481442453300, -7.643976991954077427, -18.09477374809248928 ) ) ;
#42323 = FACE_OUTER_BOUND ( 'NONE', #15158, .T. ) ;
#42324 = EDGE_CURVE ( 'NONE', #18078, #32530, #24498, .T. ) ;
#42325 = CONICAL_SURFACE ( 'NONE', #27751, 1.610000000000000986, 0.9599310885968765916 ) ;
#42326 = DIRECTION ( 'NONE',  ( 0.000000000000000000, -0.9242245927363040847, -0.3818493186865897226 ) ) ;
#42328 = CARTESIAN_POINT ( 'NONE',  ( 119.2631014775786298, 0.2603800115204892296, -16.42320221600525088 ) ) ;
#42327 = DIRECTION ( 'NONE',  ( 0.9609149988134837450, -0.1028163501681639419, 0.2570431154366518145 ) ) ;
#42329 = CARTESIAN_POINT ( 'NONE',  ( 124.9357681442453014, -7.643976991954077427, -18.09477374809248928 ) ) ;
#42330 = CARTESIAN_POINT ( 'NONE',  ( 120.5678148109119832, -1.833838273342659253, -17.42832698103878286 ) ) ;
#42331 = CARTESIAN_POINT ( 'NONE',  ( 113.1933481442453058, -5.574606645277164318, -18.38911715685844683 ) ) ;
#42332 = VERTEX_POINT ( 'NONE', #13533 ) ;
#42333 = CARTESIAN_POINT ( 'NONE',  ( 137.4443952029542118, -8.323847906524228790, -9.667664526382553802 ) ) ;
#42334 = CARTESIAN_POINT ( 'NONE',  ( 121.1918081442452859, 0.9020085738987339008, -11.91225656197089222 ) ) ;
#42335 = CARTESIAN_POINT ( 'NONE',  ( 115.6220983795247861, -8.402594152722688392, -16.93181055722141792 ) ) ;
#42336 = CARTESIAN_POINT ( 'NONE',  ( 118.9227414775786542, 0.4262465694468514643, -12.03445270309931736 ) ) ;
#42337 = EDGE_CURVE ( 'NONE', #11942, #14735, #41362, .T. ) ;
#42338 = CARTESIAN_POINT ( 'NONE',  ( 114.5547881442453217, -4.153390946401321671, -8.397313243818183892 ) ) ;
#42339 = EDGE_CURVE ( 'NONE', #523, #22660, #6688, .T. ) ;
#42340 = CARTESIAN_POINT ( 'NONE',  ( 85.54408422177358773, -28.33925901115217982, -9.149378981526259835 ) ) ;
#42341 = CARTESIAN_POINT ( 'NONE',  ( 114.6497546295247929, -4.863998795839590272, -7.631215200338315796 ) ) ;
#42342 = CARTESIAN_POINT ( 'NONE',  ( 121.3052614775786111, -7.643976991954077427, -18.09477374809248928 ) ) ;
#42343 = CIRCLE ( 'NONE', #23431, 1.000000000000000888 ) ;
#42344 = CARTESIAN_POINT ( 'NONE',  ( 124.7088614775786226, -9.565557343593413364, -10.61323700422348004 ) ) ;
#42345 = CARTESIAN_POINT ( 'NONE',  ( 116.3166296295247832, -4.863998795839541422, -8.388885654883775800 ) ) ;
#42346 = CARTESIAN_POINT ( 'NONE',  ( 109.2295678159355390, -5.842956214023153017, -7.856223403944330386 ) ) ;
#42347 = CARTESIAN_POINT ( 'NONE',  ( 121.4797829359119987, -5.367793381288652910, -18.78638297431638904 ) ) ;
#42348 = CARTESIAN_POINT ( 'NONE',  ( 113.6079577545248043, -7.250697342233347165, -7.631215200338321125 ) ) ;
#42349 = CARTESIAN_POINT ( 'NONE',  ( 116.8168314703984976, 1.985137923759451306, -20.92218200132013806 ) ) ;
#42350 = CARTESIAN_POINT ( 'NONE',  ( 116.0296814775786345, -8.166667518702817929, -8.995218007635861213 ) ) ;
#42351 = CARTESIAN_POINT ( 'NONE',  ( 113.8173414775786512, 0.2603800115204892296, -16.42320221600525088 ) ) ;
#42352 = CARTESIAN_POINT ( 'NONE',  ( 112.7050671295247923, -10.62599879583958540, -13.39321520033831447 ) ) ;
#42353 = DIRECTION ( 'NONE',  ( 0.9609149988134837450, -0.1028163501681639419, 0.2570431154366518145 ) ) ;
#42354 = ORIENTED_EDGE ( 'NONE', *, *, #10663, .T. ) ;
#42355 = DIRECTION ( 'NONE',  ( 0.000000000000000000, -0.3818493186865927203, 0.9242245927363029745 ) ) ;
#42356 = CARTESIAN_POINT ( 'NONE',  ( 124.3117748109119844, -10.30919188438810075, -12.61870101168855918 ) ) ;
#42357 = CARTESIAN_POINT ( 'NONE',  ( 117.6180281442453150, -0.4660016031367893996, -10.09054647747474043 ) ) ;
#42358 = CARTESIAN_POINT ( 'NONE',  ( 123.0637881442452937, -8.899110576539710493, -16.42337572283490132 ) ) ;
#42359 = CARTESIAN_POINT ( 'NONE',  ( 123.9146881442452894, 0.9020085738987339008, -11.91225656197089222 ) ) ;
#42360 = CARTESIAN_POINT ( 'NONE',  ( 121.8158014775786171, -5.638512984488999180, -18.83840828888717311 ) ) ;
#42361 = ADVANCED_FACE ( 'NONE', ( #6905 ), #20815, .T. ) ;
#42362 = CARTESIAN_POINT ( 'NONE',  ( 112.3578015045248861, -2.477300249445798297, -7.631215200338321125 ) ) ;
#42363 = AXIS2_PLACEMENT_3D ( 'NONE', #22378, #18740, #35821 ) ;
#42364 = CARTESIAN_POINT ( 'NONE',  ( 114.6682414775786469, -7.894159318335828068, -9.358103419637847864 ) ) ;
#42365 = CARTESIAN_POINT ( 'NONE',  ( 70.19189222814998175, -57.98054017398621340, -36.39502311309316696 ) ) ;
#42366 = ORIENTED_EDGE ( 'NONE', *, *, #18903, .T. ) ;
#42367 = CARTESIAN_POINT ( 'NONE',  ( 119.8870948109119752, -9.261995988541697145, -16.69588392320189030 ) ) ;
#42368 = CARTESIAN_POINT ( 'NONE',  ( 122.5215798109119874, -2.173413727453600508, -8.297982527556802879 ) ) ;
#42369 = CARTESIAN_POINT ( 'NONE',  ( 117.6747548109119919, -1.834011780172310813, -8.268836392978581529 ) ) ;
#42370 = ORIENTED_EDGE ( 'NONE', *, *, #40899, .T. ) ;
#42371 = CARTESIAN_POINT ( 'NONE',  ( 116.3860827545247787, -2.477300249445798297, -19.15521520033831138 ) ) ;
#42372 = CARTESIAN_POINT ( 'NONE',  ( 64.81879891447307784, -2.621774883878052353, -8.236146696172697901 ) ) ;
#42373 = CARTESIAN_POINT ( 'NONE',  ( 119.7434548109119703, 1.449227268523328505, -18.30678586333412738 ) ) ;
#42374 = CARTESIAN_POINT ( 'NONE',  ( 113.9875214775786532, -8.899110576539710493, -16.42337572283490132 ) ) ;
#42375 = CARTESIAN_POINT ( 'NONE',  ( 64.98167240748409768, -37.86052959031123777, -4.893215200338314474 ) ) ;
#42376 = CARTESIAN_POINT ( 'NONE',  ( 121.1918081442452859, -10.15424416112533912, -14.75197769757731336 ) ) ;
#42377 = FACE_OUTER_BOUND ( 'NONE', #5900, .T. ) ;
#42378 = CARTESIAN_POINT ( 'NONE',  ( 121.9292548109119849, -7.894159318335828068, -9.358103419637847864 ) ) ;
#42379 = CARTESIAN_POINT ( 'NONE',  ( 94.99177781699742695, -25.99489077589524300, -13.39321520033831447 ) ) ;
#42380 = CARTESIAN_POINT ( 'NONE',  ( 119.2063748109119814, -7.894159318335828068, -9.358103419637847864 ) ) ;
#42381 = CARTESIAN_POINT ( 'NONE',  ( 114.1577014775786552, -6.344957434206662583, -7.627207830600332805 ) ) ;
#42382 = CARTESIAN_POINT ( 'NONE',  ( 119.4332814775786318, -0.4660016031367893996, -10.09054647747474043 ) ) ;
#42383 = CARTESIAN_POINT ( 'NONE',  ( 126.3539348109119800, -4.153390946401325223, -8.397313243818185668 ) ) ;
#42384 = CARTESIAN_POINT ( 'NONE',  ( 70.19189222814998175, -60.97346038181336070, -37.59218076343751136 ) ) ;
#42385 = CARTESIAN_POINT ( 'NONE',  ( 120.0572748109119772, -6.222761293078241884, -8.102969835052219238 ) ) ;
#42386 = ORIENTED_EDGE ( 'NONE', *, *, #21820, .T. ) ;
#42387 = CARTESIAN_POINT ( 'NONE',  ( 117.1642148109119859, -9.261995988541697145, -16.69588392320189030 ) ) ;
#42388 = CARTESIAN_POINT ( 'NONE',  ( 114.1635827545248389, -6.936859964151250502, -8.388885654883777576 ) ) ;
#42389 = FACE_OUTER_BOUND ( 'NONE', #6002, .T. ) ;
#42390 = CARTESIAN_POINT ( 'NONE',  ( 114.5108483795247878, -8.402594152722633325, -16.93181055722144990 ) ) ;
#42391 = CIRCLE ( 'NONE', #8894, 3.000000000000002665 ) ;
#42392 = CARTESIAN_POINT ( 'NONE',  ( 123.2292200565388782, -8.485573535863887074, -17.53172993199662599 ) ) ;
#42393 = CARTESIAN_POINT ( 'NONE',  ( 122.4965214775786251, -10.30919188438810075, -12.61870101168855918 ) ) ;
#42394 = ORIENTED_EDGE ( 'NONE', *, *, #33687, .F. ) ;
#42395 = CARTESIAN_POINT ( 'NONE',  ( 127.0264730702701286, -8.889494433193872780, -9.787842429323326598 ) ) ;
#42396 = CARTESIAN_POINT ( 'NONE',  ( 122.6667014775786413, -2.084020599724406786, -8.691656652584148546 ) ) ;
#42397 = FACE_OUTER_BOUND ( 'NONE', #41814, .T. ) ;
#42398 = CARTESIAN_POINT ( 'NONE',  ( 62.93948576833484054, -14.63887389195935107, -17.26917803626528780 ) ) ;
#42399 = ADVANCED_FACE ( 'NONE', ( #42013 ), #4814, .T. ) ;
#42400 = CARTESIAN_POINT ( 'NONE',  ( 125.6164881442453094, 0.2603800115204892296, -16.42320221600525088 ) ) ;
#42401 = CARTESIAN_POINT ( 'NONE',  ( 112.7745202545247878, 0.1403307496149616695, -11.32035403202665336 ) ) ;
#42402 = EDGE_LOOP ( 'NONE', ( #21209, #34815, #26657, #12556, #2247 ) ) ;
#42403 = CARTESIAN_POINT ( 'NONE',  ( 115.4624148109119943, -5.638512984488999180, -18.83840828888717311 ) ) ;
#42404 = CIRCLE ( 'NONE', #22728, 2.999999999999999556 ) ;
#42405 = CARTESIAN_POINT ( 'NONE',  ( 124.4819548109119722, -2.084020599724406786, -8.691656652584148546 ) ) ;
#42406 = CARTESIAN_POINT ( 'NONE',  ( 67.19031194842951038, -1.707697914625855296, -12.39321520033831447 ) ) ;
#42407 = CARTESIAN_POINT ( 'NONE',  ( 122.1561614775786353, -8.899110576539710493, -16.42337572283490132 ) ) ;
#42408 = CARTESIAN_POINT ( 'NONE',  ( 126.2758031835872430, -3.873803345569537093, -8.462975944311656562 ) ) ;
#42409 = CARTESIAN_POINT ( 'NONE',  ( 68.68839935636917460, -25.95913848132418522, -5.893215200338315363 ) ) ;
#42410 = CARTESIAN_POINT ( 'NONE',  ( 121.7590748109119687, -7.893985811506177619, -18.51759400769804742 ) ) ;
#42411 = CARTESIAN_POINT ( 'NONE',  ( 111.4348214775786801, -3.505236298600246325, -18.68346056562440793 ) ) ;
#42412 = CARTESIAN_POINT ( 'NONE',  ( 73.07463722459043254, -62.00290045216418378, -37.10944531181986861 ) ) ;
#42413 = CARTESIAN_POINT ( 'NONE',  ( 110.1582811052981867, 0.4930828106259610433, -12.14321520033828428 ) ) ;
#42414 = DIRECTION ( 'NONE',  ( -0.000000000000000000, -0.9284778069183718952, -0.3713878862591649677 ) ) ;
#42415 = ORIENTED_EDGE ( 'NONE', *, *, #17484, .T. ) ;
#42416 = CARTESIAN_POINT ( 'NONE',  ( 115.2053796295247849, -4.863998795839590272, -8.388885654883775800 ) ) ;
#42417 = CARTESIAN_POINT ( 'NONE',  ( 122.0994348109119443, 0.9020085738987339008, -11.91225656197089222 ) ) ;
#42418 = CARTESIAN_POINT ( 'NONE',  ( 137.3019930433569016, -8.520726449178049222, -17.11237870612375644 ) ) ;
#42419 = ORIENTED_EDGE ( 'NONE', *, *, #19468, .F. ) ;
#42420 = EDGE_CURVE ( 'NONE', #41268, #33252, #430, .T. ) ;
#42421 =( BOUNDED_CURVE ( )  B_SPLINE_CURVE ( 3, ( #42206, #21225, #38532, #10308 ),
 .UNSPECIFIED., .F., .T. ) 
 B_SPLINE_CURVE_WITH_KNOTS ( ( 4, 4 ),
 ( 4.703285054500009998, 4.712388980384689674 ),
 .UNSPECIFIED. ) 
 CURVE ( )  GEOMETRIC_REPRESENTATION_ITEM ( )  RATIONAL_B_SPLINE_CURVE ( ( 1.000000000000000000, 0.9999930932230500780, 0.9999930932230500780, 1.000000000000000000 ) ) 
 REPRESENTATION_ITEM ( '' )  );
#42422 = CARTESIAN_POINT ( 'NONE',  ( 84.77016061404391678, -26.60966817898065884, -11.90521360603286816 ) ) ;
#42423 = CARTESIAN_POINT ( 'NONE',  ( 112.4559014775786778, -0.1624402480850797581, -16.17319339645315424 ) ) ;
#42424 = CARTESIAN_POINT ( 'NONE',  ( 111.3854577545248503, -2.791137627527887410, -18.39754474579284249 ) ) ;
#42425 = CARTESIAN_POINT ( 'NONE',  ( 122.4965214775786251, 0.1319031606808879209, -14.10382304977623669 ) ) ;
#42426 = ORIENTED_EDGE ( 'NONE', *, *, #18739, .F. ) ;
#42427 = AXIS2_PLACEMENT_3D ( 'NONE', #31835, #604, #24774 ) ;
#42428 = CARTESIAN_POINT ( 'NONE',  ( 112.8529881442453302, -1.561330072975668060, -17.79121239304076596 ) ) ;
#42429 = DIRECTION ( 'NONE',  ( 0.000000000000000000, -0.6004852223388320587, 0.7996358532186281787 ) ) ;
#42430 = CARTESIAN_POINT ( 'NONE',  ( 79.40221886803639961, 5.047344816279970559, -20.48083050651887405 ) ) ;
#42431 = CARTESIAN_POINT ( 'NONE',  ( 138.2184548109119930, -7.067465109756605912, -7.812468278694988832 ) ) ;
#42432 = CARTESIAN_POINT ( 'NONE',  ( 124.1983214775786166, -8.166667518702819706, -8.995218007635861213 ) ) ;
#42433 = CARTESIAN_POINT ( 'NONE',  ( 87.80477198183443477, -25.99489077589524300, -13.39321520033831625 ) ) ;
#42434 = CARTESIAN_POINT ( 'NONE',  ( 91.38554522942851577, -25.99489077589524300, -13.39321520033831625 ) ) ;
#42435 = CARTESIAN_POINT ( 'NONE',  ( 124.5386814775786206, -5.638512984488999180, -18.83840828888717311 ) ) ;
#42437 = CARTESIAN_POINT ( 'NONE',  ( 124.5386814775786206, -4.153390946401325223, -8.397313243818185668 ) ) ;
#42436 = CARTESIAN_POINT ( 'NONE',  ( 123.8012348109119642, 0.2603800115204892296, -16.42320221600525088 ) ) ;
#42438 = CARTESIAN_POINT ( 'NONE',  ( 123.2339681442453241, -3.505236298600246325, -18.68346056562440793 ) ) ;
#42439 = CARTESIAN_POINT ( 'NONE',  ( 75.95778847736514194, -3.256761025687008537, -14.39321520033831625 ) ) ;
#42440 = CARTESIAN_POINT ( 'NONE',  ( 120.5110881442453206, -6.344957434206665248, -7.627207830600338134 ) ) ;
#42441 = VERTEX_POINT ( 'NONE', #21707 ) ;
#42442 = ORIENTED_EDGE ( 'NONE', *, *, #14261, .T. ) ;
#42443 = CARTESIAN_POINT ( 'NONE',  ( 113.1706121053768186, 0.3967854368540359999, -16.28112951403850772 ) ) ;
#42444 = CARTESIAN_POINT ( 'NONE',  ( 114.7886608795247696, -8.938348069036489818, -9.318865927141430916 ) ) ;
#42445 = CARTESIAN_POINT ( 'NONE',  ( 114.5803015045248117, -6.936859964151250502, -18.39754474579286025 ) ) ;
#42446 = CARTESIAN_POINT ( 'NONE',  ( 114.6497546295247929, -4.863998795839590272, -18.39754474579285315 ) ) ;
#42447 = CARTESIAN_POINT ( 'NONE',  ( 125.8433948109119456, -1.834011780172310813, -8.268836392978581529 ) ) ;
#42448 = CARTESIAN_POINT ( 'NONE',  ( 126.0135748109119902, -1.833838273342660141, -17.42832698103878286 ) ) ;
#42449 = ORIENTED_EDGE ( 'NONE', *, *, #23940, .F. ) ;
#42450 = CARTESIAN_POINT ( 'NONE',  ( 112.8529881442453160, -7.894159318335828068, -9.358103419637847864 ) ) ;
#42451 = CARTESIAN_POINT ( 'NONE',  ( 107.3571765045248299, -7.250697342233347165, -19.15521520033831138 ) ) ;
#42452 = CARTESIAN_POINT ( 'NONE',  ( 118.9227414775786542, 0.4262465694468589028, -12.03445270309934578 ) ) ;
#42453 = CARTESIAN_POINT ( 'NONE',  ( 125.9001214775786224, -4.089484607189486809, -7.948022111789456723 ) ) ;
#42454 = CARTESIAN_POINT ( 'NONE',  ( 126.1270281442452870, -10.30919188438810075, -12.61870101168855918 ) ) ;
#42455 = CARTESIAN_POINT ( 'NONE',  ( 64.76452260854004805, -13.87123648633731854, -17.75937495128697918 ) ) ;
#42456 = CARTESIAN_POINT ( 'NONE',  ( 114.7816948109119863, 0.5811942927096154232, -14.16772938898807155 ) ) ;
#42457 = AXIS2_PLACEMENT_3D ( 'NONE', #1610, #19624, #19180 ) ;
#42458 = CARTESIAN_POINT ( 'NONE',  ( 113.5385046295247804, -4.863998795839590272, -7.631215200338315796 ) ) ;
#42459 = CARTESIAN_POINT ( 'NONE',  ( 111.8716296295247901, -4.863998795839590272, -8.388885654883775800 ) ) ;
#42460 = VERTEX_POINT ( 'NONE', #22153 ) ;
#42461 = DIRECTION ( 'NONE',  ( 0.000000000000000000, -0.3818493186865927203, 0.9242245927363029745 ) ) ;
#42462 = CARTESIAN_POINT ( 'NONE',  ( 113.6471614775786492, -4.153390946401321671, -8.397313243818183892 ) ) ;
#42463 = AXIS2_PLACEMENT_3D ( 'NONE', #31116, #13130, #37505 ) ;
#42464 = CARTESIAN_POINT ( 'NONE',  ( 125.8433948109119456, -7.643976991954077427, -18.09477374809248928 ) ) ;
#42465 = CARTESIAN_POINT ( 'NONE',  ( 113.3635281442453504, -9.988377603198976828, -10.36322818467138340 ) ) ;
#42466 = CARTESIAN_POINT ( 'NONE',  ( 124.6521348109119884, -7.894159318335828068, -9.358103419637847864 ) ) ;
#42467 = UNCERTAINTY_MEASURE_WITH_UNIT (LENGTH_MEASURE( 1.000000000000000082E-05 ), #25819, 'distance_accuracy_value', 'NONE');
#42468 = CARTESIAN_POINT ( 'NONE',  ( 119.5467348109119712, -5.574606645277164318, -18.38911715685844683 ) ) ;
#42469 = CARTESIAN_POINT ( 'NONE',  ( 114.6115148109119986, -6.222761293078241884, -8.102969835052219238 ) ) ;
#42470 = VERTEX_POINT ( 'NONE', #4140 ) ;
#42471 = CARTESIAN_POINT ( 'NONE',  ( 122.9382985609119743, -0.08252387247370887580, -11.91645802438286417 ) ) ;
#42472 = AXIS2_PLACEMENT_3D ( 'NONE', #39104, #42978, #11527 ) ;
#42473 = EDGE_CURVE ( 'NONE', #43753, #30603, #31035, .T. ) ;
#42474 = CARTESIAN_POINT ( 'NONE',  ( 91.65862616933031859, -25.99489077589524300, -13.39321520033831447 ) ) ;
#42475 = CARTESIAN_POINT ( 'NONE',  ( 116.7671281442453335, -7.643976991954077427, -18.09477374809248928 ) ) ;
#42476 = ORIENTED_EDGE ( 'NONE', *, *, #1121, .T. ) ;
#42477 = CARTESIAN_POINT ( 'NONE',  ( 126.2184548109092930, -8.879494022685642918, -16.37258252134538949 ) ) ;
#42478 = CARTESIAN_POINT ( 'NONE',  ( 112.4559014775786494, -9.988377603198976828, -10.36322818467138340 ) ) ;
#42479 = CARTESIAN_POINT ( 'NONE',  ( 107.0793640045248196, 0.1403307496149616695, -15.46607636864997204 ) ) ;
#42480 = CARTESIAN_POINT ( 'NONE',  ( 118.9907502882355033, -1.135392229370316031, -17.10942237759952533 ) ) ;
#42481 = VERTEX_POINT ( 'NONE', #25578 ) ;
#42482 = VERTEX_POINT ( 'NONE', #42685 ) ;
#42483 = CARTESIAN_POINT ( 'NONE',  ( 117.8449348109119938, -1.833838273342659253, -17.42832698103878286 ) ) ;
#42484 = CARTESIAN_POINT ( 'NONE',  ( 118.8092881442453290, -0.1624402480850797581, -16.17319339645315424 ) ) ;
#42485 = CARTESIAN_POINT ( 'NONE',  ( 124.5917477490678777, -9.748629547111955063, -14.47908513545650955 ) ) ;
#42486 = CARTESIAN_POINT ( 'NONE',  ( 121.8270485609119760, -10.36940331770106916, -15.09355782777062061 ) ) ;
#42487 = ORIENTED_EDGE ( 'NONE', *, *, #40126, .T. ) ;
#42488 = VECTOR ( 'NONE', #13250, 1000.000000000000000 ) ;
#42489 = CARTESIAN_POINT ( 'NONE',  ( 121.0408330757767459, -0.9924539043446216624, -17.29976612834909133 ) ) ;
#42490 = CARTESIAN_POINT ( 'NONE',  ( 125.3303382280751492, -1.129804808602307586, -7.332909019048677202 ) ) ;
#42491 = CARTESIAN_POINT ( 'NONE',  ( 112.9134265045247645, -7.250697342233347165, -19.15521520033831138 ) ) ;
#42492 = CIRCLE ( 'NONE', #5340, 6.999999999999999112 ) ;
#42493 = EDGE_CURVE ( 'NONE', #43396, #29748, #44204, .T. ) ;
#42494 = CARTESIAN_POINT ( 'NONE',  ( 112.6260814775786514, -9.261995988541697145, -16.69588392320189030 ) ) ;
#42495 = CARTESIAN_POINT ( 'NONE',  ( 113.4202548109119846, -10.30919188438810075, -12.61870101168855918 ) ) ;
#42496 = CARTESIAN_POINT ( 'NONE',  ( 118.2420214775786320, -6.222761293078241884, -8.102969835052219238 ) ) ;
#42497 = DIRECTION ( 'NONE',  ( 0.9609149988134837450, -0.1028163501681639419, 0.2570431154366518145 ) ) ;
#42498 = ORIENTED_EDGE ( 'NONE', *, *, #45007, .F. ) ;
#42499 = CARTESIAN_POINT ( 'NONE',  ( 116.1998614775786507, 0.4262465694468514643, -12.03445270309931736 ) ) ;
#42500 = CARTESIAN_POINT ( 'NONE',  ( 91.23658249893594530, -5.844616714554617509, -9.893215200338316251 ) ) ;
#42501 = AXIS2_PLACEMENT_3D ( 'NONE', #18420, #15442, #7460 ) ;
#42502 = CARTESIAN_POINT ( 'NONE',  ( 64.85649322025210495, -35.54674243456235416, -5.785566283887345840 ) ) ;
#42503 = CARTESIAN_POINT ( 'NONE',  ( 69.37572422742091760, -11.86958442233774313, -21.89321520033831447 ) ) ;
#42504 = CARTESIAN_POINT ( 'NONE',  ( 115.8027748109119841, -0.4660016031367893996, -10.09054647747474043 ) ) ;
#42505 = VERTEX_POINT ( 'NONE', #11000 ) ;
#42506 = CARTESIAN_POINT ( 'NONE',  ( 118.0718414775786300, -9.261995988541697145, -16.69588392320189030 ) ) ;
#42507 = CARTESIAN_POINT ( 'NONE',  ( 114.6490365460471992, -2.191907684172563986, -18.20049396185734025 ) ) ;
#42508 = CARTESIAN_POINT ( 'NONE',  ( 110.4131140045248287, -10.62599879583958717, -11.00651665394454604 ) ) ;
#42509 = CARTESIAN_POINT ( 'NONE',  ( 117.9016614775786280, -9.988377603198976828, -10.36322818467138340 ) ) ;
#42510 = CARTESIAN_POINT ( 'NONE',  ( 113.9307948109119906, 0.9020085738987339008, -11.91225656197089222 ) ) ;
#42511 = FACE_OUTER_BOUND ( 'NONE', #11544, .T. ) ;
#42512 = CARTESIAN_POINT ( 'NONE',  ( 90.72400676789006013, -25.99489077589524300, -13.39321520033831625 ) ) ;
#42513 = CARTESIAN_POINT ( 'NONE',  ( 106.4542858795248179, -8.402594152722688392, -9.854619843455216355 ) ) ;
#42514 = ORIENTED_EDGE ( 'NONE', *, *, #34728, .T. ) ;
#42515 = CARTESIAN_POINT ( 'NONE',  ( 116.0388171295248014, -10.62599879583958540, -13.39321520033831447 ) ) ;
#42516 = CARTESIAN_POINT ( 'NONE',  ( 109.2294425275515266, -7.200841873015452421, -18.15047811013180024 ) ) ;
#42517 = CARTESIAN_POINT ( 'NONE',  ( 116.3133148109120043, -2.084020599724406786, -8.691656652584148546 ) ) ;
#42518 = LINE ( 'NONE', #4197, #17573 ) ;
#42519 = CARTESIAN_POINT ( 'NONE',  ( 116.0388171295248014, 0.1403307496149613920, -13.39321520033831447 ) ) ;
#42520 = CARTESIAN_POINT ( 'NONE',  ( 114.6497546295247929, -4.863998795839590272, -18.39754474579285315 ) ) ;
#42521 = CARTESIAN_POINT ( 'NONE',  ( 121.8701654349294472, -1.040089454026960292, -17.23633227186633476 ) ) ;
#42522 = CARTESIAN_POINT ( 'NONE',  ( 113.1366214775786432, -7.643976991954077427, -18.09477374809248928 ) ) ;
#42523 = CARTESIAN_POINT ( 'NONE',  ( 135.5177942504587350, 1.083030826940885927, -12.63729283143848825 ) ) ;
#42524 = CARTESIAN_POINT ( 'NONE',  ( 123.0070614775786169, 0.9020085738987339008, -11.91225656197089222 ) ) ;
#42525 = CARTESIAN_POINT ( 'NONE',  ( 121.4754414775786131, -8.166667518702819706, -8.995218007635861213 ) ) ;
#42526 = VERTEX_POINT ( 'NONE', #14191 ) ;
#42527 = CLOSED_SHELL ( 'NONE', ( #31227, #31743, #21375, #8459, #40461, #26448, #13332, #23164, #23158, #15571, #27816, #26190, #15828, #4660, #43546, #33947, #20566, #4192, #1908, #23356, #33113, #34559, #40967, #41994, #8011, #30163, #40649, #26191, #10038, #11113, #27656, #34816, #7000, #35429, #10271, #44112, #10518, #3334, #26507, #8872, #11176, #16010, #25054, #33728, #27314, #26437, #38367, #22589, #28969, #40381, #23218, #38974, #3027, #20191, #28459, #9447, #15551, #2740, #19151, #41190, #23749, #21394, #18348, #42923, #12620, #21434, #17858, #14823, #3303, #6350, #10602, #27013, #19818, #40050, #19355, #25932, #9457, #3563, #24799, #25023 ) ) ;
#42528 = CARTESIAN_POINT ( 'NONE',  ( 116.7671281442453335, -7.643976991954077427, -18.09477374809248928 ) ) ;
#42529 = CARTESIAN_POINT ( 'NONE',  ( 112.7962614775786676, -3.383040157471821630, -19.15922257007629170 ) ) ;
#42530 = CARTESIAN_POINT ( 'NONE',  ( 118.1285681442453068, -7.893985811506177619, -18.51759400769804742 ) ) ;
#42531 = CARTESIAN_POINT ( 'NONE',  ( 120.3409081442453044, -8.899110576539710493, -16.42337572283490132 ) ) ;
#42532 = ORIENTED_EDGE ( 'NONE', *, *, #36180, .T. ) ;
#42533 = CARTESIAN_POINT ( 'NONE',  ( 120.0005481442453146, -4.153390946401325223, -8.397313243818185668 ) ) ;
#42534 = CARTESIAN_POINT ( 'NONE',  ( 121.2485348109119769, -0.4660016031367893996, -10.09054647747474043 ) ) ;
#42535 = CARTESIAN_POINT ( 'NONE',  ( 136.9555737971644760, 0.6158828431329258501, -13.00173388423986864 ) ) ;
#42536 = CARTESIAN_POINT ( 'NONE',  ( 108.8851452545248151, 0.8980012041604421569, -11.00651665394454071 ) ) ;
#42537 = CYLINDRICAL_SURFACE ( 'NONE', #32966, 0.9999999999999990008 ) ;
#42538 = CARTESIAN_POINT ( 'NONE',  ( 127.3815943569765210, 0.6976231769725066423, -12.91654422016494053 ) ) ;
#42539 = CARTESIAN_POINT ( 'NONE',  ( 112.3578015045248861, -6.936859964151250502, -18.39754474579286025 ) ) ;
#42540 = CARTESIAN_POINT ( 'NONE',  ( 115.5758681442453053, -1.561330072975668060, -17.79121239304076951 ) ) ;
#42541 = CARTESIAN_POINT ( 'NONE',  ( 137.1399781294006175, -10.21614541919964658, -13.63713482494530638 ) ) ;
#42542 = CARTESIAN_POINT ( 'NONE',  ( 116.0296814775786345, -1.833838273342658809, -17.42832698103878286 ) ) ;
#42543 = DIRECTION ( 'NONE',  ( 0.9609149988134837450, -0.1028163501681639419, 0.2570431154366518145 ) ) ;
#42544 = CARTESIAN_POINT ( 'NONE',  ( 112.5680291257774854, 0.2334052082820642360, -12.14321520033833046 ) ) ;
#42545 = CARTESIAN_POINT ( 'NONE',  ( 110.4825671295247815, 0.1403307496149613920, -13.39321520033831447 ) ) ;
#42546 = CARTESIAN_POINT ( 'NONE',  ( 112.5126281442453120, 0.1319031606808879209, -14.10382304977623669 ) ) ;
#42547 = CARTESIAN_POINT ( 'NONE',  ( 123.3550173109119612, -9.289237151508428880, -11.05642687123710211 ) ) ;
#42548 = LINE ( 'NONE', #28865, #34055 ) ;
#42550 = CARTESIAN_POINT ( 'NONE',  ( 119.0929214775786278, -5.638512984488999180, -18.83840828888717311 ) ) ;
#42549 = CARTESIAN_POINT ( 'NONE',  ( 63.69959400472163935, -14.91280095328349020, -10.08899308684463847 ) ) ;
#42551 = CARTESIAN_POINT ( 'NONE',  ( 119.6601881442453106, -1.833838273342659253, -17.42832698103878286 ) ) ;
#42552 = CARTESIAN_POINT ( 'NONE',  ( 111.3213681442453264, -7.643976991954077427, -18.09477374809248928 ) ) ;
#42553 = ORIENTED_EDGE ( 'NONE', *, *, #1337, .F. ) ;
#42554 = CARTESIAN_POINT ( 'NONE',  ( 136.7036351578981055, -7.108649276388896432, -8.207337658509201717 ) ) ;
#42555 = CARTESIAN_POINT ( 'NONE',  ( 121.8725281442453223, -3.383040157471821630, -19.15922257007629170 ) ) ;
#42556 = CARTESIAN_POINT ( 'NONE',  ( 114.0941296295247867, -4.863998795839590272, -8.388885654883775800 ) ) ;
#42557 = CARTESIAN_POINT ( 'NONE',  ( 120.1140014775786398, -7.894159318335828068, -9.358103419637847864 ) ) ;
#42558 = EDGE_CURVE ( 'NONE', #37411, #32004, #11350, .T. ) ;
#42559 = CARTESIAN_POINT ( 'NONE',  ( 115.0653281442453277, -3.505236298600246325, -18.68346056562440793 ) ) ;
#42560 = CARTESIAN_POINT ( 'NONE',  ( 84.99660211880991767, -29.66455880986359261, -10.80014759642894084 ) ) ;
#42561 = CARTESIAN_POINT ( 'NONE',  ( 114.1635827545248389, -2.477300249445798297, -19.15521520033831138 ) ) ;
#42562 = CARTESIAN_POINT ( 'NONE',  ( 120.6245414775786458, -0.1624402480850797581, -16.17319339645315424 ) ) ;
#42563 = CARTESIAN_POINT ( 'NONE',  ( 125.3895814775786448, -2.084020599724406786, -8.691656652584148546 ) ) ;
#42564 = DIRECTION ( 'NONE',  ( 0.000000000000000000, -0.9242245927363028635, -0.3818493186865930533 ) ) ;
#42565 = CARTESIAN_POINT ( 'NONE',  ( 109.2294432708102221, -4.940976372564280794, -7.813933925037506611 ) ) ;
#42566 = CARTESIAN_POINT ( 'NONE',  ( 121.8965016859119856, -0.6942167230862511529, -9.935906262978006609 ) ) ;
#42567 = CARTESIAN_POINT ( 'NONE',  ( 115.0664733795247798, -8.938348069036489818, -17.46756447353520159 ) ) ;
#42568 = CARTESIAN_POINT ( 'NONE',  ( 117.1097356970102084, 1.580032931476776481, -21.38384006208493915 ) ) ;
#42569 = CARTESIAN_POINT ( 'NONE',  ( 118.9794681442453026, -9.261995988541697145, -16.69588392320189030 ) ) ;
#42570 = CARTESIAN_POINT ( 'NONE',  ( 118.0151148109119816, -10.63000616557722466, -14.87417383870573495 ) ) ;
#42571 = CARTESIAN_POINT ( 'NONE',  ( 112.2883483795247770, -0.7896495226426338832, -9.318865927141430916 ) ) ;
#42572 = CARTESIAN_POINT ( 'NONE',  ( 114.4413348109119823, -9.261995988541697145, -16.69588392320189030 ) ) ;
#42573 = ORIENTED_EDGE ( 'NONE', *, *, #35034, .F. ) ;
#42574 = CARTESIAN_POINT ( 'NONE',  ( 123.2184548109119788, -4.863998795839242995, -13.39321520033831447 ) ) ;
#42575 = B_SPLINE_CURVE_WITH_KNOTS ( 'NONE', 3,
 ( #41409, #40954, #9709, #30901, #23621, #20202, #18339, #11050, #770, #14244, #14692, #24954, #110, #25184, #331, #7852, #35419, #3742, #39083, #3967, #20866, #17443, #31562, #14468, #21079, #42289, #31786, #3525, #10386, #4424, #21758, #28160, #35650, #10608, #24295, #35190, #28830, #31336, #32233, #4195, #38849, #21531, #14920, #28376, #17666, #34744, #41848, #1004, #42516, #38182, #7618, #18113, #32006, #11276, #6959, #17888, #14024, #28607, #558, #24511, #27938, #42070, #38396, #7168, #34956, #10828, #24725, #38613, #7389, #21307, #4642, #8744, #12403, #15368, #19237, #15817, #16042, #19006, #29716, #25850, #5539, #36099, #43629, #22204, #18564, #33120, #22651, #39541, #1668, #1888, #25636, #26303, #40210, #1230, #11952, #8526, #22428, #4871, #5321, #29049, #2113, #36547, #8977, #22875, #11506, #32892, #36769, #11724, #19457, #39756, #32678, #33340, #36320, #32455, #15591, #26076, #25410, #42741, #5090, #29494, #43407, #12175, #39310, #42957, #8080, #21981, #35871, #15143, #29272, #8302, #18788 ),
 .UNSPECIFIED., .F., .F.,
 ( 4, 2, 2, 2, 1, 1, 1, 2, 2, 2, 2, 1, 1, 1, 2, 2, 2, 2, 1, 1, 1, 1, 2, 2, 2, 2, 2, 2, 1, 1, 1, 2, 2, 2, 2, 1, 1, 2, 2, 2, 2, 1, 1, 1, 1, 2, 2, 2, 2, 2, 2, 1, 1, 1, 2, 2, 2, 2, 1, 1, 2, 2, 2, 2, 1, 1, 1, 1, 2, 2, 2, 2, 2, 2, 1, 1, 1, 2, 2, 2, 4 ),
 ( 0.000000000000000000, 0.06249999999995042854, 0.09374999999992583710, 0.1093749999999135691, 0.1171874999999075323, 0.1210937499999046457, 0.1230468749999032024, 0.1240234374999024808, 0.1249999999999017453, 0.1562499999998799571, 0.1718749999998689937, 0.1796874999998634981, 0.1835937499998608613, 0.1855468749998595290, 0.1865234374998589462, 0.1874999999998583633, 0.2187499999998322175, 0.2343749999998191169, 0.2421874999998125666, 0.2460937499998093192, 0.2480468749998077649, 0.2490234374998069877, 0.2495117187498066547, 0.2499999999998063216, 0.3124999999997608024, 0.3437499999997379319, 0.3593749999997266076, 0.3671874999997210010, 0.3710937499997181144, 0.3730468749997166711, 0.3740234374997159494, 0.3745117187497156164, 0.3749999999997152833, 0.4062499999997020161, 0.4218749999996954103, 0.4296874999996921352, 0.4335937499996906919, 0.4355468749996899702, 0.4374999999996892486, 0.4687499999996765365, 0.4843749999996702083, 0.4921874999996670441, 0.4960937499996653233, 0.4980468749996646016, 0.4990234374996641575, 0.4995117187496638245, 0.4999999999996634914, 0.5624999999997134514, 0.5937499999997383204, 0.6093749999997509770, 0.6171874999997574163, 0.6210937499997605249, 0.6230468749997619682, 0.6240234374997627453, 0.6245117187497630784, 0.6249999999997635225, 0.6562499999997883915, 0.6718749999998008260, 0.6796874999998070432, 0.6835937499998102629, 0.6855468749998119282, 0.6874999999998135936, 0.7187499999998397948, 0.7343749999998528954, 0.7421874999998594458, 0.7460937499998626654, 0.7480468749998644418, 0.7490234374998653299, 0.7495117187498657740, 0.7499999999998663291, 0.8124999999998983036, 0.8437499999999145128, 0.8593749999999226175, 0.8671874999999266143, 0.8710937499999286127, 0.8730468749999297229, 0.8740234374999301670, 0.8745117187499302780, 0.8749999999999305000, 0.9374999999999651390, 1.000000000000000000 ),
 .UNSPECIFIED. ) ;
#42576 = CIRCLE ( 'NONE', #6145, 8.000000000000001776 ) ;
#42577 = CARTESIAN_POINT ( 'NONE',  ( 116.9940348109119839, -9.988377603198976828, -10.36322818467138340 ) ) ;
#42578 = CARTESIAN_POINT ( 'NONE',  ( 122.1561614775786353, -8.899110576539710493, -16.42337572283490132 ) ) ;
#42579 = CARTESIAN_POINT ( 'NONE',  ( 112.0588148109119828, -9.859900752359374465, -12.68260735090039404 ) ) ;
#42580 = CARTESIAN_POINT ( 'NONE',  ( 122.8936081442453059, 0.2603800115204892296, -16.42320221600525088 ) ) ;
#42581 = AXIS2_PLACEMENT_3D ( 'NONE', #22295, #32325, #11588 ) ;
#42582 = ADVANCED_FACE ( 'NONE', ( #7337 ), #35135, .T. ) ;
#42583 = CARTESIAN_POINT ( 'NONE',  ( 113.9552233795247815, -8.938348069036489818, -17.46756447353520159 ) ) ;
#42584 = CARTESIAN_POINT ( 'NONE',  ( 115.4624148109119943, -4.153390946401321671, -8.397313243818183892 ) ) ;
#42585 = CARTESIAN_POINT ( 'NONE',  ( 121.4797829359119987, -4.283928203966213211, -7.183505701512925334 ) ) ;
#42586 = CARTESIAN_POINT ( 'NONE',  ( 123.6803214993270643, -5.999514616106329967, -18.26332968281675662 ) ) ;
#42587 = EDGE_LOOP ( 'NONE', ( #20175, #27177, #36294, #27277, #10277, #33134 ) ) ;
#42588 = EDGE_CURVE ( 'NONE', #30333, #37160, #36876, .T. ) ;
#42589 = CARTESIAN_POINT ( 'NONE',  ( 122.8688454359119646, -11.07370829466463569, -12.81314460846529002 ) ) ;
#42590 = EDGE_CURVE ( 'NONE', #816, #12848, #11226, .T. ) ;
#42591 = CARTESIAN_POINT ( 'NONE',  ( 118.9794681442453026, -9.261995988541697145, -16.69588392320189030 ) ) ;
#42592 = ORIENTED_EDGE ( 'NONE', *, *, #7822, .T. ) ;
#42593 = CARTESIAN_POINT ( 'NONE',  ( 55.39394582045726168, -26.25884925591183716, -7.393215200338315363 ) ) ;
#42594 = CARTESIAN_POINT ( 'NONE',  ( -13.78096647419814680, -4.499153416623470569, -8.147705117616510506 ) ) ;
#42595 = LINE ( 'NONE', #11357, #41298 ) ;
#42596 = CARTESIAN_POINT ( 'NONE',  ( 116.3133148109120043, -2.084020599724406786, -8.691656652584148546 ) ) ;
#42597 = CARTESIAN_POINT ( 'NONE',  ( 77.39830673346236267, -56.66119886563520680, -1.782287558316724141 ) ) ;
#42598 = CARTESIAN_POINT ( 'NONE',  ( 64.22513517183551812, -35.03390339818633947, -5.893215200338315363 ) ) ;
#42599 = CARTESIAN_POINT ( 'NONE',  ( 119.0361948109119652, -2.084020599724406786, -8.691656652584148546 ) ) ;
#42600 = CARTESIAN_POINT ( 'NONE',  ( 123.6776560953690591, -6.001247023715324147, -18.26661038929047010 ) ) ;
#42601 = EDGE_CURVE ( 'NONE', #16972, #16620, #33989, .T. ) ;
#42602 = CARTESIAN_POINT ( 'NONE',  ( 122.0994348109119443, -10.15424416112533912, -14.75197769757731336 ) ) ;
#42603 = CARTESIAN_POINT ( 'NONE',  ( 121.9484597424434043, -0.9924539043446216624, -17.29976612834909133 ) ) ;
#42604 = CARTESIAN_POINT ( 'NONE',  ( 120.0005481442453146, -4.153390946401325223, -8.397313243818185668 ) ) ;
#42605 = EDGE_CURVE ( 'NONE', #41400, #27136, #16778, .T. ) ;
#42606 = CARTESIAN_POINT ( 'NONE',  ( 113.5337081442453240, -9.261995988541697145, -16.69588392320189030 ) ) ;
#42607 = CARTESIAN_POINT ( 'NONE',  ( 118.5256548109119876, -0.4660016031367893996, -10.09054647747474043 ) ) ;
#42608 = CARTESIAN_POINT ( 'NONE',  ( 112.3991748109119868, -8.166667518702817929, -8.995218007635859436 ) ) ;
#42609 = DIRECTION ( 'NONE',  ( -1.000000000000000000, 0.000000000000000000, 0.000000000000000000 ) ) ;
#42610 = ADVANCED_FACE ( 'NONE', ( #30123 ), #23279, .F. ) ;
#42611 = AXIS2_PLACEMENT_3D ( 'NONE', #25442, #38646, #28637 ) ;
#42612 = CARTESIAN_POINT ( 'NONE',  ( 121.3052614775786111, -7.643976991954077427, -18.09477374809248928 ) ) ;
#42613 = ORIENTED_EDGE ( 'NONE', *, *, #43534, .T. ) ;
#42614 = CARTESIAN_POINT ( 'NONE',  ( 119.8870948109119752, -9.261995988541697145, -16.69588392320189030 ) ) ;
#42615 = CARTESIAN_POINT ( 'NONE',  ( 113.5385046295247804, -4.863998795839590272, -18.39754474579285315 ) ) ;
#42616 = DIRECTION ( 'NONE',  ( -0.000000000000000000, -0.9284778069183721172, -0.3713878862591650232 ) ) ;
#42617 = CARTESIAN_POINT ( 'NONE',  ( 63.43088374006683239, -46.96404483173760269, -16.39321520033831447 ) ) ;
#42618 = CARTESIAN_POINT ( 'NONE',  ( 122.3132204359119868, -10.25716656981731489, -12.88942061488890545 ) ) ;
#42619 = CARTESIAN_POINT ( 'NONE',  ( 125.1059481442452750, -8.166667518702819706, -8.995218007635861213 ) ) ;
#42620 = ORIENTED_EDGE ( 'NONE', *, *, #37165, .F. ) ;
#42621 = CARTESIAN_POINT ( 'NONE',  ( 87.14323352029596492, -25.99489077589524300, -13.39321520033831625 ) ) ;
#42622 = CARTESIAN_POINT ( 'NONE',  ( 120.5110881442453206, -3.505236298600246325, -18.68346056562440793 ) ) ;
#42623 = CARTESIAN_POINT ( 'NONE',  ( -13.52853001603108574, -4.831407855809472629, -18.06453541021588194 ) ) ;
#42624 = FACE_OUTER_BOUND ( 'NONE', #26033, .T. ) ;
#42625 = CARTESIAN_POINT ( 'NONE',  ( 111.6155414775786596, 0.3778260857407392814, -12.04688916545883970 ) ) ;
#42626 = CARTESIAN_POINT ( 'NONE',  ( 111.9410827545248708, -6.936859964151250502, -8.388885654883777576 ) ) ;
#42627 = VERTEX_POINT ( 'NONE', #22596 ) ;
#42628 = CARTESIAN_POINT ( 'NONE',  ( 115.1220548109119761, -8.166667518702817929, -8.995218007635861213 ) ) ;
#42629 = CARTESIAN_POINT ( 'NONE',  ( 113.8740681442453138, 0.5811942927096154232, -14.16772938898807155 ) ) ;
#42630 = CARTESIAN_POINT ( 'NONE',  ( 88.28425963449632263, -11.60945497031996787, -13.24321520033830879 ) ) ;
#42631 = CARTESIAN_POINT ( 'NONE',  ( 118.9227414775786542, 0.4262465694468514643, -12.03445270309931736 ) ) ;
#42632 = CARTESIAN_POINT ( 'NONE',  ( 126.7702028005446238, -3.262292498975457367, -8.366245766736872369 ) ) ;
#42633 = CARTESIAN_POINT ( 'NONE',  ( 124.3117748109119844, -10.30919188438810075, -12.61870101168855918 ) ) ;
#42634 = DIRECTION ( 'NONE',  ( -0.8949343913984424415, -0.1703803081152067966, 0.4123869368673871993 ) ) ;
#42635 = DIRECTION ( 'NONE',  ( 0.9908103287288655414, -0.1352586133456837314, 0.000000000000000000 ) ) ;
#42636 = FACE_OUTER_BOUND ( 'NONE', #10134, .T. ) ;
#42637 = ORIENTED_EDGE ( 'NONE', *, *, #44678, .F. ) ;
#42638 = CARTESIAN_POINT ( 'NONE',  ( 116.4555358795247884, -8.402594152722688392, -9.854619843455216355 ) ) ;
#42639 = CARTESIAN_POINT ( 'NONE',  ( 121.7023481442452777, -9.261995988541697145, -16.69588392320189030 ) ) ;
#42640 = CARTESIAN_POINT ( 'NONE',  ( 63.42519601278144847, -3.154277804759124226, -19.11392337093018767 ) ) ;
#42641 = ORIENTED_EDGE ( 'NONE', *, *, #4454, .T. ) ;
#42642 = DIRECTION ( 'NONE',  ( 0.9609149988134837450, -0.1028163501681639419, 0.2570431154366518145 ) ) ;
#42643 = CARTESIAN_POINT ( 'NONE',  ( 112.5693548109119888, 0.4262465694468514643, -12.03445270309931736 ) ) ;
#42644 = CIRCLE ( 'NONE', #6224, 1.500000000000000000 ) ;
#42645 = CARTESIAN_POINT ( 'NONE',  ( 127.3669547543380958, -4.396327407923800834, -18.94794887702561681 ) ) ;
#42646 = CARTESIAN_POINT ( 'NONE',  ( 122.4397948109119767, -0.1624402480850797581, -16.17319339645315424 ) ) ;
#42647 = VERTEX_POINT ( 'NONE', #36496 ) ;
#42648 = CARTESIAN_POINT ( 'NONE',  ( 116.4834948109119779, -1.561330072975668504, -17.79121239304076951 ) ) ;
#42649 = FACE_OUTER_BOUND ( 'NONE', #10839, .T. ) ;
#42650 = CARTESIAN_POINT ( 'NONE',  ( 60.34146317132753978, -13.36775875599912844, -18.19321520033831519 ) ) ;
#42651 = FACE_OUTER_BOUND ( 'NONE', #28812, .T. ) ;
#42652 = CARTESIAN_POINT ( 'NONE',  ( 125.0492214775786266, -6.344957434206665248, -7.627207830600338134 ) ) ;
#42653 = ADVANCED_FACE ( 'NONE', ( #44037 ), #12801, .F. ) ;
#42654 = DIRECTION ( 'NONE',  ( 1.000000000000000000, 0.000000000000000000, -0.000000000000000000 ) ) ;
#42655 = CARTESIAN_POINT ( 'NONE',  ( 31.16203868753470019, 11.28474725185576055, -17.89321520033831447 ) ) ;
#42656 = CARTESIAN_POINT ( 'NONE',  ( 122.4965214775786251, -10.30919188438810075, -12.61870101168855918 ) ) ;
#42658 = CARTESIAN_POINT ( 'NONE',  ( 123.5743281442453139, -2.084020599724406786, -8.691656652584148546 ) ) ;
#42657 = CARTESIAN_POINT ( 'NONE',  ( 122.4397948109119767, -9.988377603198976828, -10.36322818467138340 ) ) ;
#42659 = CARTESIAN_POINT ( 'NONE',  ( 120.7852516859119731, -0.6942167230862511529, -9.935906262978006609 ) ) ;
#42660 = CARTESIAN_POINT ( 'NONE',  ( 125.0492214775786266, -3.505236298600246325, -18.68346056562440793 ) ) ;
#42661 = CARTESIAN_POINT ( 'NONE',  ( 113.4202548109119846, 0.1319031606808879209, -14.10382304977623669 ) ) ;
#42662 = CARTESIAN_POINT ( 'NONE',  ( 121.4754414775786131, -8.166667518702819706, -8.995218007635861213 ) ) ;
#42663 = EDGE_LOOP ( 'NONE', ( #43852, #14457, #25598, #31711 ) ) ;
#42664 = EDGE_CURVE ( 'NONE', #25132, #5495, #31772, .T. ) ;
#42665 = ORIENTED_EDGE ( 'NONE', *, *, #5645, .F. ) ;
#42666 = CARTESIAN_POINT ( 'NONE',  ( 117.7480986403692214, -1.196538596002806099, -17.02799684832026372 ) ) ;
#42667 = LINE ( 'NONE', #22137, #5276 ) ;
#42668 = CARTESIAN_POINT ( 'NONE',  ( 112.9828796295247884, -4.863998795839590272, -8.388885654883775800 ) ) ;
#42669 = CARTESIAN_POINT ( 'NONE',  ( 111.8716296295247901, -4.863998795839590272, -8.388885654883775800 ) ) ;
#42670 = CARTESIAN_POINT ( 'NONE',  ( 124.9357681442453156, -7.643976991953167044, -18.09477374809303285 ) ) ;
#42671 = CARTESIAN_POINT ( 'NONE',  ( 116.9940348109119839, -9.988377603198976828, -10.36322818467138340 ) ) ;
#42672 = VERTEX_POINT ( 'NONE', #8691 ) ;
#42673 = CARTESIAN_POINT ( 'NONE',  ( 111.6050014775786536, 0.1319031606808879209, -14.10382304977623669 ) ) ;
#42674 = CARTESIAN_POINT ( 'NONE',  ( 105.4819421295248247, 0.8980012041604618078, -13.39321520033831447 ) ) ;
#42675 = CARTESIAN_POINT ( 'NONE',  ( 119.0929214775786278, -4.153390946401311012, -8.397313243818187445 ) ) ;
#42676 = EDGE_CURVE ( 'NONE', #29882, #13861, #15309, .T. ) ;
#42677 = CARTESIAN_POINT ( 'NONE',  ( 88.73939138327467901, -25.38011337280982715, -14.88121679464376257 ) ) ;
#42678 = CARTESIAN_POINT ( 'NONE',  ( 123.0637881442452937, -8.899110576539703388, -16.42337572283491198 ) ) ;
#42680 = AXIS2_PLACEMENT_3D ( 'NONE', #1693, #29740, #32698 ) ;
#42679 = CARTESIAN_POINT ( 'NONE',  ( 70.19189222814998175, -70.61873396092025246, -41.45025657337532010 ) ) ;
#42681 = CARTESIAN_POINT ( 'NONE',  ( 116.4267681442453153, -3.383040157471821630, -19.15922257007629170 ) ) ;
#42682 = CARTESIAN_POINT ( 'NONE',  ( 115.4831921295247952, 0.8980012041604618078, -13.39321520033831447 ) ) ;
#42683 = CARTESIAN_POINT ( 'NONE',  ( 109.5102233795247884, -1.325403438956436419, -9.854619843455211026 ) ) ;
#42684 = VERTEX_POINT ( 'NONE', #5266 ) ;
#42685 = CARTESIAN_POINT ( 'NONE',  ( 96.21525317080913453, -28.02571811214721009, -13.67504067519043431 ) ) ;
#42686 = CARTESIAN_POINT ( 'NONE',  ( 119.5467348109119712, -5.574606645277164318, -18.38911715685844683 ) ) ;
#42687 = CARTESIAN_POINT ( 'NONE',  ( 115.4624148109119943, -5.638512984488999180, -18.83840828888717311 ) ) ;
#42688 = AXIS2_PLACEMENT_3D ( 'NONE', #21055, #306, #10803 ) ;
#42689 = CARTESIAN_POINT ( 'NONE',  ( 112.6828081442453282, -7.893985811506177619, -18.51759400769804742 ) ) ;
#42690 = CARTESIAN_POINT ( 'NONE',  ( 124.2550481442452792, -0.1624402480850797581, -16.17319339645315424 ) ) ;
#42691 = CARTESIAN_POINT ( 'NONE',  ( 119.6601881442453106, -1.833838273342659253, -17.42832698103878286 ) ) ;
#42692 = CARTESIAN_POINT ( 'NONE',  ( 114.4413348109119823, -0.8288870151387760510, -10.36305467784173118 ) ) ;
#42693 = ORIENTED_EDGE ( 'NONE', *, *, #203, .T. ) ;
#42694 = CARTESIAN_POINT ( 'NONE',  ( 123.0772048109119652, -2.527210466738041728, -8.967976844669124148 ) ) ;
#42695 = VECTOR ( 'NONE', #8301, 1000.000000000000000 ) ;
#42696 = CARTESIAN_POINT ( 'NONE',  ( 67.30914723170953096, -61.59348913822725535, -38.73469799600663777 ) ) ;
#42697 = CARTESIAN_POINT ( 'NONE',  ( 119.2631014775786298, -9.565557343593413364, -10.61323700422348004 ) ) ;
#42698 = VERTEX_POINT ( 'NONE', #29217 ) ;
#42699 = CARTESIAN_POINT ( 'NONE',  ( 117.2294421295247844, -4.863998795839590272, -13.39321520033831447 ) ) ;
#42700 = CARTESIAN_POINT ( 'NONE',  ( 115.6893214775786447, 0.5811942927096154232, -14.16772938898807155 ) ) ;
#42701 = CARTESIAN_POINT ( 'NONE',  ( 114.8581140045248361, -10.62599879583958717, -11.00651665394454604 ) ) ;
#42702 = CARTESIAN_POINT ( 'NONE',  ( 125.5597614775786326, -7.894159318335828068, -9.358103419637847864 ) ) ;
#42703 = CIRCLE ( 'NONE', #5550, 8.000000000000001776 ) ;
#42704 = ORIENTED_EDGE ( 'NONE', *, *, #34603, .F. ) ;
#42705 = ORIENTED_EDGE ( 'NONE', *, *, #18048, .T. ) ;
#42706 = CARTESIAN_POINT ( 'NONE',  ( 121.8725281442453223, -6.222761293078241884, -8.102969835052219238 ) ) ;
#42707 = CARTESIAN_POINT ( 'NONE',  ( 116.1998614775786507, 0.4262465694468514643, -12.03445270309931736 ) ) ;
#42708 = CARTESIAN_POINT ( 'NONE',  ( 124.5519021741527581, -9.864481698965258616, -13.30856797738673336 ) ) ;
#42709 = EDGE_CURVE ( 'NONE', #30504, #19352, #12132, .T. ) ;
#42710 = CIRCLE ( 'NONE', #28130, 8.000000000000001776 ) ;
#42711 = CARTESIAN_POINT ( 'NONE',  ( 122.6604860609119640, -6.564341423271550902, -7.887810678476487425 ) ) ;
#42712 = ORIENTED_EDGE ( 'NONE', *, *, #16411, .T. ) ;
#42713 = DIRECTION ( 'NONE',  ( 0.000000000000000000, 0.000000000000000000, -1.000000000000000000 ) ) ;
#42714 = CARTESIAN_POINT ( 'NONE',  ( 125.0302870206144945, -2.333779524057464361, -6.280435070964202282 ) ) ;
#42715 = CARTESIAN_POINT ( 'NONE',  ( 112.1494421295248003, 0.8980012041604618078, -13.39321520033831447 ) ) ;
#42716 = CARTESIAN_POINT ( 'NONE',  ( 112.3424481442453384, -6.344957434206662583, -7.627207830600332805 ) ) ;
#42717 = PRODUCT_DEFINITION_SHAPE ( 'NONE', 'NONE',  #45152 ) ;
#42718 = CARTESIAN_POINT ( 'NONE',  ( 125.3895814775786448, -2.084020599724406786, -8.691656652584148546 ) ) ;
#42719 = CARTESIAN_POINT ( 'NONE',  ( 119.6034614775786196, -3.505236298600246325, -18.68346056562440793 ) ) ;
#42720 = DIRECTION ( 'NONE',  ( -0.000000000000000000, 0.000000000000000000, 1.000000000000000000 ) ) ;
#42721 = EDGE_LOOP ( 'NONE', ( #13033, #1631, #2793, #27627, #41735, #29084 ) ) ;
#42722 = CARTESIAN_POINT ( 'NONE',  ( 118.1852948109119836, -4.153390946401325223, -8.397313243818185668 ) ) ;
#42723 = CARTESIAN_POINT ( 'NONE',  ( 119.7434548109119845, -1.178581368880148084, -9.878999011044413692 ) ) ;
#42724 = CARTESIAN_POINT ( 'NONE',  ( 75.95778847736514194, -3.256761025687008537, -14.39321520033831625 ) ) ;
#42725 = DIRECTION ( 'NONE',  ( 0.000000000000000000, -0.9242245927363028635, -0.3818493186865930533 ) ) ;
#42726 = EDGE_CURVE ( 'NONE', #511, #43799, #19182, .T. ) ;
#42727 = CIRCLE ( 'NONE', #41277, 5.500000000000001776 ) ;
#42728 = CARTESIAN_POINT ( 'NONE',  ( 116.7104014775786425, -0.4660016031367893996, -10.09054647747474043 ) ) ;
#42729 = ORIENTED_EDGE ( 'NONE', *, *, #22838, .T. ) ;
#42730 = CARTESIAN_POINT ( 'NONE',  ( 115.6325948109119821, 0.2603800115204892296, -16.42320221600525088 ) ) ;
#42731 = CARTESIAN_POINT ( 'NONE',  ( 114.3278814775786429, -10.30919188438809542, -12.61870101168854852 ) ) ;
#42732 = CARTESIAN_POINT ( 'NONE',  ( 112.2188952545247531, 0.8980012041604421569, -11.00651665394454071 ) ) ;
#42733 = CARTESIAN_POINT ( 'NONE',  ( 115.0086014775786509, -4.089484607189486809, -7.948022111789456723 ) ) ;
#42734 = CARTESIAN_POINT ( 'NONE',  ( 118.1285681442453068, -7.893985811506177619, -18.51759400769804742 ) ) ;
#42735 = CARTESIAN_POINT ( 'NONE',  ( 126.6211808763573998, -10.06551012219619778, -13.41462627083012293 ) ) ;
#42736 = CARTESIAN_POINT ( 'NONE',  ( 138.2184548109119930, -10.36826876090623450, -11.00511718064541178 ) ) ;
#42737 = CARTESIAN_POINT ( 'NONE',  ( 106.8710046295248759, -4.863998795839590272, -18.39754474579285315 ) ) ;
#42738 = VECTOR ( 'NONE', #33854, 1000.000000000000114 ) ;
#42739 = VERTEX_POINT ( 'NONE', #36938 ) ;
#42740 = CARTESIAN_POINT ( 'NONE',  ( 70.19189222814998175, -59.47700027789979060, -36.99360193826534271 ) ) ;
#42741 = CARTESIAN_POINT ( 'NONE',  ( 109.2294694551411141, -10.13459952827899357, -11.33384148904508493 ) ) ;
#42742 = CARTESIAN_POINT ( 'NONE',  ( 120.2274548109119934, -9.859900752359374465, -12.68260735090039404 ) ) ;
#42743 = CARTESIAN_POINT ( 'NONE',  ( 125.4584548109119737, -12.36944789948969614, -14.53642012792675509 ) ) ;
#42744 = CARTESIAN_POINT ( 'NONE',  ( 114.7192077545248594, -2.791137627527939813, -18.39754474579286025 ) ) ;
#42745 = CARTESIAN_POINT ( 'NONE',  ( 113.8163171295247764, 0.1403307496149613920, -13.39321520033831447 ) ) ;
#42746 = CARTESIAN_POINT ( 'NONE',  ( 126.3115243456352488, -4.515721963253167104, -8.358698628921043650 ) ) ;
#42747 = CARTESIAN_POINT ( 'NONE',  ( 114.1009748109119784, -5.574606645277164318, -18.38911715685844683 ) ) ;
#42748 = DIRECTION ( 'NONE',  ( 0.1352586133457954198, 0.9908103287288503314, 0.000000000000000000 ) ) ;
#42749 = CARTESIAN_POINT ( 'NONE',  ( 124.2550481442452792, -9.988377603198980381, -10.36322818467138518 ) ) ;
#42750 = B_SPLINE_CURVE_WITH_KNOTS ( 'NONE', 3,
 ( #38262, #21170, #24159, #415, #13889, #2945, #14332, #27580, #7255, #3610 ),
 .UNSPECIFIED., .F., .F.,
 ( 4, 3, 3, 4 ),
 ( 0.000000000000000000, 0.0001671877560958130043, 0.0003343755126086585196, 0.0006438490228507220145 ),
 .UNSPECIFIED. ) ;
#42751 = CARTESIAN_POINT ( 'NONE',  ( 120.5678148109119832, -8.166667518702819706, -8.995218007635861213 ) ) ;
#42752 = EDGE_LOOP ( 'NONE', ( #34141, #41384, #34865, #13744 ) ) ;
#42753 = AXIS2_PLACEMENT_3D ( 'NONE', #9112, #19370, #33260 ) ;
#42754 = CARTESIAN_POINT ( 'NONE',  ( 118.0151148109119816, 0.4262465694468514643, -12.03445270309931736 ) ) ;
#42755 = CARTESIAN_POINT ( 'NONE',  ( 112.1155414775786454, 0.9020085738987339008, -11.91225656197089222 ) ) ;
#42756 = CARTESIAN_POINT ( 'NONE',  ( 119.3198281442452924, 0.5811942927096110934, -14.16772938898807510 ) ) ;
#42757 = CARTESIAN_POINT ( 'NONE',  ( 120.9649014775786355, -6.222761293078241884, -8.102969835052219238 ) ) ;
#42758 = VERTEX_POINT ( 'NONE', #23052 ) ;
#42759 = CARTESIAN_POINT ( 'NONE',  ( 124.8790414775786246, -8.899110576539710493, -16.42337572283490132 ) ) ;
#42760 = CARTESIAN_POINT ( 'NONE',  ( 119.5467348109119712, -4.089484607189486809, -7.948022111789456723 ) ) ;
#42761 = CARTESIAN_POINT ( 'NONE',  ( 137.3173478096594806, 0.3375151974989685777, -13.37218143070558263 ) ) ;
#42762 = AXIS2_PLACEMENT_3D ( 'NONE', #36284, #22389, #43141 ) ;
#42763 = CARTESIAN_POINT ( 'NONE',  ( 109.6491296295247793, -4.863998795839590272, -19.15521520033831493 ) ) ;
#42764 = DIRECTION ( 'NONE',  ( -0.7871354856660202071, 0.6167752151498580027, 0.002461946824133919541 ) ) ;
#42765 = DIRECTION ( 'NONE',  ( 0.000000000000000000, 0.000000000000000000, 1.000000000000000000 ) ) ;
#42766 = CONICAL_SURFACE ( 'NONE', #27475, 2.445500000000004448, 0.9599310885968757034 ) ;
#42767 = CARTESIAN_POINT ( 'NONE',  ( 113.1912390045248031, -9.868328341294098749, -11.32035403202665869 ) ) ;
#42768 = CARTESIAN_POINT ( 'NONE',  ( 118.2987481442453088, -1.561330072975668504, -17.79121239304076951 ) ) ;
#42769 = CARTESIAN_POINT ( 'NONE',  ( 136.2315975805985317, -10.25943272008531792, -11.12509562936944896 ) ) ;
#42770 = CARTESIAN_POINT ( 'NONE',  ( 117.0507614775786465, 0.1319031606808879209, -14.10382304977623669 ) ) ;
#42771 = CARTESIAN_POINT ( 'NONE',  ( 126.2597653975769134, -0.7068999842200600625, -10.57775600701587493 ) ) ;
#42772 = CARTESIAN_POINT ( 'NONE',  ( 117.6747548109119776, -7.643976991954101408, -18.09477374809246797 ) ) ;
#42773 = CARTESIAN_POINT ( 'NONE',  ( 111.2465515045248168, -6.936859964151250502, -18.39754474579286025 ) ) ;
#42774 = PRESENTATION_LAYER_ASSIGNMENT (  '', '', ( #7091 ) ) ;
#42775 = CARTESIAN_POINT ( 'NONE',  ( 115.2922348109119781, -10.63000616557721756, -14.87417383870574206 ) ) ;
#42776 = DIRECTION ( 'NONE',  ( -1.000000000000000000, 0.000000000000000000, 0.000000000000000000 ) ) ;
#42777 = CARTESIAN_POINT ( 'NONE',  ( 123.8370331944929035, -1.036737761566197014, -17.24079555149560861 ) ) ;
#42779 = CARTESIAN_POINT ( 'NONE',  ( 118.3554748109119998, 0.2603800115204892296, -16.42320221600525088 ) ) ;
#42778 = CARTESIAN_POINT ( 'NONE',  ( 61.65126288137282273, -14.46472726967718181, -8.900850585800878179 ) ) ;
#42780 = EDGE_CURVE ( 'NONE', #37342, #39008, #19864, .T. ) ;
#42781 = CARTESIAN_POINT ( 'NONE',  ( 118.5256548109119876, -8.899110576539710493, -16.42337572283490132 ) ) ;
#42782 = CARTESIAN_POINT ( 'NONE',  ( 113.8173414775786512, -9.565557343593413364, -10.61323700422348004 ) ) ;
#42783 = VERTEX_POINT ( 'NONE', #29438 ) ;
#42784 = LINE ( 'NONE', #39354, #5665 ) ;
#42785 = CARTESIAN_POINT ( 'NONE',  ( 123.8579614775786126, 0.5811942927096110934, -14.16772938898807510 ) ) ;
#42786 = CARTESIAN_POINT ( 'NONE',  ( 112.8439733795247832, -1.325403438956436419, -9.854619843455211026 ) ) ;
#42787 = CARTESIAN_POINT ( 'NONE',  ( 119.2631014775786298, -9.565557343593413364, -10.61323700422348004 ) ) ;
#42788 = CARTESIAN_POINT ( 'NONE',  ( 116.7104014775786425, -8.899110576539710493, -16.42337572283490132 ) ) ;
#42789 = CARTESIAN_POINT ( 'NONE',  ( 84.86020291624612355, -29.99489077589588959, -12.39321520033834645 ) ) ;
#42790 = CARTESIAN_POINT ( 'NONE',  ( 109.1629577545248395, -7.250697342233347165, -7.631215200338321125 ) ) ;
#42791 = CARTESIAN_POINT ( 'NONE',  ( 122.6099748109119929, -0.8288870151387760510, -10.36305467784173118 ) ) ;
#42792 = CARTESIAN_POINT ( 'NONE',  ( 122.7234281442452755, -4.153390946401325223, -8.397313243818185668 ) ) ;
#42793 = DIRECTION ( 'NONE',  ( 0.000000000000000000, 0.6004852223388321697, -0.7996358532186279566 ) ) ;
#42794 = CARTESIAN_POINT ( 'NONE',  ( 109.2294421281825407, -4.894246902762260376, -7.815410045176730769 ) ) ;
#42795 = CARTESIAN_POINT ( 'NONE',  ( 122.1743141859119817, -8.321307733199551748, -9.223433127585318303 ) ) ;
#42796 = VECTOR ( 'NONE', #26568, 999.9999999999998863 ) ;
#42797 = CARTESIAN_POINT ( 'NONE',  ( 106.5237390045248418, -9.868328341294098749, -11.32035403202665869 ) ) ;
#42798 = CARTESIAN_POINT ( 'NONE',  ( 116.7565503026016813, -4.863998795840742240, -18.55532337341522364 ) ) ;
#42799 = CARTESIAN_POINT ( 'NONE',  ( 83.39219417991402850, -33.04367333191778755, -22.35815310413347845 ) ) ;
#42800 = CARTESIAN_POINT ( 'NONE',  ( 116.9940348109119839, -9.988377603198976828, -10.36322818467138340 ) ) ;
#42801 = CARTESIAN_POINT ( 'NONE',  ( 120.1140014775786398, -1.561330072975668504, -17.79121239304076951 ) ) ;
#42802 = CARTESIAN_POINT ( 'NONE',  ( 109.6491296295247793, -4.863998795839590272, -19.15521520033831493 ) ) ;
#42803 = CARTESIAN_POINT ( 'NONE',  ( 70.19189222814998175, -51.68868231262963775, -33.87830190084585524 ) ) ;
#42804 = ORIENTED_EDGE ( 'NONE', *, *, #31525, .T. ) ;
#42805 = CARTESIAN_POINT ( 'NONE',  ( 117.0306702067644409, -1.223627541775731631, -16.99192386690444323 ) ) ;
#42806 = CARTESIAN_POINT ( 'NONE',  ( 117.7314814775786260, -4.089484607189486809, -7.948022111789456723 ) ) ;
#42807 = CARTESIAN_POINT ( 'NONE',  ( 123.7445081442452874, -7.894159318335828068, -9.358103419637847864 ) ) ;
#42808 = DIRECTION ( 'NONE',  ( 0.000000000000000000, 0.000000000000000000, 1.000000000000000000 ) ) ;
#42809 = CARTESIAN_POINT ( 'NONE',  ( 125.1626748109119802, -9.988377603198980381, -10.36322818467138518 ) ) ;
#42810 = CARTESIAN_POINT ( 'NONE',  ( 121.4754414775786131, -8.166667518702819706, -8.995218007635861213 ) ) ;
#42811 = CARTESIAN_POINT ( 'NONE',  ( 112.8439733795247832, -8.938348069036489818, -17.46756447353520159 ) ) ;
#42812 = CARTESIAN_POINT ( 'NONE',  ( 115.4056881442453459, -2.084020599724406786, -8.691656652584148546 ) ) ;
#42813 = CARTESIAN_POINT ( 'NONE',  ( 120.7852516859119731, -9.665098340737509730, -17.37397104707595474 ) ) ;
#42814 = DIRECTION ( 'NONE',  ( -0.000000000000000000, -0.9284778069183721172, -0.3713878862591650232 ) ) ;
#42815 = VERTEX_POINT ( 'NONE', #26480 ) ;
#42816 = CARTESIAN_POINT ( 'NONE',  ( 119.1878298109119783, -7.200787124940443817, -17.81845355600750835 ) ) ;
#42817 = CARTESIAN_POINT ( 'NONE',  ( 120.9649014775786355, -3.383040157471821630, -19.15922257007629170 ) ) ;
#42818 = ORIENTED_EDGE ( 'NONE', *, *, #33534, .F. ) ;
#42819 = CARTESIAN_POINT ( 'NONE',  ( 71.02242295334774269, -55.05296798929726521, -38.32881209277477552 ) ) ;
#42820 = DIRECTION ( 'NONE',  ( -0.3127730236694426513, 0.9498278979187093629, 0.000000000000000000 ) ) ;
#42822 = CARTESIAN_POINT ( 'NONE',  ( 70.19189222814998175, -55.19510675323109439, -35.28085945431567438 ) ) ;
#42821 = AXIS2_PLACEMENT_3D ( 'NONE', #22694, #30219, #9022 ) ;
#42823 = CARTESIAN_POINT ( 'NONE',  ( 116.8805814775786445, -3.505236298600246325, -18.68346056562440793 ) ) ;
#42824 = CARTESIAN_POINT ( 'NONE',  ( 66.03584176102988579, -0.1449045395527848445, -16.39321520033830737 ) ) ;
#42825 = CARTESIAN_POINT ( 'NONE',  ( 64.01282776924010420, -34.86145050234441811, -5.893215200338315363 ) ) ;
#42826 = CARTESIAN_POINT ( 'NONE',  ( 123.8579614775786126, -9.859900752359378018, -12.68260735090039759 ) ) ;
#42827 = CARTESIAN_POINT ( 'NONE',  ( 88.35093386163799778, -25.99489077589524300, -13.39321520033831447 ) ) ;
#42828 = CARTESIAN_POINT ( 'NONE',  ( 123.2339681442453241, -3.505236298600246325, -18.68346056562440793 ) ) ;
#42829 = CARTESIAN_POINT ( 'NONE',  ( 125.3296504289671844, -11.36836562817265950, -10.49722269535554098 ) ) ;
#42830 = CARTESIAN_POINT ( 'NONE',  ( 121.8158014775786171, -4.153390946401325223, -8.397313243818185668 ) ) ;
#42831 = CARTESIAN_POINT ( 'NONE',  ( 112.9664414775786412, 0.5811942927096154232, -14.16772938898807155 ) ) ;
#42832 = CARTESIAN_POINT ( 'NONE',  ( 119.1496481442453046, -3.383040157471821630, -19.15922257007629170 ) ) ;
#42833 = CARTESIAN_POINT ( 'NONE',  ( 112.0020881442453344, 0.2603800115204892296, -16.42320221600525088 ) ) ;
#42834 = LINE ( 'NONE', #24823, #29996 ) ;
#42835 = CARTESIAN_POINT ( 'NONE',  ( 121.5888948109119809, 0.1319031606808879209, -14.10382304977623669 ) ) ;
#42836 = ORIENTED_EDGE ( 'NONE', *, *, #44562, .T. ) ;
#42837 = CARTESIAN_POINT ( 'NONE',  ( 121.9292548109119849, -1.561330072975668948, -17.79121239304076951 ) ) ;
#42838 = CARTESIAN_POINT ( 'NONE',  ( 113.2606921295247702, -9.868328341294093420, -13.39321520033831447 ) ) ;
#42839 = ADVANCED_FACE ( 'NONE', ( #40385, #37851 ), #23743, .F. ) ;
#42840 = CARTESIAN_POINT ( 'NONE',  ( 74.66232006577804725, -2.500611837642884527, -18.79321520033831661 ) ) ;
#42841 = CARTESIAN_POINT ( 'NONE',  ( 114.5547881442453217, -4.153390946401321671, -8.397313243818183892 ) ) ;
#42842 = CARTESIAN_POINT ( 'NONE',  ( 119.8823610609119754, -3.163656168406935087, -18.89861972220014508 ) ) ;
#42843 = CARTESIAN_POINT ( 'NONE',  ( 116.5944421295247793, -9.868328341294093420, -13.39321520033831447 ) ) ;
#42844 = B_SPLINE_CURVE_WITH_KNOTS ( 'NONE', 3,
 ( #14949, #31816, #28411, #363, #35907, #588, #42320, #42544, #7417, #14498 ),
 .UNSPECIFIED., .F., .F.,
 ( 4, 3, 3, 4 ),
 ( 0.000000000000000000, 0.0002476486447138875262, 0.0004952972925464160315, 0.0009604418836934749786 ),
 .UNSPECIFIED. ) ;
#42845 = EDGE_LOOP ( 'NONE', ( #41021, #22315, #3589, #25797, #29604 ) ) ;
#42846 = CARTESIAN_POINT ( 'NONE',  ( 122.9503348109119827, -9.859900752359378018, -12.68260735090039759 ) ) ;
#42847 = DIRECTION ( 'NONE',  ( 1.000000000000000000, 0.000000000000000000, 0.000000000000000000 ) ) ;
#42848 = CARTESIAN_POINT ( 'NONE',  ( 63.48709602856936129, -14.78504216833964335, -18.40560711939649252 ) ) ;
#42849 = FACE_OUTER_BOUND ( 'NONE', #29458, .T. ) ;
#42850 = ADVANCED_FACE ( 'NONE', ( #44942 ), #6625, .T. ) ;
#42851 = CARTESIAN_POINT ( 'NONE',  ( 108.1211608795247798, -1.325403438956436419, -16.93181055722141792 ) ) ;
#42852 = ORIENTED_EDGE ( 'NONE', *, *, #27906, .T. ) ;
#42853 = CARTESIAN_POINT ( 'NONE',  ( 114.1577014775786552, -6.344957434206662583, -7.627207830600332805 ) ) ;
#42854 = CARTESIAN_POINT ( 'NONE',  ( 88.66111334384352460, -11.22778238082202407, -14.05973504337623581 ) ) ;
#42855 = CARTESIAN_POINT ( 'NONE',  ( 120.9649014775786355, -6.222761293078241884, -8.102969835052219238 ) ) ;
#42856 = CARTESIAN_POINT ( 'NONE',  ( 112.6260814775786514, -0.8288870151387760510, -10.36305467784173118 ) ) ;
#42857 = DIRECTION ( 'NONE',  ( -0.000000000000000000, -0.9284778069183718952, -0.3713878862591649677 ) ) ;
#42858 = CYLINDRICAL_SURFACE ( 'NONE', #9222, 3.000000000000001776 ) ;
#42859 = LINE ( 'NONE', #32357, #13557 ) ;
#42860 =( NAMED_UNIT ( * ) PLANE_ANGLE_UNIT ( ) SI_UNIT ( $, .RADIAN. ) );
#42861 = EDGE_LOOP ( 'NONE', ( #40787, #3867, #38067, #3896, #24881, #3253, #44924, #21607, #9633, #27663, #30324, #31031, #39529 ) ) ;
#42862 = CARTESIAN_POINT ( 'NONE',  ( 116.9417077545247992, -2.791137627527939813, -18.39754474579286025 ) ) ;
#42863 = CARTESIAN_POINT ( 'NONE',  ( 119.0361948109119652, -7.893985811506177619, -18.51759400769804742 ) ) ;
#42864 = CARTESIAN_POINT ( 'NONE',  ( 66.07631794059973629, -2.141239331173074856, -18.04181533358571343 ) ) ;
#42865 = ORIENTED_EDGE ( 'NONE', *, *, #27960, .T. ) ;
#42866 = EDGE_CURVE ( 'NONE', #18085, #24134, #13025, .T. ) ;
#42867 = CARTESIAN_POINT ( 'NONE',  ( 70.19189222814998175, -61.69445140165969121, -37.88057465812982372 ) ) ;
#42868 = EDGE_CURVE ( 'NONE', #6119, #31347, #42727, .T. ) ;
#42869 = ADVANCED_FACE ( 'NONE', ( #33978 ), #3199, .F. ) ;
#42870 = CARTESIAN_POINT ( 'NONE',  ( 112.0588148109119828, -9.859900752359374465, -12.68260735090039404 ) ) ;
#42871 = DIRECTION ( 'NONE',  ( 0.000000000000000000, 0.000000000000000000, -1.000000000000000000 ) ) ;
#42872 = CARTESIAN_POINT ( 'NONE',  ( 122.7801548109119665, -6.222761293078241884, -8.102969835052219238 ) ) ;
#42873 = ORIENTED_EDGE ( 'NONE', *, *, #40798, .F. ) ;
#42874 = CARTESIAN_POINT ( 'NONE',  ( 118.5823814775786360, -1.834011780172310813, -8.268836392978581529 ) ) ;
#42875 = LINE ( 'NONE', #38990, #19646 ) ;
#42876 = CARTESIAN_POINT ( 'NONE',  ( 120.1332064091100733, -0.9924539043446216624, -17.29976612834909133 ) ) ;
#42877 = DIRECTION ( 'NONE',  ( 0.9999995469159187467, 0.0009519285464175227711, 0.000000000000000000 ) ) ;
#42878 = CARTESIAN_POINT ( 'NONE',  ( 112.2857214775786474, -5.574606645277164318, -18.38911715685844683 ) ) ;
#42879 = DIRECTION ( 'NONE',  ( -0.9063289528979890930, -0.4225728684367167087, 0.000000000000000000 ) ) ;
#42880 = VECTOR ( 'NONE', #30511, 1000.000000000000000 ) ;
#42881 = CARTESIAN_POINT ( 'NONE',  ( 80.91184012100937650, -3.933054092416038650, -19.39321520033831447 ) ) ;
#42882 = CARTESIAN_POINT ( 'NONE',  ( 125.9568481442452850, -6.344957434206665248, -7.627207830600338134 ) ) ;
#42883 = CARTESIAN_POINT ( 'NONE',  ( 126.2972081442452890, -2.084020599724406786, -8.691656652584148546 ) ) ;
#42884 = CARTESIAN_POINT ( 'NONE',  ( 116.7523363153857048, -5.088870560009469024, -18.55110938619918670 ) ) ;
#42885 = CARTESIAN_POINT ( 'NONE',  ( 124.9357681442453014, -7.643976991954077427, -18.09477374809248928 ) ) ;
#42886 = CARTESIAN_POINT ( 'NONE',  ( 77.25325688895158294, -4.012910213732562070, -9.893215200338316251 ) ) ;
#42887 = CARTESIAN_POINT ( 'NONE',  ( 118.6391081442452986, -4.089484607189486809, -7.948022111789456723 ) ) ;
#42888 = ORIENTED_EDGE ( 'NONE', *, *, #26138, .T. ) ;
#42889 = CARTESIAN_POINT ( 'NONE',  ( 126.2184548109092361, -8.793414587017092998, -16.48721015983629457 ) ) ;
#42890 = LINE ( 'NONE', #21908, #24937 ) ;
#42891 = EDGE_CURVE ( 'NONE', #12393, #35460, #18400, .T. ) ;
#42892 = CARTESIAN_POINT ( 'NONE',  ( 114.9275671295247889, 0.1403307496149613920, -13.39321520033831447 ) ) ;
#42893 = CARTESIAN_POINT ( 'NONE',  ( 113.8163171295247764, 0.1403307496149613920, -13.39321520033831447 ) ) ;
#42894 = CARTESIAN_POINT ( 'NONE',  ( 125.5030348109119842, -6.222761293079280165, -8.102969835052485692 ) ) ;
#42895 = CARTESIAN_POINT ( 'NONE',  ( 113.9875214775786532, -0.4660016031367893996, -10.09054647747474043 ) ) ;
#42896 = ORIENTED_EDGE ( 'NONE', *, *, #38409, .F. ) ;
#42897 = CARTESIAN_POINT ( 'NONE',  ( 111.6617281442453304, 0.4262465694468514643, -12.03445270309931736 ) ) ;
#42898 = DIRECTION ( 'NONE',  ( -0.000000000000000000, -0.9284778069183721172, -0.3713878862591650232 ) ) ;
#42899 = CARTESIAN_POINT ( 'NONE',  ( 80.91184012100937650, -3.933054092416038650, -10.89321520033831447 ) ) ;
#42900 = CARTESIAN_POINT ( 'NONE',  ( 126.1270281442452870, -10.30919188438810075, -12.61870101168855918 ) ) ;
#42901 = CARTESIAN_POINT ( 'NONE',  ( 109.2295480519286883, -0.08797490772791666247, -15.21102469340631558 ) ) ;
#42902 = DIRECTION ( 'NONE',  ( 1.387778780781445676E-17, -0.9284778069183720062, -0.3713878862591650232 ) ) ;
#42903 = CARTESIAN_POINT ( 'NONE',  ( 115.7460481442453357, 0.9020085738987339008, -11.91225656197089222 ) ) ;
#42904 = ADVANCED_FACE ( 'NONE', ( #38075 ), #3425, .F. ) ;
#42905 = CARTESIAN_POINT ( 'NONE',  ( 110.2047546295247855, -4.863998795839590272, -7.631215200338315796 ) ) ;
#42906 = CARTESIAN_POINT ( 'NONE',  ( 110.1353015045248469, -6.936859964151250502, -18.39754474579286025 ) ) ;
#42907 = VERTEX_POINT ( 'NONE', #2518 ) ;
#42908 = CARTESIAN_POINT ( 'NONE',  ( 126.2872529661375438, -7.630682474280415128, -9.187169839767605595 ) ) ;
#42909 = CARTESIAN_POINT ( 'NONE',  ( 120.7379948109119709, 0.4262465694468514643, -12.03445270309931736 ) ) ;
#42910 = CARTESIAN_POINT ( 'NONE',  ( 116.9373081442452929, -8.166667518702817929, -8.995218007635861213 ) ) ;
#42911 = CARTESIAN_POINT ( 'NONE',  ( 112.0588148109119828, 0.5811942927096154232, -14.16772938898807155 ) ) ;
#42912 = CARTESIAN_POINT ( 'NONE',  ( 124.3117748109119844, 0.1319031606808879209, -14.10382304977623669 ) ) ;
#42913 = PRODUCT_DEFINITION_CONTEXT ( 'detailed design', #33198, 'design' ) ;
#42914 = CARTESIAN_POINT ( 'NONE',  ( 124.7655881442452852, -9.859900752359378018, -12.68260735090039759 ) ) ;
#42915 = CARTESIAN_POINT ( 'NONE',  ( 114.1577014775786552, -3.505236298600246325, -18.68346056562440793 ) ) ;
#42916 = ORIENTED_EDGE ( 'NONE', *, *, #15908, .T. ) ;
#42917 = CARTESIAN_POINT ( 'NONE',  ( 120.7157985609119635, -10.36940331770106916, -15.09355782777062061 ) ) ;
#42918 = CARTESIAN_POINT ( 'NONE',  ( 65.41257106814472877, -15.47412461924279725, -10.39321520033831625 ) ) ;
#42919 = CARTESIAN_POINT ( 'NONE',  ( 118.2420214775786320, -6.222761293078241884, -8.102969835052219238 ) ) ;
#42920 = ORIENTED_EDGE ( 'NONE', *, *, #8365, .F. ) ;
#42921 = AXIS2_PLACEMENT_3D ( 'NONE', #1437, #25626, #8516 ) ;
#42922 = DIRECTION ( 'NONE',  ( 1.000000000000000000, 0.000000000000000000, 0.000000000000000000 ) ) ;
#42923 = ADVANCED_FACE ( 'NONE', ( #2746 ), #16943, .T. ) ;
#42924 = CARTESIAN_POINT ( 'NONE',  ( 116.4834948109119779, -1.561330072975668504, -17.79121239304076951 ) ) ;
#42925 = CARTESIAN_POINT ( 'NONE',  ( 107.9128015045248219, -6.936859964151250502, -18.39754474579286025 ) ) ;
#42926 = DIRECTION ( 'NONE',  ( 0.000000000000000000, 0.000000000000000000, -1.000000000000000000 ) ) ;
#42927 = EDGE_LOOP ( 'NONE', ( #28521, #8005, #39724, #1292 ) ) ;
#42928 = ORIENTED_EDGE ( 'NONE', *, *, #28009, .T. ) ;
#42929 = CARTESIAN_POINT ( 'NONE',  ( 120.9081748109119872, -4.153390946401325223, -8.397313243818185668 ) ) ;
#42930 = CARTESIAN_POINT ( 'NONE',  ( 117.7314814775786260, -5.574606645277164318, -18.38911715685844683 ) ) ;
#42931 = EDGE_CURVE ( 'NONE', #33919, #20193, #12983, .T. ) ;
#42932 = CARTESIAN_POINT ( 'NONE',  ( 124.5737018702985779, -9.836393355957630646, -13.94123563784690667 ) ) ;
#42933 = LINE ( 'NONE', #24478, #25705 ) ;
#42934 = ORIENTED_EDGE ( 'NONE', *, *, #34011, .T. ) ;
#42935 = FACE_OUTER_BOUND ( 'NONE', #21685, .T. ) ;
#42936 = CARTESIAN_POINT ( 'NONE',  ( 62.35495919926018615, -65.08422123914256474, -45.30333471292594538 ) ) ;
#42937 = CARTESIAN_POINT ( 'NONE',  ( 110.2742077545248094, -7.250697342233347165, -7.631215200338321125 ) ) ;
#42938 = CARTESIAN_POINT ( 'NONE',  ( 116.7671281442453335, -1.834011780172310813, -8.268836392978581529 ) ) ;
#42939 = CARTESIAN_POINT ( 'NONE',  ( 112.2857214775786474, -4.089484607189486809, -7.948022111789456723 ) ) ;
#42940 = CARTESIAN_POINT ( 'NONE',  ( 122.2696148109119889, -5.574606645277164318, -18.38911715685844683 ) ) ;
#42941 = CARTESIAN_POINT ( 'NONE',  ( 60.45894907855898026, -4.846173528048905332, -19.39321520033831447 ) ) ;
#42942 = ORIENTED_EDGE ( 'NONE', *, *, #31338, .F. ) ;
#42943 = CARTESIAN_POINT ( 'NONE',  ( 119.7736414775786358, 0.1319031606808879209, -14.10382304977623669 ) ) ;
#42944 = CARTESIAN_POINT ( 'NONE',  ( 115.8999108795247821, -8.938348069036489818, -9.318865927141430916 ) ) ;
#42945 = CARTESIAN_POINT ( 'NONE',  ( 114.3024890045248156, 0.8980012041604421569, -15.77991374673208469 ) ) ;
#42946 = CARTESIAN_POINT ( 'NONE',  ( 118.2420214775786320, -3.383040157471821630, -19.15922257007629170 ) ) ;
#42947 = ORIENTED_EDGE ( 'NONE', *, *, #34508, .F. ) ;
#42948 = CARTESIAN_POINT ( 'NONE',  ( 116.4834948109119779, -1.561330072975668504, -17.79121239304076951 ) ) ;
#42949 = CARTESIAN_POINT ( 'NONE',  ( 62.70685217410979106, -37.48166990149824329, -5.152479539365462990 ) ) ;
#42950 = CARTESIAN_POINT ( 'NONE',  ( 105.5513952545248060, 0.8980012041604421569, -11.00651665394454071 ) ) ;
#42951 = CARTESIAN_POINT ( 'NONE',  ( 115.0653281442453277, -6.344957434206662583, -7.627207830600332805 ) ) ;
#42952 = CARTESIAN_POINT ( 'NONE',  ( 118.2420214775786320, -3.383040157471821630, -19.15922257007629170 ) ) ;
#42953 = CARTESIAN_POINT ( 'NONE',  ( 107.2294421295247844, -9.051693226400931991, -21.39321520033831447 ) ) ;
#42954 = DIRECTION ( 'NONE',  ( 0.000000000000000000, 0.000000000000000000, -1.000000000000000000 ) ) ;
#42955 = ORIENTED_EDGE ( 'NONE', *, *, #37861, .T. ) ;
#42956 = CARTESIAN_POINT ( 'NONE',  ( 121.9092173576684957, -6.302457937304696500, -18.83702152638931082 ) ) ;
#42957 = CARTESIAN_POINT ( 'NONE',  ( 109.2294422178231201, -10.02089344363390744, -11.03051820906416403 ) ) ;
#42958 = CARTESIAN_POINT ( 'NONE',  ( 121.6456214775786293, 0.4262465694468514643, -12.03445270309931736 ) ) ;
#42959 = CARTESIAN_POINT ( 'NONE',  ( 113.7468640045248236, 0.1403307496149616695, -15.46607636864997204 ) ) ;
#42960 = CARTESIAN_POINT ( 'NONE',  ( 106.0375671295248310, -10.62599879583958540, -13.39321520033831447 ) ) ;
#42961 = AXIS2_PLACEMENT_3D ( 'NONE', #29254, #4403, #35628 ) ;
#42962 = CARTESIAN_POINT ( 'NONE',  ( 115.5191414775786569, -6.222761293078241884, -8.102969835052219238 ) ) ;
#42963 = CARTESIAN_POINT ( 'NONE',  ( 117.2294421295247844, 1.035107641088057973, -5.059859068394715109 ) ) ;
#42964 = CARTESIAN_POINT ( 'NONE',  ( 124.5954081442453116, -3.383040157471821630, -19.15922257007629170 ) ) ;
#42965 = CARTESIAN_POINT ( 'NONE',  ( 121.3619881442452879, -4.089484607189486809, -7.948022111789456723 ) ) ;
#42967 = ORIENTED_EDGE ( 'NONE', *, *, #3275, .T. ) ;
#42966 = EDGE_CURVE ( 'NONE', #41162, #9931, #19413, .T. ) ;
#42968 = CARTESIAN_POINT ( 'NONE',  ( 117.7314814775786260, -5.574606645277164318, -18.38911715685844683 ) ) ;
#42969 = DIRECTION ( 'NONE',  ( 0.000000000000000000, 0.000000000000000000, 1.000000000000000000 ) ) ;
#42970 = CARTESIAN_POINT ( 'NONE',  ( 120.0005481442453146, -5.638512984488999180, -18.83840828888717311 ) ) ;
#42971 = CARTESIAN_POINT ( 'NONE',  ( 119.7736414775786358, 0.1319031606808879209, -14.10382304977623669 ) ) ;
#42972 = ORIENTED_EDGE ( 'NONE', *, *, #19438, .F. ) ;
#42973 = DIRECTION ( 'NONE',  ( 1.000000000000000000, 0.000000000000000000, -0.000000000000000000 ) ) ;
#42974 = CARTESIAN_POINT ( 'NONE',  ( 119.2063748109119814, -1.561330072975668504, -17.79121239304076951 ) ) ;
#42975 = EDGE_CURVE ( 'NONE', #9906, #523, #6337, .T. ) ;
#42976 = CARTESIAN_POINT ( 'NONE',  ( 112.6260814775786514, -0.8288870151387760510, -10.36305467784173118 ) ) ;
#42977 = EDGE_CURVE ( 'NONE', #6307, #35850, #18803, .T. ) ;
#42978 = DIRECTION ( 'NONE',  ( 0.7697712484781088493, -0.6383198453882299450, 0.000000000000000000 ) ) ;
#42979 = CARTESIAN_POINT ( 'NONE',  ( 126.2184548109119788, 0.08617673920515746266, -14.09731900820182915 ) ) ;
#42980 = CARTESIAN_POINT ( 'NONE',  ( 115.0664733795247798, -1.325403438956436419, -9.854619843455211026 ) ) ;
#42981 = CIRCLE ( 'NONE', #17502, 2.999999999999999556 ) ;
#42982 = CARTESIAN_POINT ( 'NONE',  ( 119.3198281442452924, 0.5811942927096110934, -14.16772938898807510 ) ) ;
#42983 = VECTOR ( 'NONE', #10310, 1000.000000000000000 ) ;
#42984 = LINE ( 'NONE', #11751, #6211 ) ;
#42985 = CARTESIAN_POINT ( 'NONE',  ( 114.6115148109119986, -6.222761293078241884, -8.102969835052219238 ) ) ;
#42986 = CARTESIAN_POINT ( 'NONE',  ( 125.6732148109119862, 0.5811942927096110934, -14.16772938898807510 ) ) ;
#42987 = CARTESIAN_POINT ( 'NONE',  ( 126.3509913981939405, -0.5655071077596977025, -10.71139246774309051 ) ) ;
#42988 = CARTESIAN_POINT ( 'NONE',  ( 117.5045748109119756, -9.859900752359374465, -12.68260735090039404 ) ) ;
#42989 = CARTESIAN_POINT ( 'NONE',  ( 109.4407702545248355, 0.1403307496149616695, -11.32035403202665336 ) ) ;
#42990 = CARTESIAN_POINT ( 'NONE',  ( 114.1577014775786552, -3.505236298600246325, -18.68346056562440793 ) ) ;
#42991 = DIRECTION ( 'NONE',  ( 1.000000000000000000, 0.000000000000000000, -0.000000000000000000 ) ) ;
#42992 = CARTESIAN_POINT ( 'NONE',  ( 71.02242295334774269, -51.33905676162378739, -36.84326054773811876 ) ) ;
#42994 = CARTESIAN_POINT ( 'NONE',  ( 120.8514481442452961, -7.893985811506177619, -18.51759400769804742 ) ) ;
#42993 = CARTESIAN_POINT ( 'NONE',  ( 63.13932362937020315, -14.69787538488875533, -9.650383735752717129 ) ) ;
#42995 = CARTESIAN_POINT ( 'NONE',  ( 121.4187148109119789, -3.505236298600246325, -18.68346056562440793 ) ) ;
#42996 = VERTEX_POINT ( 'NONE', #13098 ) ;
#42997 = CARTESIAN_POINT ( 'NONE',  ( 136.8340972670087297, -7.132904381023736917, -8.303565050146163529 ) ) ;
#42998 = CARTESIAN_POINT ( 'NONE',  ( 125.2194014775786286, -10.30919188438810075, -12.61870101168855918 ) ) ;
#42999 = CARTESIAN_POINT ( 'NONE',  ( 111.8716296295247901, -4.863998795839590272, -8.388885654883775800 ) ) ;
#43000 = CARTESIAN_POINT ( 'NONE',  ( 120.8514481442452961, -2.084020599724406786, -8.691656652584148546 ) ) ;
#43001 = CARTESIAN_POINT ( 'NONE',  ( 122.6667014775786413, -2.084020599724406786, -8.691656652584148546 ) ) ;
#43002 = CARTESIAN_POINT ( 'NONE',  ( 115.2355081442453155, 0.1319031606808879209, -14.10382304977623669 ) ) ;
#43003 = CARTESIAN_POINT ( 'NONE',  ( 85.50018718514893123, -28.44542656748122056, -9.229114258165695972 ) ) ;
#43004 = CARTESIAN_POINT ( 'NONE',  ( 108.2600671295247992, -10.62599879583958540, -13.39321520033831447 ) ) ;
#43005 = CARTESIAN_POINT ( 'NONE',  ( 123.8579614775786126, -9.859900752359378018, -12.68260735090039759 ) ) ;
#43006 = CARTESIAN_POINT ( 'NONE',  ( 124.8223148109119762, -10.15424416112533912, -14.75197769757731336 ) ) ;
#43007 = CARTESIAN_POINT ( 'NONE',  ( 67.84197459855160162, -62.01099631431865333, -38.73636453584316541 ) ) ;
#43008 = AXIS2_PLACEMENT_3D ( 'NONE', #11450, #35815, #32177 ) ;
#43009 = DIRECTION ( 'NONE',  ( -0.000000000000000000, -0.9284778069183718952, -0.3713878862591649677 ) ) ;
#43010 = CARTESIAN_POINT ( 'NONE',  ( 123.2855641859119942, -0.8832429491016019485, -18.19431474523657855 ) ) ;
#43011 = CARTESIAN_POINT ( 'NONE',  ( 113.9552233795247815, -8.938348069036489818, -17.46756447353520159 ) ) ;
#43012 = DIRECTION ( 'NONE',  ( 0.7202110682883375858, 0.2576522076061144029, -0.6441361323747234469 ) ) ;
#43013 = CARTESIAN_POINT ( 'NONE',  ( 83.86207143271133191, -31.76334952037468540, -22.85450806870273865 ) ) ;
#43014 = CARTESIAN_POINT ( 'NONE',  ( 118.1852948109119836, -5.638512984488999180, -18.83840828888717311 ) ) ;
#43015 = CARTESIAN_POINT ( 'NONE',  ( 116.8805814775786445, -6.344957434206662583, -7.627207830600332805 ) ) ;
#43016 = CARTESIAN_POINT ( 'NONE',  ( 108.6073327545248048, -2.477300249445798297, -19.15521520033831138 ) ) ;
#43017 = CARTESIAN_POINT ( 'NONE',  ( 86.09323753712084226, -25.38011337280982715, -14.88121679464376257 ) ) ;
#43018 = CARTESIAN_POINT ( 'NONE',  ( 67.30914723170953096, -51.38023326212514519, -34.64943124715581035 ) ) ;
#43019 = ORIENTED_EDGE ( 'NONE', *, *, #15556, .F. ) ;
#43020 = CARTESIAN_POINT ( 'NONE',  ( 112.3759981608379803, 0.3867979994853637526, -14.64321520033830026 ) ) ;
#43021 = CIRCLE ( 'NONE', #5156, 1.610000000000000986 ) ;
#43022 = CARTESIAN_POINT ( 'NONE',  ( 118.2420214775786320, -3.383040157471821630, -19.15922257007629170 ) ) ;
#43023 = CARTESIAN_POINT ( 'NONE',  ( 125.9568481442452850, -3.505236298600246325, -18.68346056562440793 ) ) ;
#43024 = DIRECTION ( 'NONE',  ( 1.000000000000000000, 0.000000000000000000, 0.000000000000000000 ) ) ;
#43025 = VECTOR ( 'NONE', #31153, 1000.000000000000000 ) ;
#43026 = CARTESIAN_POINT ( 'NONE',  ( 115.2922348109119781, 0.4262465694468514643, -12.03445270309931736 ) ) ;
#43027 = CARTESIAN_POINT ( 'NONE',  ( 121.4187148109119789, -6.344957434206665248, -7.627207830600338134 ) ) ;
#43028 = CARTESIAN_POINT ( 'NONE',  ( 114.7192077545248594, -7.250697342233347165, -7.631215200338321125 ) ) ;
#43029 = ADVANCED_FACE ( 'NONE', ( #9221 ), #30642, .T. ) ;
#43030 = CARTESIAN_POINT ( 'NONE',  ( 117.1642148109119859, -0.8288870151387760510, -10.36305467784173118 ) ) ;
#43031 = CARTESIAN_POINT ( 'NONE',  ( 116.8221226705892803, -1.747798139657595673, -17.59079367583192166 ) ) ;
#43032 = CARTESIAN_POINT ( 'NONE',  ( 117.2294421295247844, 0.6306099254434621715, -14.64321520033831447 ) ) ;
#43033 = ORIENTED_EDGE ( 'NONE', *, *, #30872, .T. ) ;
#43034 = CARTESIAN_POINT ( 'NONE',  ( 120.9936110609119737, -6.340755971794695078, -8.611740276972781771 ) ) ;
#43035 = CARTESIAN_POINT ( 'NONE',  ( 118.5823814775786360, -1.834011780172310813, -8.268836392978581529 ) ) ;
#43036 = ORIENTED_EDGE ( 'NONE', *, *, #39042, .F. ) ;
#43037 = CARTESIAN_POINT ( 'NONE',  ( 76.69189222814998175, -45.49566950204133065, -7.393215200338315363 ) ) ;
#43038 = CARTESIAN_POINT ( 'NONE',  ( -13.67905184926989826, -4.633292466094534490, -7.903589911137905766 ) ) ;
#43039 = AXIS2_PLACEMENT_3D ( 'NONE', #39865, #9080, #35976 ) ;
#43040 = CARTESIAN_POINT ( 'NONE',  ( 125.0849635773846842, -2.467220198597905867, -17.83387418641800437 ) ) ;
#43041 = CARTESIAN_POINT ( 'NONE',  ( 119.7736414775786358, 0.1319031606808879209, -14.10382304977623669 ) ) ;
#43042 = CARTESIAN_POINT ( 'NONE',  ( 67.90996757083897251, -0.5187677644655397380, -16.39321520033831447 ) ) ;
#43043 = CARTESIAN_POINT ( 'NONE',  ( 123.9601326669217372, -2.334846009198419559, -18.01015021110789505 ) ) ;
#43044 = CARTESIAN_POINT ( 'NONE',  ( 122.6667014775786413, -2.084020599724406786, -8.691656652584148546 ) ) ;
#43045 = CARTESIAN_POINT ( 'NONE',  ( 121.3619881442452879, -4.089484607189477039, -7.948022111789462052 ) ) ;
#43046 = CARTESIAN_POINT ( 'NONE',  ( 123.4041481442452834, 0.1319031606808879209, -14.10382304977623669 ) ) ;
#43047 = VECTOR ( 'NONE', #5326, 1000.000000000000000 ) ;
#43048 = CARTESIAN_POINT ( 'NONE',  ( 125.2014504115533668, -11.57818613074989855, -16.36145069722488898 ) ) ;
#43049 = CARTESIAN_POINT ( 'NONE',  ( 119.2631014775786298, -9.565557343593413364, -10.61323700422348004 ) ) ;
#43050 = CARTESIAN_POINT ( 'NONE',  ( 123.0070614775786169, -10.15424416112533912, -14.75197769757731336 ) ) ;
#43051 = VECTOR ( 'NONE', #22324, 1000.000000000000227 ) ;
#43052 = CARTESIAN_POINT ( 'NONE',  ( 112.0020881442453344, 0.2603800115204892296, -16.42320221600525088 ) ) ;
#43053 = CARTESIAN_POINT ( 'NONE',  ( 120.4543614775786295, -4.089484607189486809, -7.948022111789456723 ) ) ;
#43054 = CARTESIAN_POINT ( 'NONE',  ( 114.5547881442453217, -5.638512984488999180, -18.83840828888717311 ) ) ;
#43055 = CARTESIAN_POINT ( 'NONE',  ( 121.4551560953690483, -6.001247023715324147, -18.26661038929047010 ) ) ;
#43056 = CARTESIAN_POINT ( 'NONE',  ( 125.1626748109119802, -0.1624402480850797581, -16.17319339645315424 ) ) ;
#43057 = EDGE_LOOP ( 'NONE', ( #23965, #44852, #29380, #11854 ) ) ;
#43058 = CARTESIAN_POINT ( 'NONE',  ( 118.9227414775786400, -10.63000616557722466, -14.87417383870573495 ) ) ;
#43059 = CARTESIAN_POINT ( 'NONE',  ( 111.0381921295247878, -9.868328341294093420, -13.39321520033831447 ) ) ;
#43060 = CARTESIAN_POINT ( 'NONE',  ( 112.4272546295247821, -4.863998795839590272, -18.39754474579285315 ) ) ;
#43061 = CARTESIAN_POINT ( 'NONE',  ( 83.46705746533213244, -32.83968548964498524, -23.89321520033831803 ) ) ;
#43062 = CARTESIAN_POINT ( 'NONE',  ( 114.2711548109119803, -0.1624402480850797581, -16.17319339645315424 ) ) ;
#43063 = DIRECTION ( 'NONE',  ( 0.000000000000000000, -1.000000000000000000, 0.000000000000000000 ) ) ;
#43064 = CARTESIAN_POINT ( 'NONE',  ( 124.6521348109119884, -1.561330072975668948, -17.79121239304076951 ) ) ;
#43065 = ORIENTED_EDGE ( 'NONE', *, *, #1924, .F. ) ;
#43066 = CARTESIAN_POINT ( 'NONE',  ( 120.2841814775786276, -10.15424416112533912, -14.75197769757731336 ) ) ;
#43067 = CARTESIAN_POINT ( 'NONE',  ( 120.0907204359119760, 1.345710702986147034, -13.97328579221134426 ) ) ;
#43068 = CARTESIAN_POINT ( 'NONE',  ( 120.1601735609119856, 0.6414057260225851653, -11.69287257290600657 ) ) ;
#43069 = CARTESIAN_POINT ( 'NONE',  ( 124.0588908503701475, -8.552676153439012552, -17.65880394779906837 ) ) ;
#43070 = CARTESIAN_POINT ( 'NONE',  ( 109.0935046295247872, -4.863998795839590272, -18.39754474579285315 ) ) ;
#43071 = ORIENTED_EDGE ( 'NONE', *, *, #27820, .T. ) ;
#43072 = CARTESIAN_POINT ( 'NONE',  ( 116.4267681442453153, -3.383040157471821630, -19.15922257007629170 ) ) ;
#43073 = CARTESIAN_POINT ( 'NONE',  ( 125.3328548109119964, -9.261995988541697145, -16.69588392320189030 ) ) ;
#43074 = AXIS2_PLACEMENT_3D ( 'NONE', #39256, #8022, #21710 ) ;
#43075 = CARTESIAN_POINT ( 'NONE',  ( 119.7169148109119874, -0.1624402480850797581, -16.17319339645315424 ) ) ;
#43076 = CARTESIAN_POINT ( 'NONE',  ( 126.4599182912938318, -3.568828463829896602, -8.438959581207143401 ) ) ;
#43077 = CARTESIAN_POINT ( 'NONE',  ( 111.2751814775786556, -7.618532446445550832, -18.05174138884716228 ) ) ;
#43078 =( BOUNDED_CURVE ( )  B_SPLINE_CURVE ( 2, ( #9972, #40750, #36626, #33650, #5401, #9507, #40986, #27065, #40525, #9740, #13163, #9058, #26609, #23193, #44399, #20229, #5846 ),
 .UNSPECIFIED., .F., .T. ) 
 B_SPLINE_CURVE_WITH_KNOTS ( ( 3, 2, 2, 2, 2, 2, 2, 2, 3 ),
 ( 0.2040431156034945015, 0.2124999999999999944, 0.2250000000000000056, 0.2374999999999999889, 0.2500000000000000000, 0.2625000000000000111, 0.2750000000000000222, 0.2874999999999999778, 0.2959568843965054707 ),
 .UNSPECIFIED. ) 
 CURVE ( )  GEOMETRIC_REPRESENTATION_ITEM ( )  RATIONAL_B_SPLINE_CURVE ( ( 0.9666851417651740608, 0.9485006404992000206, 1.000000000000000000, 0.9238795325112869605, 1.000000000000000000, 0.9238795325112869605, 1.000000000000000000, 0.9238795325112869605, 1.000000000000000000, 0.9238795325112869605, 1.000000000000000000, 0.9238795325112869605, 1.000000000000000000, 0.9238795325112869605, 1.000000000000000000, 0.9485006404991980222, 0.9666851417651760592 ) ) 
 REPRESENTATION_ITEM ( '' )  );
#43079 = DIRECTION ( 'NONE',  ( 0.000000000000000000, 0.000000000000000000, 1.000000000000000000 ) ) ;
#43080 = FACE_OUTER_BOUND ( 'NONE', #41719, .T. ) ;
#43081 = ORIENTED_EDGE ( 'NONE', *, *, #29924, .T. ) ;
#43082 = CARTESIAN_POINT ( 'NONE',  ( 114.6497546295247929, -4.863998795839590272, -18.39754474579285315 ) ) ;
#43083 = VECTOR ( 'NONE', #2565, 1000.000000000000000 ) ;
#43084 = CARTESIAN_POINT ( 'NONE',  ( 121.1918081442452859, 0.9020085738987339008, -11.91225656197089222 ) ) ;
#43085 = CARTESIAN_POINT ( 'NONE',  ( 60.53937939559665438, -4.256997083809236138, -19.39321520033831447 ) ) ;
#43086 = ORIENTED_EDGE ( 'NONE', *, *, #39235, .F. ) ;
#43087 = CARTESIAN_POINT ( 'NONE',  ( 115.3489614775786407, -9.261995988541697145, -16.69588392320189030 ) ) ;
#43088 = CARTESIAN_POINT ( 'NONE',  ( 111.4348214775786801, -3.505236298600246325, -18.68346056562440793 ) ) ;
#43089 = COLOUR_RGB ( '',0.7921568627450980005, 0.8196078431372548767, 0.9333333333333333481 ) ;
#43090 = CARTESIAN_POINT ( 'NONE',  ( 110.8992858795247827, -8.402594152722736354, -9.854619843455244776 ) ) ;
#43091 = CARTESIAN_POINT ( 'NONE',  ( 124.0848681442452772, -5.574606645277164318, -18.38911715685844683 ) ) ;
#43092 = ORIENTED_EDGE ( 'NONE', *, *, #9672, .T. ) ;
#43093 = CARTESIAN_POINT ( 'NONE',  ( 117.5045748109119756, 0.5811942927096110934, -14.16772938898807510 ) ) ;
#43094 = FACE_OUTER_BOUND ( 'NONE', #22135, .T. ) ;
#43095 = DIRECTION ( 'NONE',  ( 0.3445294493088594256, 0.9387755102040817867, 0.000000000000000000 ) ) ;
#43096 = CARTESIAN_POINT ( 'NONE',  ( 115.3001676093651753, 0.5600166689815611054, -14.64321520033831447 ) ) ;
#43097 = CARTESIAN_POINT ( 'NONE',  ( 137.2865145795249475, -4.931349962157201006, -8.163486744682481699 ) ) ;
#43098 = CARTESIAN_POINT ( 'NONE',  ( 112.9097148109120070, -9.565557343593413364, -10.61323700422348004 ) ) ;
#43099 = DIRECTION ( 'NONE',  ( -1.000000000000000000, 0.000000000000000000, 0.000000000000000000 ) ) ;
#43100 = VECTOR ( 'NONE', #17790, 999.9999999999998863 ) ;
#43101 = CARTESIAN_POINT ( 'NONE',  ( 125.3184118084099623, -3.219979270944925087, -20.33414543254830420 ) ) ;
#43102 = CARTESIAN_POINT ( 'NONE',  ( 111.7184548109119788, -0.8288870151387760510, -10.36305467784173118 ) ) ;
#43103 = CARTESIAN_POINT ( 'NONE',  ( 112.6828081442453282, -7.893985811506177619, -18.51759400769804742 ) ) ;
#43104 = CARTESIAN_POINT ( 'NONE',  ( 116.6277022568074102, -9.657689035024059621, -14.93094152719381107 ) ) ;
#43105 = CARTESIAN_POINT ( 'NONE',  ( 124.3685014775786328, 0.4262465694468514643, -12.03445270309931736 ) ) ;
#43106 = PLANE ( 'NONE',  #21133 ) ;
#43107 = CARTESIAN_POINT ( 'NONE',  ( 119.4332814775786318, -0.4660016031367893996, -10.09054647747474043 ) ) ;
#43108 = ORIENTED_EDGE ( 'NONE', *, *, #33926, .T. ) ;
#43109 = CARTESIAN_POINT ( 'NONE',  ( 126.3444272079807007, -8.643527312879829338, -16.76218589705026574 ) ) ;
#43110 = CARTESIAN_POINT ( 'NONE',  ( 114.6497546295247929, -4.863998795839590272, -7.631215200338315796 ) ) ;
#43111 = CARTESIAN_POINT ( 'NONE',  ( 112.0799890045248475, -9.868328341294098749, -11.32035403202665869 ) ) ;
#43112 = CARTESIAN_POINT ( 'NONE',  ( 110.4825671295247815, 0.1403307496149613920, -13.39321520033831447 ) ) ;
#43113 = CARTESIAN_POINT ( 'NONE',  ( 126.3999550322252361, -9.807393774667220399, -12.17702641686377873 ) ) ;
#43114 = CARTESIAN_POINT ( 'NONE',  ( 114.7249681442453237, 0.2603800115204892296, -16.42320221600525088 ) ) ;
#43115 = ORIENTED_EDGE ( 'NONE', *, *, #23468, .F. ) ;
#43116 = CARTESIAN_POINT ( 'NONE',  ( 117.0507614775786465, 0.1319031606808879209, -14.10382304977623669 ) ) ;
#43117 = CARTESIAN_POINT ( 'NONE',  ( 108.6767858795247861, -0.7896495226426338832, -17.46756447353520159 ) ) ;
#43118 = CARTESIAN_POINT ( 'NONE',  ( 151.2860562277021472, -2.211393927326563702, -15.67656524173425758 ) ) ;
#43119 = LINE ( 'NONE', #28770, #39295 ) ;
#43120 = ADVANCED_FACE ( 'NONE', ( #44559 ), #16973, .F. ) ;
#43121 = CARTESIAN_POINT ( 'NONE',  ( 122.4040527111058339, -1.267766418764731728, -16.93314635290706605 ) ) ;
#43122 = CARTESIAN_POINT ( 'NONE',  ( 112.2289948109119848, -1.834011780172310813, -8.268836392978581529 ) ) ;
#43123 = CARTESIAN_POINT ( 'NONE',  ( 116.7104014775786425, -0.4660016031367893996, -10.09054647747474043 ) ) ;
#43124 = CARTESIAN_POINT ( 'NONE',  ( 112.4272546295247821, -4.863998795839590272, -7.631215200338315796 ) ) ;
#43125 = CARTESIAN_POINT ( 'NONE',  ( 112.0799890045248475, -9.868328341294098749, -11.32035403202665869 ) ) ;
#43126 = ORIENTED_EDGE ( 'NONE', *, *, #29888, .F. ) ;
#43127 = DIRECTION ( 'NONE',  ( -0.9063289528979876497, -0.4225728684367200394, 0.000000000000000000 ) ) ;
#43128 = CARTESIAN_POINT ( 'NONE',  ( 118.6391081442452986, -5.574606645277164318, -18.38911715685844683 ) ) ;
#43129 = CARTESIAN_POINT ( 'NONE',  ( 114.8951481442453115, -0.4660016031367893996, -10.09054647747474043 ) ) ;
#43130 = FACE_OUTER_BOUND ( 'NONE', #27894, .T. ) ;
#43131 = CARTESIAN_POINT ( 'NONE',  ( 117.9132914748722385, -0.1020945015694949415, -15.74893487844865625 ) ) ;
#43132 = CARTESIAN_POINT ( 'NONE',  ( 122.4965214775786251, 0.1319031606808879209, -14.10382304977623669 ) ) ;
#43133 = CARTESIAN_POINT ( 'NONE',  ( 115.6325948109119821, -9.565557343593413364, -10.61323700422348004 ) ) ;
#43134 = EDGE_LOOP ( 'NONE', ( #7242, #21498, #10260, #18237 ) ) ;
#43135 = CIRCLE ( 'NONE', #25656, 1.199999999999999512 ) ;
#43136 = CARTESIAN_POINT ( 'NONE',  ( 123.0077516859119839, -0.6942167230862511529, -9.935906262978006609 ) ) ;
#43137 = VECTOR ( 'NONE', #3898, 1000.000000000000000 ) ;
#43138 = DIRECTION ( 'NONE',  ( 0.000000000000000000, 0.9284778069183718952, 0.3713878862591650232 ) ) ;
#43139 = CARTESIAN_POINT ( 'NONE',  ( 119.4900081442453086, -7.643976991954077427, -18.09477374809248928 ) ) ;
#43140 = VERTEX_POINT ( 'NONE', #10133 ) ;
#43141 = DIRECTION ( 'NONE',  ( 0.8636456077245089347, -0.5040994586965589219, 0.000000000000000000 ) ) ;
#43142 = CARTESIAN_POINT ( 'NONE',  ( 113.5337081442453240, -9.261995988541697145, -16.69588392320189030 ) ) ;
#43143 = CARTESIAN_POINT ( 'NONE',  ( 116.5249890045247980, 0.8980012041604421569, -15.77991374673208469 ) ) ;
#43144 = CARTESIAN_POINT ( 'NONE',  ( 113.7606148109119886, -7.894159318335828068, -9.358103419637847864 ) ) ;
#43145 = EDGE_CURVE ( 'NONE', #6217, #29655, #19507, .T. ) ;
#43146 = ORIENTED_EDGE ( 'NONE', *, *, #42866, .F. ) ;
#43147 = AXIS2_PLACEMENT_3D ( 'NONE', #4287, #1098, #11595 ) ;
#43148 = ORIENTED_EDGE ( 'NONE', *, *, #13618, .T. ) ;
#43149 = CARTESIAN_POINT ( 'NONE',  ( 122.6667014775786413, -2.084020599724406786, -8.691656652584148546 ) ) ;
#43150 = CARTESIAN_POINT ( 'NONE',  ( 116.9373081442452929, -1.833838273342659253, -17.42832698103878286 ) ) ;
#43151 = DIRECTION ( 'NONE',  ( 0.000000000000000000, 0.3818493186865928868, -0.9242245927363027524 ) ) ;
#43152 = ADVANCED_FACE ( 'NONE', ( #9438 ), #26997, .T. ) ;
#43153 = ORIENTED_EDGE ( 'NONE', *, *, #2472, .F. ) ;
#43154 = LINE ( 'NONE', #8498, #25944 ) ;
#43155 = FACE_OUTER_BOUND ( 'NONE', #30280, .T. ) ;
#43156 = EDGE_CURVE ( 'NONE', #41325, #10999, #25251, .T. ) ;
#43157 = CARTESIAN_POINT ( 'NONE',  ( 111.4549108795247747, -8.938348069036489818, -9.318865927141430916 ) ) ;
#43158 =( BOUNDED_CURVE ( )  B_SPLINE_CURVE ( 2, ( #1520, #1970, #36174, #26150, #12026, #19536, #12256, #36844, #18855, #29347, #43707, #15441, #5613, #40518, #5839, #29796, #26378 ),
 .UNSPECIFIED., .F., .T. ) 
 B_SPLINE_CURVE_WITH_KNOTS ( ( 3, 2, 2, 2, 2, 2, 2, 2, 3 ),
 ( 0.5035091206787219997, 0.5124999999999999556, 0.5250000000000000222, 0.5374999999999999778, 0.5500000000000000444, 0.5625000000000000000, 0.5749999999999999556, 0.5875000000000000222, 0.5964908793212779781 ),
 .UNSPECIFIED. ) 
 CURVE ( )  GEOMETRIC_REPRESENTATION_ITEM ( )  RATIONAL_B_SPLINE_CURVE ( ( 0.9692594319298230010, 0.9452488050343759163, 1.000000000000000000, 0.9238795325112869605, 1.000000000000000000, 0.9238795325112869605, 1.000000000000000000, 0.9238795325112869605, 1.000000000000000000, 0.9238795325112869605, 1.000000000000000000, 0.9238795325112869605, 1.000000000000000000, 0.9238795325112869605, 1.000000000000000000, 0.9452488050343769155, 0.9692594319298230010 ) ) 
 REPRESENTATION_ITEM ( '' )  );
#43159 = CARTESIAN_POINT ( 'NONE',  ( 117.8449348109119938, -8.166667518702817929, -8.995218007635861213 ) ) ;
#43161 = CARTESIAN_POINT ( 'NONE',  ( 117.0507614775786465, 0.1319031606808879209, -14.10382304977623669 ) ) ;
#43160 = CARTESIAN_POINT ( 'NONE',  ( 111.7751814775786556, -7.893985811506177619, -18.51759400769804742 ) ) ;
#43162 = CARTESIAN_POINT ( 'NONE',  ( 123.0637881442452937, -8.899110576539710493, -16.42337572283490132 ) ) ;
#43163 = DIRECTION ( 'NONE',  ( -1.000000000000000000, 0.000000000000000000, 0.000000000000000000 ) ) ;
#43164 = ORIENTED_EDGE ( 'NONE', *, *, #11932, .F. ) ;
#43165 = CARTESIAN_POINT ( 'NONE',  ( 118.9227414775786542, 0.4262465694468514643, -12.03445270309931736 ) ) ;
#43166 = EDGE_CURVE ( 'NONE', #36261, #41199, #44111, .T. ) ;
#43167 = CARTESIAN_POINT ( 'NONE',  ( 123.6877814775786533, -6.222761293078241884, -8.102969835052219238 ) ) ;
#43168 = CARTESIAN_POINT ( 'NONE',  ( 111.4549108795247747, -8.938348069036489818, -9.318865927141430916 ) ) ;
#43169 = AXIS2_PLACEMENT_3D ( 'NONE', #5140, #19056, #32942 ) ;
#43170 = CARTESIAN_POINT ( 'NONE',  ( 116.1082702545247827, 0.1403307496149616695, -11.32035403202665336 ) ) ;
#43171 = CARTESIAN_POINT ( 'NONE',  ( 113.3301452545248083, 0.8980012041604421569, -11.00651665394454071 ) ) ;
#43172 = CARTESIAN_POINT ( 'NONE',  ( 118.4689281442453392, 0.9020085738987339008, -11.91225656197089222 ) ) ;
#43173 = ORIENTED_EDGE ( 'NONE', *, *, #17225, .T. ) ;
#43174 = EDGE_CURVE ( 'NONE', #20751, #39978, #23805, .T. ) ;
#43175 = CARTESIAN_POINT ( 'NONE',  ( 121.8158014775786171, -5.638512984488999180, -18.83840828888717311 ) ) ;
#43176 = CARTESIAN_POINT ( 'NONE',  ( 115.2581675888224169, -2.372251574601226043, -17.96033910819752322 ) ) ;
#43177 = DIRECTION ( 'NONE',  ( -0.000000000000000000, -0.9284778069183721172, -0.3713878862591650232 ) ) ;
#43178 = CARTESIAN_POINT ( 'NONE',  ( 117.6747548109119919, -1.834011780172310813, -8.268836392978581529 ) ) ;
#43179 = EDGE_CURVE ( 'NONE', #34025, #2916, #22773, .T. ) ;
#43180 = ADVANCED_FACE ( 'NONE', ( #40458 ), #18701, .T. ) ;
#43181 = CARTESIAN_POINT ( 'NONE',  ( 119.1496481442453046, -3.383040157471821630, -19.15922257007629170 ) ) ;
#43182 =( GEOMETRIC_REPRESENTATION_CONTEXT ( 3 ) GLOBAL_UNCERTAINTY_ASSIGNED_CONTEXT ( ( #24680 ) ) GLOBAL_UNIT_ASSIGNED_CONTEXT ( ( #30518, #30073, #13207 ) ) REPRESENTATION_CONTEXT ( 'NONE', 'WORKASPACE' ) );
#43183 = CARTESIAN_POINT ( 'NONE',  ( 62.47183387988239645, -3.518612362980701125, -19.22720551556120228 ) ) ;
#43184 = CARTESIAN_POINT ( 'NONE',  ( 116.9384279471258878, -11.58292435961694089, -5.930349853556944772 ) ) ;
#43185 = VERTEX_POINT ( 'NONE', #23130 ) ;
#43186 = AXIS2_PLACEMENT_3D ( 'NONE', #29293, #12657, #8767 ) ;
#43187 = CARTESIAN_POINT ( 'NONE',  ( 123.2184548109119788, -6.965697074025154478, -10.59448971407311646 ) ) ;
#43188 = CARTESIAN_POINT ( 'NONE',  ( 73.07463722459043254, -62.21038723923624048, -37.19243930338672754 ) ) ;
#43189 = CARTESIAN_POINT ( 'NONE',  ( 119.5467348109119712, -5.574606645277164318, -18.38911715685844683 ) ) ;
#43190 = CARTESIAN_POINT ( 'NONE',  ( 113.6079577545248043, -2.791137627527939813, -18.39754474579286025 ) ) ;
#43191 = CARTESIAN_POINT ( 'NONE',  ( 105.7597546295248350, -4.863998795839590272, -7.631215200338315796 ) ) ;
#43192 = CARTESIAN_POINT ( 'NONE',  ( 113.7606148109119886, -7.894159318335828068, -9.358103419637847864 ) ) ;
#43193 = CARTESIAN_POINT ( 'NONE',  ( 123.7253032127138397, -2.191907684172563986, -18.20049396185734025 ) ) ;
#43194 = CARTESIAN_POINT ( 'NONE',  ( 114.2144281442453178, -1.833838273342658809, -17.42832698103878286 ) ) ;
#43195 = CARTESIAN_POINT ( 'NONE',  ( 118.1852948109119836, -5.638512984488999180, -18.83840828888717311 ) ) ;
#43196 = EDGE_LOOP ( 'NONE', ( #11763, #15541, #36002, #969 ) ) ;
#43197 = CARTESIAN_POINT ( 'NONE',  ( 117.6747548109119919, -7.643976991954077427, -18.09477374809248928 ) ) ;
#43198 = CARTESIAN_POINT ( 'NONE',  ( 114.5547881442453217, -5.638512984488999180, -18.83840828888717311 ) ) ;
#43199 = CARTESIAN_POINT ( 'NONE',  ( 121.5321681442453183, -9.988377603198976828, -10.36322818467138340 ) ) ;
#43200 = CARTESIAN_POINT ( 'NONE',  ( 121.4754414775786131, -1.833838273342659697, -17.42832698103878286 ) ) ;
#43201 = ORIENTED_EDGE ( 'NONE', *, *, #24599, .F. ) ;
#43202 = CARTESIAN_POINT ( 'NONE',  ( 124.1415948109119540, -3.505236298600246325, -18.68346056562440793 ) ) ;
#43203 = AXIS2_PLACEMENT_3D ( 'NONE', #19357, #22327, #19580 ) ;
#43204 = CARTESIAN_POINT ( 'NONE',  ( 122.1561614775786353, -0.4660016031367893996, -10.09054647747474043 ) ) ;
#43205 = CARTESIAN_POINT ( 'NONE',  ( 124.9542645564588526, -8.185087495464536289, -6.532584163191488713 ) ) ;
#43206 = CARTESIAN_POINT ( 'NONE',  ( 121.8725281442453223, -3.383040157471821630, -19.15922257007629170 ) ) ;
#43207 = CARTESIAN_POINT ( 'NONE',  ( 85.82015659721905365, -25.23119213852205789, -15.24166438581092109 ) ) ;
#43208 = CARTESIAN_POINT ( 'NONE',  ( 127.8473378044042477, -3.224434522777662515, -14.32704208324133255 ) ) ;
#43209 = CARTESIAN_POINT ( 'NONE',  ( 112.6356140045247827, 0.1403307496149616695, -15.46607636864997204 ) ) ;
#43210 = CIRCLE ( 'NONE', #3879, 2.541999999999999371 ) ;
#43211 = CARTESIAN_POINT ( 'NONE',  ( 94.20708369096698220, -25.99489077589524300, -13.39321520033831447 ) ) ;
#43212 = CARTESIAN_POINT ( 'NONE',  ( 75.95778847736514194, -3.256761025687008537, -7.147228641687434880 ) ) ;
#43213 = CARTESIAN_POINT ( 'NONE',  ( 115.4056881442453459, -2.084020599724406786, -8.691656652584148546 ) ) ;
#43214 = CARTESIAN_POINT ( 'NONE',  ( 112.1155414775786454, -10.15424416112533912, -14.75197769757731336 ) ) ;
#43215 = CARTESIAN_POINT ( 'NONE',  ( 64.37417719139408234, -13.02885965268791324, -15.64938273518901291 ) ) ;
#43216 = DIRECTION ( 'NONE',  ( 0.1352586133457950590, 0.9908103287288504424, 1.214306433183764177E-14 ) ) ;
#43217 = CARTESIAN_POINT ( 'NONE',  ( 108.8851452545248151, -9.868328341294098749, -15.46607636864997204 ) ) ;
#43218 = CARTESIAN_POINT ( 'NONE',  ( 115.8027748109119841, -8.899110576539710493, -16.42337572283490132 ) ) ;
#43219 = DIRECTION ( 'NONE',  ( 0.000000000000000000, 0.3818493186865927203, -0.9242245927363029745 ) ) ;
#43220 = EDGE_CURVE ( 'NONE', #1042, #43595, #9231, .T. ) ;
#43221 = CARTESIAN_POINT ( 'NONE',  ( 78.69189222814998175, -49.76310523276723785, -24.89321520033831447 ) ) ;
#43223 = CARTESIAN_POINT ( 'NONE',  ( 120.5678148109119832, -8.166667518702819706, -8.995218007635861213 ) ) ;
#43222 = CARTESIAN_POINT ( 'NONE',  ( 65.34866896724287244, -14.13234089959629536, -9.463491280356649327 ) ) ;
#43224 = CARTESIAN_POINT ( 'NONE',  ( 121.7590748109119687, -2.084020599724406786, -8.691656652584148546 ) ) ;
#43225 = ORIENTED_EDGE ( 'NONE', *, *, #40636, .T. ) ;
#43226 = CARTESIAN_POINT ( 'NONE',  ( 114.8360934012278847, 0.04929351793716424401, -14.64321520033828783 ) ) ;
#43227 = CARTESIAN_POINT ( 'NONE',  ( 125.0492214775786266, -6.344957434206665248, -7.627207830600338134 ) ) ;
#43228 = CARTESIAN_POINT ( 'NONE',  ( 110.4825671295247815, 0.1403307496149613920, -13.39321520033831447 ) ) ;
#43229 = CARTESIAN_POINT ( 'NONE',  ( 121.9859814775786333, -9.565557343593413364, -10.61323700422348004 ) ) ;
#43230 = CARTESIAN_POINT ( 'NONE',  ( 120.2274548109119934, -9.859900752359374465, -12.68260735090039404 ) ) ;
#43232 = CARTESIAN_POINT ( 'NONE',  ( 114.7816948109119863, -9.859900752359374465, -12.68260735090039404 ) ) ;
#43231 = AXIS2_PLACEMENT_3D ( 'NONE', #34096, #9950, #9040 ) ;
#43233 = CARTESIAN_POINT ( 'NONE',  ( 124.9009360172597098, 2.389294270081054439, -15.88150311065928832 ) ) ;
#43234 = CARTESIAN_POINT ( 'NONE',  ( 110.1353015045248469, -2.477300249445798297, -7.631215200338321125 ) ) ;
#43235 = CARTESIAN_POINT ( 'NONE',  ( 125.1626748109119802, -0.1624402480850797581, -16.17319339645315424 ) ) ;
#43236 = CIRCLE ( 'NONE', #41781, 1.499999999999996225 ) ;
#43237 = CARTESIAN_POINT ( 'NONE',  ( 123.5176014775786228, -0.8288870151387760510, -10.36305467784173118 ) ) ;
#43238 = DIRECTION ( 'NONE',  ( -1.000000000000000000, 0.000000000000000000, 0.000000000000000000 ) ) ;
#43239 = CARTESIAN_POINT ( 'NONE',  ( 112.7395348109119766, -4.153390946401321671, -8.397313243818183892 ) ) ;
#43240 = CARTESIAN_POINT ( 'NONE',  ( 121.3408766859119794, -9.033780868592240054, -16.85052413769862056 ) ) ;
#43241 = CARTESIAN_POINT ( 'NONE',  ( 115.7610046295247912, -4.863998795839590272, -7.631215200338315796 ) ) ;
#43242 = DIRECTION ( 'NONE',  ( 1.000000000000000000, 0.000000000000000000, 0.000000000000000000 ) ) ;
#43243 = LINE ( 'NONE', #36377, #39428 ) ;
#43244 = CARTESIAN_POINT ( 'NONE',  ( 121.1918081442452859, 0.9020085738987339008, -11.91225656197089222 ) ) ;
#43245 = CARTESIAN_POINT ( 'NONE',  ( 119.0929214775786278, -5.638512984488999180, -18.83840828888717311 ) ) ;
#43246 = CARTESIAN_POINT ( 'NONE',  ( 108.4684265045247997, -7.250697342233347165, -19.15521520033831138 ) ) ;
#43247 = ADVANCED_FACE ( 'NONE', ( #3268 ), #13985, .T. ) ;
#43248 = CARTESIAN_POINT ( 'NONE',  ( 115.4624148109119943, -5.638512984488999180, -18.83840828888717311 ) ) ;
#43249 = DIRECTION ( 'NONE',  ( 1.000000000000000000, 0.000000000000000000, -0.000000000000000000 ) ) ;
#43250 = VERTEX_POINT ( 'NONE', #17411 ) ;
#43251 = CARTESIAN_POINT ( 'NONE',  ( 91.11246428952674137, -26.75858941326842810, -11.54476601486570964 ) ) ;
#43252 = VECTOR ( 'NONE', #35449, 1000.000000000000000 ) ;
#43253 = CARTESIAN_POINT ( 'NONE',  ( 120.2274548109119934, 0.5811942927096110934, -14.16772938898807510 ) ) ;
#43254 = CARTESIAN_POINT ( 'NONE',  ( 125.1626748109119802, -0.1624402480850797581, -16.17319339645315424 ) ) ;
#43255 = APPLICATION_PROTOCOL_DEFINITION ( 'draft international standard', 'automotive_design', 1998, #40213 ) ;
#43256 = CARTESIAN_POINT ( 'NONE',  ( 113.1933481442453058, -5.574606645277164318, -18.38911715685844683 ) ) ;
#43257 = CARTESIAN_POINT ( 'NONE',  ( 123.9146881442452894, 0.9020085738987339008, -11.91225656197089222 ) ) ;
#43258 = CARTESIAN_POINT ( 'NONE',  ( 108.2600671295247992, -10.62599879583958540, -13.39321520033831447 ) ) ;
#43259 = CARTESIAN_POINT ( 'NONE',  ( 121.7023481442452777, -0.8288870151387760510, -10.36305467784173118 ) ) ;
#43260 = DIRECTION ( 'NONE',  ( -0.000000000000000000, -0.9284778069183718952, -0.3713878862591649677 ) ) ;
#43261 = CARTESIAN_POINT ( 'NONE',  ( 151.2860562277021472, -4.863998795839242995, -13.39321520033831447 ) ) ;
#43262 = ORIENTED_EDGE ( 'NONE', *, *, #351, .F. ) ;
#43263 = CLOSED_SHELL ( 'NONE', ( #21205, #8887, #41379, #38963, #4823, #25571, #17899, #30115, #32588, #6075, #36251, #43665, #2894, #11074, #23822, #4515, #15325, #34270, #5025, #29852, #9130, #13376, #15628, #8833, #24313, #31156, #44902, #3002, #41342, #6885 ) ) ;
#43264 = CARTESIAN_POINT ( 'NONE',  ( 122.7993923109119692, -0.4387604401700512802, -15.73000352943951619 ) ) ;
#43265 = CARTESIAN_POINT ( 'NONE',  ( 121.9292548109119849, -1.561330072975668948, -17.79121239304076951 ) ) ;
#43266 = ORIENTED_EDGE ( 'NONE', *, *, #1925, .T. ) ;
#43267 = DIRECTION ( 'NONE',  ( 0.000000000000000000, 0.000000000000000000, 1.000000000000000000 ) ) ;
#43268 = CARTESIAN_POINT ( 'NONE',  ( 67.18677111376662481, -1.717760636639239280, -9.553179424549121279 ) ) ;
#43269 = LINE ( 'NONE', #18863, #22357 ) ;
#43270 = CARTESIAN_POINT ( 'NONE',  ( 119.4332814775786318, -8.899110576539710493, -16.42337572283490132 ) ) ;
#43271 = CARTESIAN_POINT ( 'NONE',  ( 72.54180985774836188, -60.65691546915440568, -36.73639088572416966 ) ) ;
#43272 = CARTESIAN_POINT ( 'NONE',  ( 124.5348847846778852, -9.832371414934382159, -12.82702404581066880 ) ) ;
#43273 = CARTESIAN_POINT ( 'NONE',  ( 125.1059481442452750, -1.833838273342660141, -17.42832698103878286 ) ) ;
#43274 = FACE_OUTER_BOUND ( 'NONE', #11354, .T. ) ;
#43275 = CARTESIAN_POINT ( 'NONE',  ( 124.3500856911477399, -11.94161027609003334, -17.01447758398505172 ) ) ;
#43276 = CARTESIAN_POINT ( 'NONE',  ( 117.3911214775786505, -7.894159318335828068, -9.358103419637847864 ) ) ;
#43277 = CARTESIAN_POINT ( 'NONE',  ( 123.4608748109119745, 0.4262465694468514643, -12.03445270309931736 ) ) ;
#43278 = CARTESIAN_POINT ( 'NONE',  ( 119.7736414775786358, -10.30919188438810075, -12.61870101168855918 ) ) ;
#43279 = CARTESIAN_POINT ( 'NONE',  ( 117.3911214775786505, -1.561330072975668504, -17.79121239304076951 ) ) ;
#43280 = CARTESIAN_POINT ( 'NONE',  ( 113.6079577545248043, -2.791137627527939813, -18.39754474579286025 ) ) ;
#43281 = CARTESIAN_POINT ( 'NONE',  ( 125.5030348109119558, -6.222761293078241884, -8.102969835052219238 ) ) ;
#43282 = ORIENTED_EDGE ( 'NONE', *, *, #13999, .F. ) ;
#43283 = CARTESIAN_POINT ( 'NONE',  ( 118.6958348109119754, -6.344957434206665248, -7.627207830600338134 ) ) ;
#43284 = CARTESIAN_POINT ( 'NONE',  ( 113.6774108795247997, -8.938348069036489818, -9.318865927141430916 ) ) ;
#43285 = CARTESIAN_POINT ( 'NONE',  ( 110.4131140045248287, 0.1403307496149616695, -15.46607636864997204 ) ) ;
#43286 = CARTESIAN_POINT ( 'NONE',  ( 83.83554121260367253, -25.99489077589524300, -13.39321520033831625 ) ) ;
#43287 = VECTOR ( 'NONE', #12145, 1000.000000000000000 ) ;
#43288 = CARTESIAN_POINT ( 'NONE',  ( 112.5693548109119888, 0.4262465694468514643, -12.03445270309931736 ) ) ;
#43289 = ADVANCED_FACE ( 'NONE', ( #18073 ), #3403, .T. ) ;
#43290 = CARTESIAN_POINT ( 'NONE',  ( 123.9584548109119737, -12.80254289275730173, -14.38292102596908784 ) ) ;
#43291 = CARTESIAN_POINT ( 'NONE',  ( 116.8722546295247895, -4.863998795839590272, -18.39754474579285315 ) ) ;
#43292 = ORIENTED_EDGE ( 'NONE', *, *, #43498, .T. ) ;
#43293 = CARTESIAN_POINT ( 'NONE',  ( 126.6375681442452930, -10.15424416112533912, -14.75197769757731336 ) ) ;
#43294 = CARTESIAN_POINT ( 'NONE',  ( -13.56828337869051460, -4.779084862086333096, -17.94035226225507884 ) ) ;
#43295 = CARTESIAN_POINT ( 'NONE',  ( 119.9518141859119851, -0.8832429491016019485, -18.19431474523657855 ) ) ;
#43296 = PLANE ( 'NONE',  #34812 ) ;
#43297 = TOROIDAL_SURFACE ( 'NONE', #17106, 4.500000000000000000, 0.5000000000000000000 ) ;
#43298 = CARTESIAN_POINT ( 'NONE',  ( 107.8433483795247838, -8.402594152722688392, -16.93181055722141792 ) ) ;
#43299 = ORIENTED_EDGE ( 'NONE', *, *, #43431, .T. ) ;
#43300 = CARTESIAN_POINT ( 'NONE',  ( 115.8595014775786609, -1.834011780172310813, -8.268836392978581529 ) ) ;
#43301 = CARTESIAN_POINT ( 'NONE',  ( 125.7299414775786346, 0.9020085738987339008, -11.91225656197089222 ) ) ;
#43302 = CARTESIAN_POINT ( 'NONE',  ( 119.2063748109119814, -7.894159318335828068, -9.358103419637847864 ) ) ;
#43303 = CARTESIAN_POINT ( 'NONE',  ( 113.4769814775786330, 0.4262465694468514643, -12.03445270309931736 ) ) ;
#43304 = CARTESIAN_POINT ( 'NONE',  ( 70.19189222814998175, -41.58126682492877535, -29.83537093841426469 ) ) ;
#43305 = CARTESIAN_POINT ( 'NONE',  ( 71.85867159647438029, -25.32195970414818476, -4.893215200338314474 ) ) ;
#43306 = CARTESIAN_POINT ( 'NONE',  ( 113.8173414775786512, 0.2603800115204892296, -16.42320221600525088 ) ) ;
#43307 = CARTESIAN_POINT ( 'NONE',  ( 114.5803015045248117, -6.936859964151250502, -18.39754474579286025 ) ) ;
#43308 = EDGE_CURVE ( 'NONE', #29255, #2299, #3930, .T. ) ;
#43309 = CARTESIAN_POINT ( 'NONE',  ( 123.7445081442452874, -1.561330072975668948, -17.79121239304076951 ) ) ;
#43310 = B_SPLINE_CURVE_WITH_KNOTS ( 'NONE', 3,
 ( #7066, #10061, #27152, #41734, #2971, #20090, #38073, #33976, #10498, #17121, #41074, #3636, #31010, #24620, #6170, #34416, #23964, #6851, #17554, #37632, #27605, #44483, #31448, #20758, #218, #20313, #14131, #20536, #37849, #28047 ),
 .UNSPECIFIED., .F., .F.,
 ( 4, 2, 2, 1, 1, 2, 2, 2, 2, 2, 2, 2, 1, 1, 2, 2, 4 ),
 ( 0.000000000000000000, 0.1249999999999235056, 0.1874999999998855915, 0.2187499999998666345, 0.2343749999998555322, 0.2421874999998526456, 0.2499999999998497868, 0.3749999999999040212, 0.4374999999999267808, 0.4999999999999494849, 0.6249999999999925615, 0.6875000000000155431, 0.7187500000000270894, 0.7343750000000252021, 0.7421875000000229816, 0.7500000000000207612, 1.000000000000000000 ),
 .UNSPECIFIED. ) ;
#43311 = CARTESIAN_POINT ( 'NONE',  ( 137.2528433483972776, -8.502389972432839116, -17.19305753011830618 ) ) ;
#43312 = ORIENTED_EDGE ( 'NONE', *, *, #26228, .F. ) ;
#43313 = CARTESIAN_POINT ( 'NONE',  ( 112.9097148109120070, 0.2603800115204892296, -16.42320221600525088 ) ) ;
#43314 = CARTESIAN_POINT ( 'NONE',  ( 111.8319081442453182, -4.153390946401321671, -8.397313243818183892 ) ) ;
#43315 = LINE ( 'NONE', #25091, #44629 ) ;
#43316 = CARTESIAN_POINT ( 'NONE',  ( 122.0994348109119443, -10.15424416112533912, -14.75197769757731336 ) ) ;
#43317 = CIRCLE ( 'NONE', #7636, 5.999999999999997335 ) ;
#43318 = VERTEX_POINT ( 'NONE', #3709 ) ;
#43319 = CARTESIAN_POINT ( 'NONE',  ( 118.9794681442453026, -9.261995988541697145, -16.69588392320189030 ) ) ;
#43320 = CARTESIAN_POINT ( 'NONE',  ( 70.19189222814998175, -59.11650476797663600, -36.84940499091918298 ) ) ;
#43321 = DIRECTION ( 'NONE',  ( -1.000000000000000000, 0.000000000000000000, -0.000000000000000000 ) ) ;
#43322 = DIRECTION ( 'NONE',  ( -1.224775218828351862E-16, 0.9242245927363029745, 0.3818493186865928868 ) ) ;
#43323 = ADVANCED_BREP_SHAPE_REPRESENTATION ( '', ( #21433, #12375 ), #19397 ) ;
#43324 = CARTESIAN_POINT ( 'NONE',  ( 137.0105207745552889, -5.223277318015287385, -7.946479427247078675 ) ) ;
#43325 = VECTOR ( 'NONE', #18814, 1000.000000000000000 ) ;
#43326 = CARTESIAN_POINT ( 'NONE',  ( 115.4056881442453459, -2.084020599724406786, -8.691656652584148546 ) ) ;
#43327 = DIRECTION ( 'NONE',  ( -0.7400066460894876297, 0.6725995567522979890, 0.000000000000000000 ) ) ;
#43328 = CARTESIAN_POINT ( 'NONE',  ( 125.2512474355150260, -2.025430522367418718, -20.07795600484094933 ) ) ;
#43329 = CARTESIAN_POINT ( 'NONE',  ( 112.5126281442453120, 0.1319031606808879209, -14.10382304977623669 ) ) ;
#43330 = CARTESIAN_POINT ( 'NONE',  ( 111.8319081442453182, -5.638512984488999180, -18.83840828888717311 ) ) ;
#43331 = CARTESIAN_POINT ( 'NONE',  ( 123.9584548109119737, 0.04957186715663468302, -7.079989135975798042 ) ) ;
#43332 = CARTESIAN_POINT ( 'NONE',  ( 125.3895814775786448, -2.084020599724406786, -8.691656652584148546 ) ) ;
#43333 = DIRECTION ( 'NONE',  ( 1.000000000000000000, 0.000000000000000000, -0.000000000000000000 ) ) ;
#43334 = CARTESIAN_POINT ( 'NONE',  ( 120.8514481442452961, -7.893985811506177619, -18.51759400769804742 ) ) ;
#43335 = CARTESIAN_POINT ( 'NONE',  ( 120.3409081442453044, -0.4660016031367893996, -10.09054647747474043 ) ) ;
#43336 = ORIENTED_EDGE ( 'NONE', *, *, #28759, .T. ) ;
#43337 = CARTESIAN_POINT ( 'NONE',  ( 128.2184548109119930, -8.536181032868617180, -18.13822074491315561 ) ) ;
#43338 = CARTESIAN_POINT ( 'NONE',  ( 111.7327233795247849, -8.938348069036489818, -17.46756447353520159 ) ) ;
#43339 = CARTESIAN_POINT ( 'NONE',  ( 108.3295202545248657, 0.1403307496149616695, -11.32035403202665336 ) ) ;
#43340 = CARTESIAN_POINT ( 'NONE',  ( 111.3160046295247838, -4.863998795839590272, -18.39754474579285315 ) ) ;
#43341 = CARTESIAN_POINT ( 'NONE',  ( 126.3509913982061050, -9.799826457514038580, -12.25005761896067824 ) ) ;
#43342 = CARTESIAN_POINT ( 'NONE',  ( 116.1431348109119881, -10.30919188438810075, -12.61870101168855918 ) ) ;
#43343 = VERTEX_POINT ( 'NONE', #45011 ) ;
#43344 = CARTESIAN_POINT ( 'NONE',  ( 106.0375671295248310, -10.62599879583958540, -13.39321520033831447 ) ) ;
#43345 = DIRECTION ( 'NONE',  ( 0.000000000000000000, 0.3818493186865927203, -0.9242245927363029745 ) ) ;
#43346 = CARTESIAN_POINT ( 'NONE',  ( 115.1787814775786387, -0.1624402480850797581, -16.17319339645315424 ) ) ;
#43347 =( BOUNDED_SURFACE ( )  B_SPLINE_SURFACE ( 1, 2, ( 
 ( #23210, #19335, #2669, #19785, #16602, #13181, #36646, #15921, #37089, #29819, #12504, #30495, #26401, #40311, #5863, #16367, #9075, #30269, #44195, #26853, #40766, #20014, #22977, #27084, #9523, #23440, #1766, #36867, #37324, #6095, #15692, #6554, #35000, #41450, #10208, #31165, #13408, #38443, #13626, #21126, #3571, #17055, #7213, #17274, #38223, #28207, #41889, #31381, #3784, #31608, #27311, #42115, #23898, #41674, #152, #9987, #17708, #27536, #14066, #27985, #6328, #23669, #377, #37557, #34788, #34352, #30723, #20246, #10431, #30947, #34132, #37781, #14288, #44870, #2901, #16830, #41228, #3355, #17483, #10651, #45084, #44646, #24557, #13843, #7003, #20471, #3130, #24116, #38010, #6784, #34572, #20694, #27759, #24339, #20914, #25677, #11319, #28651, #31832, #28425, #8125, #4011, #29316, #25229, #602, #32278, #4470, #1046, #11768, #35464, #14513, #32498, #7662, #24770, #28874, #38661, #38893, #39583, #8345, #42336, #39127, #21800, #35694, #18157, #32053, #42787, #22246, #1273, #18390, #11548, #14962, #32718, #15412, #21577, #820, #17933, #25455, #39357, #22027, #35920, #42557, #4686, #4239, #7894, #18607, #11097, #24998, #1490, #35235, #15185, #7430, #14739, #29088, #43000, #36142, #4910, #21351, #18826, #10875, #34024, #41119, #20138, #29542, #27201, #26967, #44530, #13067, #16719, #40655, #20361, #6216, #41350, #9410, #43229, #23788, #2792, #34462, #36365, #3241, #11996, #5137, #25898, #40887, #27428, #30613, #13293, #34248, #13519, #9641, #6453, #44312, #10106, #16490, #2561, #23321, #9878, #3020, #19053, #37678, #16942, #30837, #17167, #44760, #24010, #5979, #39802, #33789, #37898, #8571, #32939, #37444, #6676, #20583, #22471, #1714, #23563, #15638, #43458, #12222, #26121, #30390, #37206, #19904, #3469, #21020, #34893, #38782, #14626, #267, #7324, #4352, #17384, #14176, #28093, #21244, #31273, #46, #13960, #3682, #24889, #706, #28544, #44984, #35121, #42448, #27871, #11214, #42002, #17603, #25119, #10766, #20802, #3904, #14402, #13742, #39015, #41785 ),
 ( #38333, #41566, #10540, #7785, #24442, #31056, #27651, #7110, #24662, #10987, #7553, #38549, #21694, #21468, #17822, #488, #31496, #31719, #28312, #42224, #18046, #35351, #4126, #31940, #35579, #10325, #24228, #38118, #6892, #34681, #35806, #15521, #11441, #36703, #32615, #39240, #39696, #11884, #8461, #19170, #42895, #8004, #39920, #15076, #32168, #36260, #937, #1160, #1824, #33050, #21913, #1381, #29205, #43114, #25564, #39470, #5027, #29654, #4576, #25787, #32391, #43567, #1601, #15753, #26236, #25346, #18501, #22364, #28988, #11657, #12336, #8234, #22141, #18942, #29428, #36033, #15296, #32832, #43342, #12112, #40146, #4802, #8910, #36486, #26015, #18272, #18723, #8681, #22585, #22808, #5253, #14856, #28765, #42671, #13014, #40372, #20304, #40601, #2963, #30554, #44026, #34189, #44258, #20081, #10054, #23732, #13242, #16891, #13468, #9135, #23957, #5698, #23505, #27144, #36926, #30784, #9361, #41065, #9822, #5927, #30110, #37623, #16434, #6397, #33736, #44707, #27370, #41292, #19849, #23269, #26468, #23039, #2735, #43798, #5471, #2507, #19615, #26913, #40834, #9589, #19391, #12788, #33499, #33280, #2278, #2055, #37390, #15978, #16208, #29881, #12563, #26690, #30332, #6162, #33967, #37151, #16660, #44475, #4066, #24174, #3627, #6843, #17990, #21187, #35293, #655, #31004, #10267, #208, #44931, #41511, #31889, #20750, #3415, #28039, #35065, #34629, #34841, #38495, #14122, #17546, #21411, #38066, #28488, #10930, #3846, #11157, #24391, #31662, #13689, #42393, #17331, #14570, #10489, #38279, #41947, #27598, #7495, #27812, #37839, #17766, #31221, #6616, #31440, #7271, #20529, #24832, #431, #34409, #3190, #40285, #17114, #13903, #10711, #14347, #41726, #7059, #20969, #28261, #42170, #24612, #38723, #22533, #29603, #36209, #35756, #32112, #43519, #43064, #32340, #35523, #11381, #33001, #18452, #25062, #38955, #42619, #4750, #4976, #18887, #32563, #1775, #1551, #18671, #39646, #39184, #7949, #15701, #4295, #15473, #21636, #14799, #11832, #25740, #8409, #22314, #18216 ) ),
 .UNSPECIFIED., .F., .F., .T. ) 
 B_SPLINE_SURFACE_WITH_KNOTS ( ( 2, 2 ),
 ( 3, 2, 2, 2, 2, 2, 2, 2, 2, 2, 2, 2, 2, 2, 2, 2, 2, 2, 2, 2, 2, 2, 2, 2, 2, 2, 2, 2, 2, 2, 2, 2, 2, 2, 2, 2, 2, 2, 2, 2, 2, 2, 2, 2, 2, 2, 2, 2, 2, 2, 2, 2, 2, 2, 2, 2, 2, 2, 2, 2, 2, 2, 2, 2, 2, 2, 2, 2, 2, 2, 2, 2, 2, 2, 2, 2, 2, 2, 2, 2, 2, 2, 2, 2, 2, 2, 2, 2, 2, 2, 2, 2, 2, 2, 2, 2, 2, 2, 2, 2, 2, 2, 2, 2, 2, 2, 2, 2, 2, 2, 2, 2, 2, 2, 2, 2, 2, 2, 2, 2, 2, 2, 2, 2, 2, 2, 2, 2, 3 ),
 ( 0.000000000000000000, 1.000000000000000000 ),
 ( 0.000000000000000000, 0.007812500000000000000, 0.01562500000000000000, 0.02343750000000000000, 0.03125000000000000000, 0.03906250000000000000, 0.04687500000000000000, 0.05468750000000000000, 0.06250000000000000000, 0.07031250000000000000, 0.07812500000000000000, 0.08593750000000000000, 0.09375000000000000000, 0.1015625000000000000, 0.1093750000000000000, 0.1171875000000000000, 0.1250000000000000000, 0.1328125000000000000, 0.1406250000000000000, 0.1484375000000000000, 0.1562500000000000000, 0.1640625000000000000, 0.1718750000000000000, 0.1796875000000000000, 0.1875000000000000000, 0.1953125000000000000, 0.2031250000000000000, 0.2109375000000000000, 0.2187500000000000000, 0.2265625000000000000, 0.2343750000000000000, 0.2421875000000000000, 0.2500000000000000000, 0.2578125000000000000, 0.2656250000000000000, 0.2734375000000000000, 0.2812500000000000000, 0.2890625000000000000, 0.2968750000000000000, 0.3046875000000000000, 0.3125000000000000000, 0.3203125000000000000, 0.3281250000000000000, 0.3359375000000000000, 0.3437500000000000000, 0.3515625000000000000, 0.3593750000000000000, 0.3671875000000000000, 0.3750000000000000000, 0.3828125000000000000, 0.3906250000000000000, 0.3984375000000000000, 0.4062500000000000000, 0.4140625000000000000, 0.4218750000000000000, 0.4296875000000000000, 0.4375000000000000000, 0.4453125000000000000, 0.4531250000000000000, 0.4609375000000000000, 0.4687500000000000000, 0.4765625000000000000, 0.4843750000000000000, 0.4921875000000000000, 0.5000000000000000000, 0.5078125000000000000, 0.5156250000000000000, 0.5234375000000000000, 0.5312500000000000000, 0.5390625000000000000, 0.5468750000000000000, 0.5546875000000000000, 0.5625000000000000000, 0.5703125000000000000, 0.5781250000000000000, 0.5859375000000000000, 0.5937500000000000000, 0.6015625000000000000, 0.6093750000000000000, 0.6171875000000000000, 0.6250000000000000000, 0.6328125000000000000, 0.6406250000000000000, 0.6484375000000000000, 0.6562500000000000000, 0.6640625000000000000, 0.6718750000000000000, 0.6796875000000000000, 0.6875000000000000000, 0.6953125000000000000, 0.7031250000000000000, 0.7109375000000000000, 0.7187500000000000000, 0.7265625000000000000, 0.7343750000000000000, 0.7421875000000000000, 0.7500000000000000000, 0.7578125000000000000, 0.7656250000000000000, 0.7734375000000000000, 0.7812500000000000000, 0.7890625000000000000, 0.7968750000000000000, 0.8046875000000000000, 0.8125000000000000000, 0.8203125000000000000, 0.8281250000000000000, 0.8359375000000000000, 0.8437500000000000000, 0.8515625000000000000, 0.8593750000000000000, 0.8671875000000000000, 0.8750000000000000000, 0.8828125000000000000, 0.8906250000000000000, 0.8984375000000000000, 0.9062500000000000000, 0.9140625000000000000, 0.9218750000000000000, 0.9296875000000000000, 0.9375000000000000000, 0.9453125000000000000, 0.9531250000000000000, 0.9609375000000000000, 0.9687500000000000000, 0.9765625000000000000, 0.9843750000000000000, 0.9921875000000000000, 1.000000000000000000 ),
 .UNSPECIFIED. ) 
 GEOMETRIC_REPRESENTATION_ITEM ( )  RATIONAL_B_SPLINE_SURFACE ( (
 ( 1.000000000000000000, 0.9238795325112869605, 1.000000000000000000, 0.9238795325112869605, 1.000000000000000000, 0.9238795325112869605, 1.000000000000000000, 0.9238795325112869605, 1.000000000000000000, 0.9238795325112869605, 1.000000000000000000, 0.9238795325112869605, 1.000000000000000000, 0.9238795325112869605, 1.000000000000000000, 0.9238795325112869605, 1.000000000000000000, 0.9238795325112869605, 1.000000000000000000, 0.9238795325112869605, 1.000000000000000000, 0.9238795325112869605, 1.000000000000000000, 0.9238795325112869605, 1.000000000000000000, 0.9238795325112869605, 1.000000000000000000, 0.9238795325112869605, 1.000000000000000000, 0.9238795325112869605, 1.000000000000000000, 0.9238795325112869605, 1.000000000000000000, 0.9238795325112869605, 1.000000000000000000, 0.9238795325112869605, 1.000000000000000000, 0.9238795325112869605, 1.000000000000000000, 0.9238795325112869605, 1.000000000000000000, 0.9238795325112869605, 1.000000000000000000, 0.9238795325112869605, 1.000000000000000000, 0.9238795325112869605, 1.000000000000000000, 0.9238795325112869605, 1.000000000000000000, 0.9238795325112869605, 1.000000000000000000, 0.9238795325112869605, 1.000000000000000000, 0.9238795325112869605, 1.000000000000000000, 0.9238795325112869605, 1.000000000000000000, 0.9238795325112869605, 1.000000000000000000, 0.9238795325112869605, 1.000000000000000000, 0.9238795325112869605, 1.000000000000000000, 0.9238795325112869605, 1.000000000000000000, 0.9238795325112869605, 1.000000000000000000, 0.9238795325112869605, 1.000000000000000000, 0.9238795325112869605, 1.000000000000000000, 0.9238795325112869605, 1.000000000000000000, 0.9238795325112869605, 1.000000000000000000, 0.9238795325112869605, 1.000000000000000000, 0.9238795325112869605, 1.000000000000000000, 0.9238795325112869605, 1.000000000000000000, 0.9238795325112869605, 1.000000000000000000, 0.9238795325112869605, 1.000000000000000000, 0.9238795325112869605, 1.000000000000000000, 0.9238795325112869605, 1.000000000000000000, 0.9238795325112869605, 1.000000000000000000, 0.9238795325112869605, 1.000000000000000000, 0.9238795325112869605, 1.000000000000000000, 0.9238795325112869605, 1.000000000000000000, 0.9238795325112869605, 1.000000000000000000, 0.9238795325112869605, 1.000000000000000000, 0.9238795325112869605, 1.000000000000000000, 0.9238795325112869605, 1.000000000000000000, 0.9238795325112869605, 1.000000000000000000, 0.9238795325112869605, 1.000000000000000000, 0.9238795325112869605, 1.000000000000000000, 0.9238795325112869605, 1.000000000000000000, 0.9238795325112869605, 1.000000000000000000, 0.9238795325112869605, 1.000000000000000000, 0.9238795325112869605, 1.000000000000000000, 0.9238795325112869605, 1.000000000000000000, 0.9238795325112869605, 1.000000000000000000, 0.9238795325112869605, 1.000000000000000000, 0.9238795325112869605, 1.000000000000000000, 0.9238795325112869605, 1.000000000000000000, 0.9238795325112869605, 1.000000000000000000, 0.9238795325112869605, 1.000000000000000000, 0.9238795325112869605, 1.000000000000000000, 0.9238795325112869605, 1.000000000000000000, 0.9238795325112869605, 1.000000000000000000, 0.9238795325112869605, 1.000000000000000000, 0.9238795325112869605, 1.000000000000000000, 0.9238795325112869605, 1.000000000000000000, 0.9238795325112869605, 1.000000000000000000, 0.9238795325112869605, 1.000000000000000000, 0.9238795325112869605, 1.000000000000000000, 0.9238795325112869605, 1.000000000000000000, 0.9238795325112869605, 1.000000000000000000, 0.9238795325112869605, 1.000000000000000000, 0.9238795325112869605, 1.000000000000000000, 0.9238795325112869605, 1.000000000000000000, 0.9238795325112869605, 1.000000000000000000, 0.9238795325112869605, 1.000000000000000000, 0.9238795325112869605, 1.000000000000000000, 0.9238795325112869605, 1.000000000000000000, 0.9238795325112869605, 1.000000000000000000, 0.9238795325112869605, 1.000000000000000000, 0.9238795325112869605, 1.000000000000000000, 0.9238795325112869605, 1.000000000000000000, 0.9238795325112869605, 1.000000000000000000, 0.9238795325112869605, 1.000000000000000000, 0.9238795325112869605, 1.000000000000000000, 0.9238795325112869605, 1.000000000000000000, 0.9238795325112869605, 1.000000000000000000, 0.9238795325112869605, 1.000000000000000000, 0.9238795325112869605, 1.000000000000000000, 0.9238795325112869605, 1.000000000000000000, 0.9238795325112869605, 1.000000000000000000, 0.9238795325112869605, 1.000000000000000000, 0.9238795325112869605, 1.000000000000000000, 0.9238795325112869605, 1.000000000000000000, 0.9238795325112869605, 1.000000000000000000, 0.9238795325112869605, 1.000000000000000000, 0.9238795325112869605, 1.000000000000000000, 0.9238795325112869605, 1.000000000000000000, 0.9238795325112869605, 1.000000000000000000, 0.9238795325112869605, 1.000000000000000000, 0.9238795325112869605, 1.000000000000000000, 0.9238795325112869605, 1.000000000000000000, 0.9238795325112869605, 1.000000000000000000, 0.9238795325112869605, 1.000000000000000000, 0.9238795325112869605, 1.000000000000000000, 0.9238795325112869605, 1.000000000000000000, 0.9238795325112869605, 1.000000000000000000, 0.9238795325112869605, 1.000000000000000000, 0.9238795325112869605, 1.000000000000000000, 0.9238795325112869605, 1.000000000000000000, 0.9238795325112869605, 1.000000000000000000, 0.9238795325112869605, 1.000000000000000000, 0.9238795325112869605, 1.000000000000000000, 0.9238795325112869605, 1.000000000000000000, 0.9238795325112869605, 1.000000000000000000, 0.9238795325112869605, 1.000000000000000000, 0.9238795325112869605, 1.000000000000000000, 0.9238795325112869605, 1.000000000000000000, 0.9238795325112869605, 1.000000000000000000, 0.9238795325112869605, 1.000000000000000000, 0.9238795325112869605, 1.000000000000000000, 0.9238795325112869605, 1.000000000000000000),
 ( 1.000000000000000000, 0.9238795325112869605, 1.000000000000000000, 0.9238795325112869605, 1.000000000000000000, 0.9238795325112869605, 1.000000000000000000, 0.9238795325112869605, 1.000000000000000000, 0.9238795325112869605, 1.000000000000000000, 0.9238795325112869605, 1.000000000000000000, 0.9238795325112869605, 1.000000000000000000, 0.9238795325112869605, 1.000000000000000000, 0.9238795325112869605, 1.000000000000000000, 0.9238795325112869605, 1.000000000000000000, 0.9238795325112869605, 1.000000000000000000, 0.9238795325112869605, 1.000000000000000000, 0.9238795325112869605, 1.000000000000000000, 0.9238795325112869605, 1.000000000000000000, 0.9238795325112869605, 1.000000000000000000, 0.9238795325112869605, 1.000000000000000000, 0.9238795325112869605, 1.000000000000000000, 0.9238795325112869605, 1.000000000000000000, 0.9238795325112869605, 1.000000000000000000, 0.9238795325112869605, 1.000000000000000000, 0.9238795325112869605, 1.000000000000000000, 0.9238795325112869605, 1.000000000000000000, 0.9238795325112869605, 1.000000000000000000, 0.9238795325112869605, 1.000000000000000000, 0.9238795325112869605, 1.000000000000000000, 0.9238795325112869605, 1.000000000000000000, 0.9238795325112869605, 1.000000000000000000, 0.9238795325112869605, 1.000000000000000000, 0.9238795325112869605, 1.000000000000000000, 0.9238795325112869605, 1.000000000000000000, 0.9238795325112869605, 1.000000000000000000, 0.9238795325112869605, 1.000000000000000000, 0.9238795325112869605, 1.000000000000000000, 0.9238795325112869605, 1.000000000000000000, 0.9238795325112869605, 1.000000000000000000, 0.9238795325112869605, 1.000000000000000000, 0.9238795325112869605, 1.000000000000000000, 0.9238795325112869605, 1.000000000000000000, 0.9238795325112869605, 1.000000000000000000, 0.9238795325112869605, 1.000000000000000000, 0.9238795325112869605, 1.000000000000000000, 0.9238795325112869605, 1.000000000000000000, 0.9238795325112869605, 1.000000000000000000, 0.9238795325112869605, 1.000000000000000000, 0.9238795325112869605, 1.000000000000000000, 0.9238795325112869605, 1.000000000000000000, 0.9238795325112869605, 1.000000000000000000, 0.9238795325112869605, 1.000000000000000000, 0.9238795325112869605, 1.000000000000000000, 0.9238795325112869605, 1.000000000000000000, 0.9238795325112869605, 1.000000000000000000, 0.9238795325112869605, 1.000000000000000000, 0.9238795325112869605, 1.000000000000000000, 0.9238795325112869605, 1.000000000000000000, 0.9238795325112869605, 1.000000000000000000, 0.9238795325112869605, 1.000000000000000000, 0.9238795325112869605, 1.000000000000000000, 0.9238795325112869605, 1.000000000000000000, 0.9238795325112869605, 1.000000000000000000, 0.9238795325112869605, 1.000000000000000000, 0.9238795325112869605, 1.000000000000000000, 0.9238795325112869605, 1.000000000000000000, 0.9238795325112869605, 1.000000000000000000, 0.9238795325112869605, 1.000000000000000000, 0.9238795325112869605, 1.000000000000000000, 0.9238795325112869605, 1.000000000000000000, 0.9238795325112869605, 1.000000000000000000, 0.9238795325112869605, 1.000000000000000000, 0.9238795325112869605, 1.000000000000000000, 0.9238795325112869605, 1.000000000000000000, 0.9238795325112869605, 1.000000000000000000, 0.9238795325112869605, 1.000000000000000000, 0.9238795325112869605, 1.000000000000000000, 0.9238795325112869605, 1.000000000000000000, 0.9238795325112869605, 1.000000000000000000, 0.9238795325112869605, 1.000000000000000000, 0.9238795325112869605, 1.000000000000000000, 0.9238795325112869605, 1.000000000000000000, 0.9238795325112869605, 1.000000000000000000, 0.9238795325112869605, 1.000000000000000000, 0.9238795325112869605, 1.000000000000000000, 0.9238795325112869605, 1.000000000000000000, 0.9238795325112869605, 1.000000000000000000, 0.9238795325112869605, 1.000000000000000000, 0.9238795325112869605, 1.000000000000000000, 0.9238795325112869605, 1.000000000000000000, 0.9238795325112869605, 1.000000000000000000, 0.9238795325112869605, 1.000000000000000000, 0.9238795325112869605, 1.000000000000000000, 0.9238795325112869605, 1.000000000000000000, 0.9238795325112869605, 1.000000000000000000, 0.9238795325112869605, 1.000000000000000000, 0.9238795325112869605, 1.000000000000000000, 0.9238795325112869605, 1.000000000000000000, 0.9238795325112869605, 1.000000000000000000, 0.9238795325112869605, 1.000000000000000000, 0.9238795325112869605, 1.000000000000000000, 0.9238795325112869605, 1.000000000000000000, 0.9238795325112869605, 1.000000000000000000, 0.9238795325112869605, 1.000000000000000000, 0.9238795325112869605, 1.000000000000000000, 0.9238795325112869605, 1.000000000000000000, 0.9238795325112869605, 1.000000000000000000, 0.9238795325112869605, 1.000000000000000000, 0.9238795325112869605, 1.000000000000000000, 0.9238795325112869605, 1.000000000000000000, 0.9238795325112869605, 1.000000000000000000, 0.9238795325112869605, 1.000000000000000000, 0.9238795325112869605, 1.000000000000000000, 0.9238795325112869605, 1.000000000000000000, 0.9238795325112869605, 1.000000000000000000, 0.9238795325112869605, 1.000000000000000000, 0.9238795325112869605, 1.000000000000000000, 0.9238795325112869605, 1.000000000000000000, 0.9238795325112869605, 1.000000000000000000, 0.9238795325112869605, 1.000000000000000000, 0.9238795325112869605, 1.000000000000000000, 0.9238795325112869605, 1.000000000000000000, 0.9238795325112869605, 1.000000000000000000, 0.9238795325112869605, 1.000000000000000000, 0.9238795325112869605, 1.000000000000000000, 0.9238795325112869605, 1.000000000000000000, 0.9238795325112869605, 1.000000000000000000, 0.9238795325112869605, 1.000000000000000000, 0.9238795325112869605, 1.000000000000000000, 0.9238795325112869605, 1.000000000000000000, 0.9238795325112869605, 1.000000000000000000, 0.9238795325112869605, 1.000000000000000000) ) ) 
 REPRESENTATION_ITEM ( '' )  SURFACE ( )  );
#43348 = CARTESIAN_POINT ( 'NONE',  ( 123.1249303192116713, -2.378957183258601393, -17.95140958770220152 ) ) ;
#43349 = CARTESIAN_POINT ( 'NONE',  ( 118.7525614775786380, -8.166667518702819706, -8.995218007635861213 ) ) ;
#43350 = CARTESIAN_POINT ( 'NONE',  ( 111.2465515045248168, -2.477300249445798297, -7.631215200338321125 ) ) ;
#43351 = LINE ( 'NONE', #33059, #22781 ) ;
#43352 = AXIS2_PLACEMENT_3D ( 'NONE', #31482, #14161, #33369 ) ;
#43353 = ORIENTED_EDGE ( 'NONE', *, *, #7730, .T. ) ;
#43354 = DIRECTION ( 'NONE',  ( -1.000000000000000000, 0.000000000000000000, -0.000000000000000000 ) ) ;
#43355 = CARTESIAN_POINT ( 'NONE',  ( 117.6180281442453150, -8.899110576539710493, -16.42337572283490132 ) ) ;
#43356 = CARTESIAN_POINT ( 'NONE',  ( 116.4267681442453153, -3.383040157471821630, -19.15922257007629170 ) ) ;
#43357 = CARTESIAN_POINT ( 'NONE',  ( 112.6260814775786514, -9.261995988541697145, -16.69588392320189030 ) ) ;
#43358 = CARTESIAN_POINT ( 'NONE',  ( 136.1055339648910376, -7.166517036409639552, -18.81773387731445624 ) ) ;
#43359 = CARTESIAN_POINT ( 'NONE',  ( 125.2194014775786286, 0.1319031606808879209, -14.10382304977623669 ) ) ;
#43360 = CARTESIAN_POINT ( 'NONE',  ( 116.8805814775786445, -3.505236298600246325, -18.68346056562440793 ) ) ;
#43361 = EDGE_LOOP ( 'NONE', ( #18724, #19439, #9557, #28841, #20996, #33493 ) ) ;
#43362 = VECTOR ( 'NONE', #6184, 999.9999999999998863 ) ;
#43363 = CARTESIAN_POINT ( 'NONE',  ( 123.2855641859119942, -8.321307733199551748, -9.223433127585318303 ) ) ;
#43364 = CARTESIAN_POINT ( 'NONE',  ( 112.6828081442453282, -7.893985811506177619, -18.51759400769804742 ) ) ;
#43365 = CARTESIAN_POINT ( 'NONE',  ( 117.9583881442453048, 0.1319031606808879209, -14.10382304977623669 ) ) ;
#43366 = ORIENTED_EDGE ( 'NONE', *, *, #23542, .T. ) ;
#43367 = FACE_BOUND ( 'NONE', #23129, .T. ) ;
#43368 = CARTESIAN_POINT ( 'NONE',  ( 113.3068014775786594, -8.166667518702817929, -8.995218007635859436 ) ) ;
#43369 = CARTESIAN_POINT ( 'NONE',  ( 106.4542858795248179, -8.402594152722688392, -9.854619843455216355 ) ) ;
#43370 = CARTESIAN_POINT ( 'NONE',  ( 112.5693548109119888, 0.4262465694468514643, -12.03445270309931736 ) ) ;
#43371 = EDGE_LOOP ( 'NONE', ( #7292, #20946, #24633, #5319 ) ) ;
#43372 = ORIENTED_EDGE ( 'NONE', *, *, #3382, .T. ) ;
#43373 = CARTESIAN_POINT ( 'NONE',  ( 120.5110881442453206, -3.505236298600246325, -18.68346056562440793 ) ) ;
#43374 = AXIS2_PLACEMENT_3D ( 'NONE', #19512, #40031, #22702 ) ;
#43375 = CARTESIAN_POINT ( 'NONE',  ( 122.6099748109119929, -0.8288870151387760510, -10.36305467784173118 ) ) ;
#43376 = CARTESIAN_POINT ( 'NONE',  ( 65.52066458535989568, -15.46830930983349184, -16.39321520033831092 ) ) ;
#43377 = ADVANCED_FACE ( 'NONE', ( #13770 ), #10572, .T. ) ;
#43378 = EDGE_LOOP ( 'NONE', ( #209, #33373, #41541, #29916, #618 ) ) ;
#43379 = DIRECTION ( 'NONE',  ( -0.000000000000000000, -0.000000000000000000, 1.000000000000000000 ) ) ;
#43380 = CARTESIAN_POINT ( 'NONE',  ( 62.16180176470561491, -65.29550861636488435, -44.87722419103883453 ) ) ;
#43381 = CONICAL_SURFACE ( 'NONE', #9908, 1.610000000000000986, 0.9599310885968765916 ) ;
#43382 = CARTESIAN_POINT ( 'NONE',  ( 106.8710046295248759, -4.863998795839590272, -7.631215200338315796 ) ) ;
#43383 = CARTESIAN_POINT ( 'NONE',  ( 115.2355081442453155, -10.30919188438810075, -12.61870101168855918 ) ) ;
#43385 = CARTESIAN_POINT ( 'NONE',  ( 117.2776681442452968, -4.153390946401321671, -8.397313243818183892 ) ) ;
#43384 = CARTESIAN_POINT ( 'NONE',  ( 114.4980614775786592, -7.893985811506177619, -18.51759400769804742 ) ) ;
#43386 = CARTESIAN_POINT ( 'NONE',  ( 122.4965214775786251, 0.1319031606808879209, -14.10382304977623669 ) ) ;
#43387 = CARTESIAN_POINT ( 'NONE',  ( 75.95778847736514194, -3.256761025687008537, -19.39321520033831447 ) ) ;
#43388 = ORIENTED_EDGE ( 'NONE', *, *, #10263, .F. ) ;
#43389 = AXIS2_PLACEMENT_3D ( 'NONE', #27688, #45019, #6485 ) ;
#43390 = CARTESIAN_POINT ( 'NONE',  ( 121.2485348109119769, -8.899110576539710493, -16.42337572283490132 ) ) ;
#43391 = CARTESIAN_POINT ( 'NONE',  ( 125.6164881442453094, -9.565557343593413364, -10.61323700422348004 ) ) ;
#43392 = CARTESIAN_POINT ( 'NONE',  ( 111.3854577545248645, -7.250697342233347165, -7.631215200338321125 ) ) ;
#43393 = CARTESIAN_POINT ( 'NONE',  ( 115.7610046295247912, -4.863998795839590272, -18.39754474579285315 ) ) ;
#43394 = CARTESIAN_POINT ( 'NONE',  ( 109.9963952545248134, 0.8980012041604421569, -11.00651665394454071 ) ) ;
#43395 = CARTESIAN_POINT ( 'NONE',  ( 120.1140014775786398, -1.561330072975668504, -17.79121239304076951 ) ) ;
#43396 = VERTEX_POINT ( 'NONE', #27681 ) ;
#43397 = CARTESIAN_POINT ( 'NONE',  ( 121.0783548109119749, 0.2603800115204892296, -16.42320221600525088 ) ) ;
#43398 = CARTESIAN_POINT ( 'NONE',  ( 62.88810427208139942, -37.62639143044070522, -5.060171215880807871 ) ) ;
#43399 = LINE ( 'NONE', #16948, #43083 ) ;
#43400 = CARTESIAN_POINT ( 'NONE',  ( 117.1074881442453233, -10.63000616557722466, -14.87417383870573495 ) ) ;
#43401 = CARTESIAN_POINT ( 'NONE',  ( 115.9729548109119861, -6.344957434206662583, -7.627207830600332805 ) ) ;
#43402 = CARTESIAN_POINT ( 'NONE',  ( 123.6294907289968279, -6.032552146994431652, -18.32589373581284775 ) ) ;
#43403 = PLANE ( 'NONE',  #41713 ) ;
#43404 = EDGE_CURVE ( 'NONE', #35019, #11934, #8714, .T. ) ;
#43405 = ORIENTED_EDGE ( 'NONE', *, *, #43434, .T. ) ;
#43406 = DIRECTION ( 'NONE',  ( 0.000000000000000000, 0.000000000000000000, -1.000000000000000000 ) ) ;
#43407 = CARTESIAN_POINT ( 'NONE',  ( 109.2294458807338344, -10.05974036254392878, -11.12818462664568386 ) ) ;
#43408 = CARTESIAN_POINT ( 'NONE',  ( 119.7169148109119874, -0.1624402480850797581, -16.17319339645315424 ) ) ;
#43409 = AXIS2_PLACEMENT_3D ( 'NONE', #42740, #4194, #25409 ) ;
#43410 = CARTESIAN_POINT ( 'NONE',  ( 110.2742077545248094, -2.791137627527939813, -18.39754474579286025 ) ) ;
#43411 = CARTESIAN_POINT ( 'NONE',  ( 115.2748327545248657, -6.936859964151250502, -8.388885654883777576 ) ) ;
#43412 = CARTESIAN_POINT ( 'NONE',  ( 118.1285681442453068, -2.084020599724406786, -8.691656652584148546 ) ) ;
#43413 = LINE ( 'NONE', #5096, #43047 ) ;
#43414 = CARTESIAN_POINT ( 'NONE',  ( 70.07532415883380850, -25.67919796285898926, -5.724353937072305776 ) ) ;
#43415 = ADVANCED_FACE ( 'NONE', ( #7135 ), #2678, .T. ) ;
#43416 = CARTESIAN_POINT ( 'NONE',  ( 125.9568481442452850, -6.344957434206665248, -7.627207830600338134 ) ) ;
#43417 = CARTESIAN_POINT ( 'NONE',  ( 120.8514481442452961, -7.893985811506177619, -18.51759400769804742 ) ) ;
#43418 = ORIENTED_EDGE ( 'NONE', *, *, #13240, .T. ) ;
#43419 = EDGE_CURVE ( 'NONE', #12164, #26262, #26714, .T. ) ;
#43420 = VECTOR ( 'NONE', #45133, 1000.000000000000000 ) ;
#43421 = CARTESIAN_POINT ( 'NONE',  ( 120.1140014775786398, -7.894159318335828068, -9.358103419637847864 ) ) ;
#43422 = CARTESIAN_POINT ( 'NONE',  ( 114.2711548109119803, -9.988377603198976828, -10.36322818467138340 ) ) ;
#43423 = CARTESIAN_POINT ( 'NONE',  ( 123.2906948109119867, -8.166667518702819706, -8.995218007635861213 ) ) ;
#43424 = CARTESIAN_POINT ( 'NONE',  ( 121.3619881442452879, -5.574606645277164318, -18.38911715685844683 ) ) ;
#43425 = ORIENTED_EDGE ( 'NONE', *, *, #7215, .T. ) ;
#43426 = CARTESIAN_POINT ( 'NONE',  ( 125.2761281442453054, 0.4262465694468514643, -12.03445270309931736 ) ) ;
#43427 = CIRCLE ( 'NONE', #17239, 3.499999999999998668 ) ;
#43428 = CARTESIAN_POINT ( 'NONE',  ( 118.5823814775786360, -1.834011780172310813, -8.268836392978581529 ) ) ;
#43429 = LINE ( 'NONE', #40230, #1250 ) ;
#43430 = CARTESIAN_POINT ( 'NONE',  ( 122.7234281442452755, -5.638512984488999180, -18.83840828888717311 ) ) ;
#43431 = EDGE_CURVE ( 'NONE', #39048, #41341, #31096, .T. ) ;
#43432 = DIRECTION ( 'NONE',  ( 1.000000000000000000, 0.000000000000000000, 0.000000000000000000 ) ) ;
#43433 = ADVANCED_FACE ( 'NONE', ( #11238 ), #38147, .F. ) ;
#43434 = EDGE_CURVE ( 'NONE', #17999, #23145, #43989, .T. ) ;
#43435 = CARTESIAN_POINT ( 'NONE',  ( 119.7434548109119703, -1.204716393658298523, -20.50726132761981901 ) ) ;
#43436 = CARTESIAN_POINT ( 'NONE',  ( 137.2446579711038908, -1.128119387170134047, -17.11910725436554870 ) ) ;
#43437 = CARTESIAN_POINT ( 'NONE',  ( 107.7044421295247929, -9.868328341294093420, -13.39321520033831447 ) ) ;
#43438 = CARTESIAN_POINT ( 'NONE',  ( 70.36267391504958368, -5.685877709920885259, -19.39321520033831447 ) ) ;
#43439 = CARTESIAN_POINT ( 'NONE',  ( 136.5935259641925654, -10.15732810381489593, -11.25679434072407581 ) ) ;
#43440 = CARTESIAN_POINT ( 'NONE',  ( 118.0718414775786442, -0.8288870151387760510, -10.36305467784173118 ) ) ;
#43441 = CARTESIAN_POINT ( 'NONE',  ( 125.0492214775786266, -6.344957434206665248, -7.627207830600338134 ) ) ;
#43442 = CARTESIAN_POINT ( 'NONE',  ( 64.38259412312832808, -13.03244878199202361, -15.64233727451349054 ) ) ;
#43443 = ORIENTED_EDGE ( 'NONE', *, *, #3802, .T. ) ;
#43444 = CARTESIAN_POINT ( 'NONE',  ( 115.7523666692504065, -2.311015703046737535, -18.04188382666267998 ) ) ;
#43445 = CARTESIAN_POINT ( 'NONE',  ( 111.4549108795247747, -1.325403438956436419, -16.93181055722141792 ) ) ;
#43446 = CARTESIAN_POINT ( 'NONE',  ( 117.3343948109119737, -6.222761293078241884, -8.102969835052219238 ) ) ;
#43447 = FACE_OUTER_BOUND ( 'NONE', #27117, .T. ) ;
#43448 = TOROIDAL_SURFACE ( 'NONE', #512, 6.500000000000000000, 1.500000000000000000 ) ;
#43449 = CARTESIAN_POINT ( 'NONE',  ( 65.49030871267177645, -0.3060001693188343919, -10.39321520033831447 ) ) ;
#43450 = CARTESIAN_POINT ( 'NONE',  ( -2.329871626679969054, -6.983709645767248730, -19.17689330043476659 ) ) ;
#43452 = CARTESIAN_POINT ( 'NONE',  ( 122.5532481442453019, -10.63000616557722466, -14.87417383870573495 ) ) ;
#43451 = CARTESIAN_POINT ( 'NONE',  ( 60.62026699881264591, -14.54430726831175669, -7.482851213058667739 ) ) ;
#43453 = CARTESIAN_POINT ( 'NONE',  ( 123.4041481442452834, 0.1319031606808879209, -14.10382304977623669 ) ) ;
#43454 = ORIENTED_EDGE ( 'NONE', *, *, #25101, .F. ) ;
#43455 = FACE_OUTER_BOUND ( 'NONE', #43731, .T. ) ;
#43456 = CARTESIAN_POINT ( 'NONE',  ( 65.83110444452054821, -15.38354445881851440, -10.39321520033831625 ) ) ;
#43457 = CARTESIAN_POINT ( 'NONE',  ( 108.2600671295247992, 0.1403307496149613920, -13.39321520033831447 ) ) ;
#43458 = CARTESIAN_POINT ( 'NONE',  ( 124.4819548109119722, -2.084020599724406786, -8.691656652584148546 ) ) ;
#43459 = CARTESIAN_POINT ( 'NONE',  ( 120.6245414775786458, -0.1624402480850797581, -16.17319339645315424 ) ) ;
#43460 = CIRCLE ( 'NONE', #2658, 5.999999999999997335 ) ;
#43461 = CARTESIAN_POINT ( 'NONE',  ( 119.7169148109119874, -0.1624402480850797581, -16.17319339645315424 ) ) ;
#43462 = CARTESIAN_POINT ( 'NONE',  ( 124.3741441133367545, 1.422210110677154971, -18.26991642492331636 ) ) ;
#43463 = CARTESIAN_POINT ( 'NONE',  ( 108.4684265045247997, -7.250697342233347165, -19.15521520033831138 ) ) ;
#43464 = CARTESIAN_POINT ( 'NONE',  ( -6.962123463324038752, -11.49046785505262669, -7.393215200338315363 ) ) ;
#43465 = CARTESIAN_POINT ( 'NONE',  ( 85.82015659721905365, -25.99489077589524300, -13.39321520033831625 ) ) ;
#43466 = CARTESIAN_POINT ( 'NONE',  ( -13.56828337869050927, -4.779084862086334873, -8.893215200338314474 ) ) ;
#43467 = CARTESIAN_POINT ( 'NONE',  ( 108.7462390045248242, 0.8980012041604421569, -15.77991374673208469 ) ) ;
#43468 = CARTESIAN_POINT ( 'NONE',  ( -12.36826994950264336, -4.374949827406451774, -19.39321520033831803 ) ) ;
#43469 = CARTESIAN_POINT ( 'NONE',  ( 63.69189222814998175, -37.86175736943883408, -4.893215200338314474 ) ) ;
#43470 = CARTESIAN_POINT ( 'NONE',  ( 120.3409081442453044, -0.4660016031367893996, -10.09054647747474043 ) ) ;
#43471 = CARTESIAN_POINT ( 'NONE',  ( 118.8092881442453290, -9.988377603198976828, -10.36322818467138340 ) ) ;
#43472 = CARTESIAN_POINT ( 'NONE',  ( 107.4960827545248350, -2.477300249445798297, -19.15521520033831138 ) ) ;
#43473 = CARTESIAN_POINT ( 'NONE',  ( 118.0151148109119816, -10.63000616557722466, -14.87417383870573495 ) ) ;
#43474 = LINE ( 'NONE', #33180, #25030 ) ;
#43475 = VERTEX_POINT ( 'NONE', #32418 ) ;
#43476 = DIRECTION ( 'NONE',  ( 0.9387755102040822308, -0.3445294493088585375, 0.000000000000000000 ) ) ;
#43477 = EDGE_CURVE ( 'NONE', #13151, #26347, #32192, .T. ) ;
#43478 = CARTESIAN_POINT ( 'NONE',  ( 121.3052614775786111, -1.834011780172310813, -8.268836392978581529 ) ) ;
#43479 = CARTESIAN_POINT ( 'NONE',  ( 120.0572748109119772, -3.383040157471821630, -19.15922257007629170 ) ) ;
#43480 = CARTESIAN_POINT ( 'NONE',  ( 125.2761281442453054, 0.4262465694468514643, -12.03445270309931736 ) ) ;
#43481 = AXIS2_PLACEMENT_3D ( 'NONE', #6714, #9916, #20624 ) ;
#43482 = DIRECTION ( 'NONE',  ( 0.000000000000000000, 0.000000000000000000, 1.000000000000000000 ) ) ;
#43483 = CARTESIAN_POINT ( 'NONE',  ( 113.7606148109119886, -7.894159318335828068, -9.358103419637847864 ) ) ;
#43484 = CARTESIAN_POINT ( 'NONE',  ( 123.7445081442452874, -1.561330072975668948, -17.79121239304076951 ) ) ;
#43485 = CARTESIAN_POINT ( 'NONE',  ( 111.3854577545248645, -7.250697342233347165, -7.631215200338321125 ) ) ;
#43486 = CARTESIAN_POINT ( 'NONE',  ( 119.2063748109119814, -7.894159318335828068, -9.358103419637847864 ) ) ;
#43487 = CARTESIAN_POINT ( 'NONE',  ( 70.19189222814998175, -54.26662894631272849, -34.90947156805651019 ) ) ;
#43488 = CARTESIAN_POINT ( 'NONE',  ( 116.3166296295247832, -4.863998795839590272, -19.15521520033831493 ) ) ;
#43489 = VERTEX_POINT ( 'NONE', #43591 ) ;
#43490 = ADVANCED_FACE ( 'NONE', ( #5053 ), #11911, .T. ) ;
#43491 = DIRECTION ( 'NONE',  ( 0.000000000000000000, -0.9242245927363027524, -0.3818493186865928868 ) ) ;
#43492 = CARTESIAN_POINT ( 'NONE',  ( 121.8725281442453223, -3.383040157471821630, -19.15922257007629170 ) ) ;
#43493 = CARTESIAN_POINT ( 'NONE',  ( 70.19189222814998175, -100.0979043305785581, -53.24182196210380624 ) ) ;
#43494 = CARTESIAN_POINT ( 'NONE',  ( 125.0302870206147219, 1.954631471695863487, -10.15285534273483847 ) ) ;
#43495 = EDGE_CURVE ( 'NONE', #4599, #44158, #22724, .T. ) ;
#43496 = CARTESIAN_POINT ( 'NONE',  ( 119.5467348109119712, -5.574606645277164318, -18.38911715685844683 ) ) ;
#43497 = CARTESIAN_POINT ( 'NONE',  ( 112.0588148109119828, 0.5811942927096154232, -14.16772938898807155 ) ) ;
#43498 = EDGE_CURVE ( 'NONE', #15377, #31774, #29631, .T. ) ;
#43499 = CARTESIAN_POINT ( 'NONE',  ( 84.38170309240724976, -25.99489077589524300, -13.39321520033831447 ) ) ;
#43500 = CARTESIAN_POINT ( 'NONE',  ( 122.0994348109119443, -10.15424416112533912, -14.75197769757731336 ) ) ;
#43501 = CARTESIAN_POINT ( 'NONE',  ( 123.3116793777725064, -1.267766418764731728, -16.93314635290706605 ) ) ;
#43502 = CARTESIAN_POINT ( 'NONE',  ( 124.8790414775786246, -8.899110576539710493, -16.42337572283490132 ) ) ;
#43503 = CARTESIAN_POINT ( 'NONE',  ( 116.0286950891469786, 2.331313199634366118, -19.89321520033831447 ) ) ;
#43505 = CARTESIAN_POINT ( 'NONE',  ( 122.9503348109119827, 0.5811942927096110934, -14.16772938898807510 ) ) ;
#43504 = VECTOR ( 'NONE', #14905, 1000.000000000000000 ) ;
#43506 = CARTESIAN_POINT ( 'NONE',  ( 118.0718414775786442, -0.8288870151387760510, -10.36305467784173118 ) ) ;
#43507 = CARTESIAN_POINT ( 'NONE',  ( 122.4397948109119767, -0.1624402480850797581, -16.17319339645315424 ) ) ;
#43508 = ORIENTED_EDGE ( 'NONE', *, *, #44296, .F. ) ;
#43509 = CARTESIAN_POINT ( 'NONE',  ( 121.9292548109119849, -1.561330072975668948, -17.79121239304076951 ) ) ;
#43510 = CARTESIAN_POINT ( 'NONE',  ( 116.5969481442453031, 0.5811942927096154232, -14.16772938898807155 ) ) ;
#43511 = CARTESIAN_POINT ( 'NONE',  ( 113.6932004811916954, -3.807985514183293230, -19.09877912889401230 ) ) ;
#43512 = CARTESIAN_POINT ( 'NONE',  ( 125.3895814775786448, -2.084020599724406786, -8.691656652584148546 ) ) ;
#43513 = CARTESIAN_POINT ( 'NONE',  ( 121.6456214775786293, -10.63000616557722466, -14.87417383870573495 ) ) ;
#43514 = CARTESIAN_POINT ( 'NONE',  ( 114.0246765045248196, -7.250697342233347165, -19.15521520033831138 ) ) ;
#43515 = CARTESIAN_POINT ( 'NONE',  ( 108.0517077545248696, -2.791137627527939813, -18.39754474579286025 ) ) ;
#43516 = CARTESIAN_POINT ( 'NONE',  ( 78.69189222814998175, -55.76310523276723785, -40.89321520033831092 ) ) ;
#43517 = CARTESIAN_POINT ( 'NONE',  ( 112.7395348109119766, -4.153390946401321671, -8.397313243818183892 ) ) ;
#43518 = DIRECTION ( 'NONE',  ( -0.7871354856660202071, 0.6167752151498580027, 0.002461946824133919541 ) ) ;
#43519 = CARTESIAN_POINT ( 'NONE',  ( 124.5954081442453116, -3.383040157471821630, -19.15922257007629170 ) ) ;
#43520 = ORIENTED_EDGE ( 'NONE', *, *, #2147, .F. ) ;
#43521 = CARTESIAN_POINT ( 'NONE',  ( 124.7088614775786226, -9.565557343593413364, -10.61323700422348004 ) ) ;
#43522 = CARTESIAN_POINT ( 'NONE',  ( 123.6328298109119714, -2.173413727453600508, -8.297982527556802879 ) ) ;
#43523 = AXIS2_PLACEMENT_3D ( 'NONE', #30885, #16309, #5798 ) ;
#43524 = CARTESIAN_POINT ( 'NONE',  ( 123.7807890828414230, -8.372502050422333753, -17.31760344562334808 ) ) ;
#43525 = CARTESIAN_POINT ( 'NONE',  ( 109.2324108795247923, -1.325403438956436419, -16.93181055722141792 ) ) ;
#43526 = ORIENTED_EDGE ( 'NONE', *, *, #24911, .T. ) ;
#43527 = CARTESIAN_POINT ( 'NONE',  ( 119.2631014775786298, 0.2603800115204892296, -16.42320221600525088 ) ) ;
#43528 = CARTESIAN_POINT ( 'NONE',  ( 113.2500748109119968, -6.344957434206662583, -7.627207830600333693 ) ) ;
#43529 = CARTESIAN_POINT ( 'NONE',  ( 122.9503348109119827, -9.859900752359378018, -12.68260735090039759 ) ) ;
#43530 = CARTESIAN_POINT ( 'NONE',  ( 116.2565881442453133, -0.8288870151387760510, -10.36305467784173118 ) ) ;
#43531 = CARTESIAN_POINT ( 'NONE',  ( 42.57150613532612482, -13.18613447638990088, -12.39321520033831447 ) ) ;
#43532 = CARTESIAN_POINT ( 'NONE',  ( 124.3685014775786186, -10.63000616557722999, -14.87417383870572962 ) ) ;
#43533 = CARTESIAN_POINT ( 'NONE',  ( 115.9729548109119861, -6.344957434206662583, -7.627207830600332805 ) ) ;
#43534 = EDGE_CURVE ( 'NONE', #3183, #31639, #21111, .T. ) ;
#43535 = CARTESIAN_POINT ( 'NONE',  ( 109.9269421295247753, -9.868328341294093420, -13.39321520033831447 ) ) ;
#43536 = CIRCLE ( 'NONE', #37710, 4.999999999999998224 ) ;
#43537 = CARTESIAN_POINT ( 'NONE',  ( 125.6732148109119862, 0.5811942927096110934, -14.16772938898807510 ) ) ;
#43538 = DIRECTION ( 'NONE',  ( 0.000000000000000000, 0.000000000000000000, -1.000000000000000000 ) ) ;
#43539 = ORIENTED_EDGE ( 'NONE', *, *, #11060, .F. ) ;
#43540 = CARTESIAN_POINT ( 'NONE',  ( 115.9162281442453235, -4.089484607189486809, -7.948022111789456723 ) ) ;
#43541 = CARTESIAN_POINT ( 'NONE',  ( 112.8529881442453160, -7.894159318335828068, -9.358103419637847864 ) ) ;
#43542 = DIRECTION ( 'NONE',  ( 0.5040994586965589219, 0.8636456077245089347, 0.000000000000000000 ) ) ;
#43543 = CARTESIAN_POINT ( 'NONE',  ( 113.3635281442453504, -9.988377603198976828, -10.36322818467138340 ) ) ;
#43544 = ORIENTED_EDGE ( 'NONE', *, *, #10288, .T. ) ;
#43545 = CARTESIAN_POINT ( 'NONE',  ( 117.7314814775786260, -4.089484607189486809, -7.948022111789456723 ) ) ;
#43546 = ADVANCED_FACE ( 'NONE', ( #29012 ), #23096, .T. ) ;
#43547 = PLANE ( 'NONE',  #12146 ) ;
#43548 = CARTESIAN_POINT ( 'NONE',  ( 109.5796765045248264, -2.791137627527992215, -8.388885654883745602 ) ) ;
#43549 = CARTESIAN_POINT ( 'NONE',  ( 124.9868051361299166, -1.575707845324203493, -20.23615509330177531 ) ) ;
#43550 = CARTESIAN_POINT ( 'NONE',  ( 116.0286950891469786, 2.331313199634366118, -6.893215200338315363 ) ) ;
#43551 = CARTESIAN_POINT ( 'NONE',  ( 113.3635281442453504, -0.1624402480850797581, -16.17319339645315424 ) ) ;
#43552 = FACE_OUTER_BOUND ( 'NONE', #33585, .T. ) ;
#43553 = CARTESIAN_POINT ( 'NONE',  ( 125.0370334466769151, -1.627738329600721290, -20.20867991148268317 ) ) ;
#43554 = CARTESIAN_POINT ( 'NONE',  ( 113.3068014775786594, -1.833838273342658809, -17.42832698103878286 ) ) ;
#43555 = CARTESIAN_POINT ( 'NONE',  ( 125.5030348109119558, -6.222761293078241884, -8.102969835052219238 ) ) ;
#43556 = CARTESIAN_POINT ( 'NONE',  ( 121.7575954359119805, 0.5291689781388270175, -13.89700978578772705 ) ) ;
#43557 = CARTESIAN_POINT ( 'NONE',  ( 126.6375681442452930, -10.15424416112533912, -14.75197769757731336 ) ) ;
#43558 = CARTESIAN_POINT ( 'NONE',  ( 112.9097148109120070, -9.565557343593413364, -10.61323700422348004 ) ) ;
#43559 = CARTESIAN_POINT ( 'NONE',  ( 121.9292548109119849, -1.561330072975668948, -17.79121239304076951 ) ) ;
#43560 = CARTESIAN_POINT ( 'NONE',  ( 122.7234281442452755, -5.638512984488999180, -18.83840828888717311 ) ) ;
#43561 = ORIENTED_EDGE ( 'NONE', *, *, #5394, .T. ) ;
#43562 = CARTESIAN_POINT ( 'NONE',  ( 126.3243314201126850, -8.659408885743252071, -16.72895926446462411 ) ) ;
#43563 = CARTESIAN_POINT ( 'NONE',  ( 110.7603796295247918, -4.863998795839590272, -19.15521520033831493 ) ) ;
#43564 = CARTESIAN_POINT ( 'NONE',  ( 109.3713171295247832, 0.1403307496149613920, -13.39321520033831447 ) ) ;
#43565 = CARTESIAN_POINT ( 'NONE',  ( 108.3989733795248753, -1.325403438956436419, -9.854619843455211026 ) ) ;
#43566 = CARTESIAN_POINT ( 'NONE',  ( 128.2184548109119930, -10.36826876090625760, -11.00511718064540467 ) ) ;
#43567 = CARTESIAN_POINT ( 'NONE',  ( 115.1787814775786387, -9.988377603198976828, -10.36322818467138340 ) ) ;
#43568 = VERTEX_POINT ( 'NONE', #15777 ) ;
#43569 = DIRECTION ( 'NONE',  ( 0.000000000000000000, -0.9284778069183718952, -0.3713878862591650232 ) ) ;
#43570 = CARTESIAN_POINT ( 'NONE',  ( 123.9800954359119913, 0.5291689781388270175, -13.89700978578772705 ) ) ;
#43571 = CARTESIAN_POINT ( 'NONE',  ( 143.3676850761856940, -69.76310523276724496, -16.89321520033831447 ) ) ;
#43572 = CARTESIAN_POINT ( 'NONE',  ( 112.6260814775786514, -0.8288870151387760510, -10.36305467784173118 ) ) ;
#43573 = CARTESIAN_POINT ( 'NONE',  ( 123.2697102440515238, -2.467220198592778413, -17.83387418641524391 ) ) ;
#43574 = CARTESIAN_POINT ( 'NONE',  ( 118.2420214775786320, -3.383040157471821630, -19.15922257007629170 ) ) ;
#43575 = CARTESIAN_POINT ( 'NONE',  ( 111.0381921295247878, 0.8980012041604618078, -13.39321520033831447 ) ) ;
#43576 = CARTESIAN_POINT ( 'NONE',  ( 119.4944236525450236, -2.378957183258601393, -17.95140958770220152 ) ) ;
#43577 = EDGE_LOOP ( 'NONE', ( #37417, #35377, #16773, #28567 ) ) ;
#43578 = CARTESIAN_POINT ( 'NONE',  ( 110.8551676093651821, 0.5600166689815611054, -14.64321520033834645 ) ) ;
#43579 = CARTESIAN_POINT ( 'NONE',  ( 118.2420214775786320, -6.222761293078241884, -8.102969835052219238 ) ) ;
#43580 = CARTESIAN_POINT ( 'NONE',  ( 116.5402214775786405, 0.2603800115204892296, -16.42320221600525088 ) ) ;
#43581 = CARTESIAN_POINT ( 'NONE',  ( 114.7816948109119863, -9.859900752359374465, -12.68260735090039404 ) ) ;
#43582 = CARTESIAN_POINT ( 'NONE',  ( 114.2144281442453178, -8.166667518702817929, -8.995218007635859436 ) ) ;
#43583 = CYLINDRICAL_SURFACE ( 'NONE', #7449, 4.999999999999998224 ) ;
#43584 = CARTESIAN_POINT ( 'NONE',  ( 122.3830681442452857, -1.833838273342659697, -17.42832698103878286 ) ) ;
#43585 = CARTESIAN_POINT ( 'NONE',  ( 120.8514481442452961, -2.084020599724406786, -8.691656652584148546 ) ) ;
#43586 = ORIENTED_EDGE ( 'NONE', *, *, #24490, .F. ) ;
#43587 = CARTESIAN_POINT ( 'NONE',  ( 123.7022829359119811, -4.283928203966213211, -7.183505701512925334 ) ) ;
#43588 = CARTESIAN_POINT ( 'NONE',  ( 112.7395348109119766, -5.638512984488999180, -18.83840828888717311 ) ) ;
#43589 = CARTESIAN_POINT ( 'NONE',  ( 122.9503348109119827, -9.859900752359378018, -12.68260735090039759 ) ) ;
#43590 = ORIENTED_EDGE ( 'NONE', *, *, #35896, .T. ) ;
#43591 = CARTESIAN_POINT ( 'NONE',  ( 73.07463722459043254, -58.49647601156275556, -35.70688775835006368 ) ) ;
#43592 = CARTESIAN_POINT ( 'NONE',  ( 116.6536748109119941, 0.9020085738987339008, -11.91225656197089222 ) ) ;
#43593 = CARTESIAN_POINT ( 'NONE',  ( 112.0105358795247810, -0.7896495226426338832, -17.46756447353520159 ) ) ;
#43594 = CARTESIAN_POINT ( 'NONE',  ( 115.1787814775786387, -0.1624402480850797581, -16.17319339645315424 ) ) ;
#43595 = VERTEX_POINT ( 'NONE', #25592 ) ;
#43596 = ORIENTED_EDGE ( 'NONE', *, *, #18077, .T. ) ;
#43597 = CARTESIAN_POINT ( 'NONE',  ( 123.5743281442453139, -2.084020599724406786, -8.691656652584148546 ) ) ;
#43598 = ADVANCED_FACE ( 'NONE', ( #36059 ), #24566, .T. ) ;
#43599 = CARTESIAN_POINT ( 'NONE',  ( 119.3198281442452924, -9.859900752359374465, -12.68260735090039404 ) ) ;
#43600 = DIRECTION ( 'NONE',  ( -0.000000000000000000, -0.9284778069183721172, -0.3713878862591650232 ) ) ;
#43601 = EDGE_LOOP ( 'NONE', ( #5020, #10571 ) ) ;
#43602 = DIRECTION ( 'NONE',  ( 1.000000000000000000, 0.000000000000000000, 0.000000000000000000 ) ) ;
#43603 = DIRECTION ( 'NONE',  ( -0.2397535688815953248, -0.7732992861493835912, 0.5869637469634660931 ) ) ;
#43604 = CARTESIAN_POINT ( 'NONE',  ( 106.9404577545248145, -7.250697342233347165, -7.631215200338321125 ) ) ;
#43605 = CARTESIAN_POINT ( 'NONE',  ( 115.2922348109119781, -10.63000616557722466, -14.87417383870573495 ) ) ;
#43607 = CARTESIAN_POINT ( 'NONE',  ( 117.6747548109119919, -7.643976991954077427, -18.09477374809248928 ) ) ;
#43606 = CARTESIAN_POINT ( 'NONE',  ( 114.7816948109119863, 0.5811942927096154232, -14.16772938898807155 ) ) ;
#43608 =( BOUNDED_CURVE ( )  B_SPLINE_CURVE ( 2, ( #16896, #2513, #13473, #44935, #6167, #9594, #16439, #13693, #30561, #27602, #41516, #10272, #6847, #20755, #13247, #26918, #23510 ),
 .UNSPECIFIED., .F., .F. ) 
 B_SPLINE_CURVE_WITH_KNOTS ( ( 3, 2, 2, 2, 2, 2, 2, 2, 3 ),
 ( 0.7589135524044680059, 0.7812500000000000000, 0.8125000000000000000, 0.8437500000000000000, 0.8750000000000000000, 0.9062500000000000000, 0.9375000000000000000, 0.9687500000000000000, 0.9910864475955319941 ),
 .UNSPECIFIED. ) 
 CURVE ( )  GEOMETRIC_REPRESENTATION_ITEM ( )  RATIONAL_B_SPLINE_CURVE ( ( 0.9689618144536780164, 0.9455916533437099813, 1.000000000000000000, 0.9238795325112869605, 1.000000000000000000, 0.9238795325112869605, 1.000000000000000000, 0.9238795325112869605, 1.000000000000000000, 0.9238795325112869605, 1.000000000000000000, 0.9238795325112869605, 1.000000000000000000, 0.9238795325112869605, 1.000000000000000000, 0.9455916533437099813, 0.9689618144536780164 ) ) 
 REPRESENTATION_ITEM ( '' )  );
#43609 = CARTESIAN_POINT ( 'NONE',  ( 120.4543614775786295, -5.574606645277164318, -18.38911715685844683 ) ) ;
#43610 = CARTESIAN_POINT ( 'NONE',  ( 111.8886348109120092, -3.383040157471821630, -19.15922257007629170 ) ) ;
#43611 = ORIENTED_EDGE ( 'NONE', *, *, #1593, .F. ) ;
#43612 = CARTESIAN_POINT ( 'NONE',  ( 118.5823814775786360, -7.643976991954077427, -18.09477374809248928 ) ) ;
#43613 = B_SPLINE_CURVE_WITH_KNOTS ( 'NONE', 3,
 ( #25547, #14381, #31922, #35101, #32373, #4332, #18484, #28970, #14157, #7306, #42430, #28074, #24646, #1140, #21224 ),
 .UNSPECIFIED., .F., .F.,
 ( 4, 2, 2, 1, 1, 1, 2, 2, 4 ),
 ( 0.000000000000000000, 0.2500000000001339484, 0.3750000000001929013, 0.4375000000002189915, 0.4687500000002216560, 0.4843750000002229883, 0.4921875000002237099, 0.5000000000002243761, 1.000000000000000000 ),
 .UNSPECIFIED. ) ;
#43614 = CARTESIAN_POINT ( 'NONE',  ( 120.8637602976252055, -8.580000213326620440, -17.71054824844518905 ) ) ;
#43615 = CARTESIAN_POINT ( 'NONE',  ( 113.0523327545247838, -2.477300249445798297, -19.15521520033831138 ) ) ;
#43616 = DIRECTION ( 'NONE',  ( -0.2768435750659266059, -0.3568721902840680249, 0.8921882507333128709 ) ) ;
#43617 = CARTESIAN_POINT ( 'NONE',  ( 110.2047546295247855, -4.863998795839590272, -7.631215200338315796 ) ) ;
#43618 = CARTESIAN_POINT ( 'NONE',  ( 117.4478481442453131, 0.2603800115204892296, -16.42320221600525088 ) ) ;
#43619 = ORIENTED_EDGE ( 'NONE', *, *, #23139, .T. ) ;
#43620 = CARTESIAN_POINT ( 'NONE',  ( 121.0216281442452981, -1.561330072975668948, -17.79121239304076951 ) ) ;
#43621 = CARTESIAN_POINT ( 'NONE',  ( 115.4833430939976893, -2.236191541394345172, -18.14152338500401029 ) ) ;
#43622 = CARTESIAN_POINT ( 'NONE',  ( 105.7597546295248350, -4.863998795839590272, -7.631215200338315796 ) ) ;
#43623 = CARTESIAN_POINT ( 'NONE',  ( 118.5256548109119876, -0.4660016031367893996, -10.09054647747474043 ) ) ;
#43624 = CARTESIAN_POINT ( 'NONE',  ( 116.3700414775786527, -5.638512984488999180, -18.83840828888717311 ) ) ;
#43625 = CARTESIAN_POINT ( 'NONE',  ( 123.2976082044368127, -6.247802574075781656, -18.73351920797576042 ) ) ;
#43626 = CARTESIAN_POINT ( 'NONE',  ( 120.4315948253203032, -6.059724811980584214, -18.37735133589801606 ) ) ;
#43627 = VERTEX_POINT ( 'NONE', #25147 ) ;
#43628 = CARTESIAN_POINT ( 'NONE',  ( 83.82415148905927538, -46.76310523276723785, -6.893215200338315363 ) ) ;
#43629 = CARTESIAN_POINT ( 'NONE',  ( 109.2294539694104287, -9.998871404483669068, -15.31448480652960242 ) ) ;
#43630 = CARTESIAN_POINT ( 'NONE',  ( 121.3619881442452879, -5.574606645277164318, -18.38911715685844683 ) ) ;
#43631 = CARTESIAN_POINT ( 'NONE',  ( 112.5661608795247872, -1.325403438956436419, -16.93181055722141792 ) ) ;
#43632 = CARTESIAN_POINT ( 'NONE',  ( 110.4825671295247815, 0.1403307496149613920, -13.39321520033831447 ) ) ;
#43634 = AXIS2_PLACEMENT_3D ( 'NONE', #21972, #23101, #16722 ) ;
#43633 = CARTESIAN_POINT ( 'NONE',  ( 118.6958348109119754, -3.505236298600246325, -18.68346056562440793 ) ) ;
#43635 = DIRECTION ( 'NONE',  ( -1.000000000000000000, 0.000000000000000000, 0.000000000000000000 ) ) ;
#43636 = CARTESIAN_POINT ( 'NONE',  ( 69.22226139490459218, -26.09593875132798857, -5.871463680831255694 ) ) ;
#43637 = CARTESIAN_POINT ( 'NONE',  ( 112.8529881442453160, -7.894159318335828068, -9.358103419637847864 ) ) ;
#43638 = CARTESIAN_POINT ( 'NONE',  ( 124.7088614775786226, 0.2603800115204892296, -16.42320221600525088 ) ) ;
#43639 = ORIENTED_EDGE ( 'NONE', *, *, #9118, .F. ) ;
#43640 = CARTESIAN_POINT ( 'NONE',  ( 117.3911214775786505, -7.894159318335828068, -9.358103419637847864 ) ) ;
#43641 = CARTESIAN_POINT ( 'NONE',  ( 114.2144281442453178, -8.166667518702817929, -8.995218007635859436 ) ) ;
#43642 = CARTESIAN_POINT ( 'NONE',  ( 121.0783548109119749, 0.2603800115204892296, -16.42320221600525088 ) ) ;
#43643 = CARTESIAN_POINT ( 'NONE',  ( 122.9503348109119827, -9.859900752359378018, -12.68260735090039759 ) ) ;
#43644 = EDGE_LOOP ( 'NONE', ( #30891, #13709, #9562, #40571, #38326, #17778, #12330, #21725, #6844, #39276, #17789 ) ) ;
#43645 = DIRECTION ( 'NONE',  ( -0.8636456077245080465, 0.5040994586965603652, 0.000000000000000000 ) ) ;
#43646 = CARTESIAN_POINT ( 'NONE',  ( 124.3117748109119844, -10.30919188438810075, -12.61870101168855918 ) ) ;
#43647 = CARTESIAN_POINT ( 'NONE',  ( 112.7395348109119766, -4.153390946401321671, -8.397313243818183892 ) ) ;
#43648 = CARTESIAN_POINT ( 'NONE',  ( 124.0281414775786146, -1.834011780172310813, -8.268836392978581529 ) ) ;
#43649 = CARTESIAN_POINT ( 'NONE',  ( 106.1070202545248407, -10.62599879583958717, -15.77991374673208469 ) ) ;
#43650 = CARTESIAN_POINT ( 'NONE',  ( 67.08264006073221708, -20.21382323020432992, -15.89321520033831447 ) ) ;
#43651 = CARTESIAN_POINT ( 'NONE',  ( 138.2184548109120499, -2.342207185915014644, -15.50236782978752537 ) ) ;
#43652 = CARTESIAN_POINT ( 'NONE',  ( 109.0240515045248202, -6.936859964151250502, -18.39754474579286025 ) ) ;
#43653 = AXIS2_PLACEMENT_3D ( 'NONE', #44072, #37434, #12836 ) ;
#43654 = CARTESIAN_POINT ( 'NONE',  ( 123.6328298109119714, -7.200787124940443817, -17.81845355600750835 ) ) ;
#43655 = AXIS2_PLACEMENT_3D ( 'NONE', #39866, #15470, #15698 ) ;
#43656 = CARTESIAN_POINT ( 'NONE',  ( 136.7036351579054383, -10.11817554825837639, -11.31345360030072023 ) ) ;
#43657 = CARTESIAN_POINT ( 'NONE',  ( 120.2274548109119934, -9.859900752359374465, -12.68260735090039404 ) ) ;
#43658 = CARTESIAN_POINT ( 'NONE',  ( 125.3328548109119964, -9.261995988541697145, -16.69588392320189030 ) ) ;
#43659 = DIRECTION ( 'NONE',  ( 1.000000000000000000, 0.000000000000000000, 0.000000000000000000 ) ) ;
#43660 = VERTEX_POINT ( 'NONE', #35608 ) ;
#43661 = CARTESIAN_POINT ( 'NONE',  ( 116.7333483795247844, -8.402594152722688392, -16.93181055722141792 ) ) ;
#43662 = CARTESIAN_POINT ( 'NONE',  ( 108.1906140045248037, 0.1403307496149616695, -15.46607636864997204 ) ) ;
#43663 = CARTESIAN_POINT ( 'NONE',  ( 116.1431348109119881, 0.1319031606808879209, -14.10382304977623669 ) ) ;
#43664 = CARTESIAN_POINT ( 'NONE',  ( 71.31713442278437753, 2.423123680056944007, -10.89321520033831447 ) ) ;
#43665 = ADVANCED_FACE ( 'NONE', ( #43367, #15324 ), #22611, .F. ) ;
#43666 = DIRECTION ( 'NONE',  ( 1.000000000000000000, 0.000000000000000000, 0.000000000000000000 ) ) ;
#43667 = CARTESIAN_POINT ( 'NONE',  ( 122.6695390828414105, -8.372502050422333753, -17.31760344562334808 ) ) ;
#43669 = CARTESIAN_POINT ( 'NONE',  ( 121.9292548109119849, -1.561330072975668948, -17.79121239304076951 ) ) ;
#43668 = CARTESIAN_POINT ( 'NONE',  ( 70.09311708302951160, -26.31909214926311691, -5.693345267502175844 ) ) ;
#43670 = CARTESIAN_POINT ( 'NONE',  ( 123.7445081442452874, -7.894159318335828068, -9.358103419637847864 ) ) ;
#43671 = ORIENTED_EDGE ( 'NONE', *, *, #5904, .F. ) ;
#43672 = FACE_OUTER_BOUND ( 'NONE', #27247, .T. ) ;
#43673 = CARTESIAN_POINT ( 'NONE',  ( 78.69189222814998175, -69.76310523276724496, 3.106784799661685526 ) ) ;
#43674 = CARTESIAN_POINT ( 'NONE',  ( 109.3713171295247832, 0.1403307496149613920, -13.39321520033831447 ) ) ;
#43675 = CARTESIAN_POINT ( 'NONE',  ( 121.3619881442452879, -5.574606645277164318, -18.38911715685844683 ) ) ;
#43676 = CARTESIAN_POINT ( 'NONE',  ( 121.4187148109119789, -3.505236298600246325, -18.68346056562440793 ) ) ;
#43677 = CARTESIAN_POINT ( 'NONE',  ( 119.6811727111058588, -1.267766418764730840, -16.93314635290706605 ) ) ;
#43678 = CARTESIAN_POINT ( 'NONE',  ( 107.9822546295247889, -4.863998795839590272, -7.631215200338315796 ) ) ;
#43679 = DIRECTION ( 'NONE',  ( 0.000000000000000000, 0.000000000000000000, -1.000000000000000000 ) ) ;
#43680 = FACE_OUTER_BOUND ( 'NONE', #38006, .T. ) ;
#43681 = CARTESIAN_POINT ( 'NONE',  ( 76.69189222814998175, -49.76310523276720232, -19.39321520033831447 ) ) ;
#43682 = CARTESIAN_POINT ( 'NONE',  ( 111.7327233795247849, -8.938348069036489818, -17.46756447353520159 ) ) ;
#43683 = ADVANCED_FACE ( 'NONE', ( #4382 ), #24526, .F. ) ;
#43684 = CARTESIAN_POINT ( 'NONE',  ( -13.78505786849313886, -3.796669023460156556, -17.89321520033824697 ) ) ;
#43685 = CARTESIAN_POINT ( 'NONE',  ( 115.4137390045248566, 0.8980012041604421569, -15.77991374673208469 ) ) ;
#43686 = CARTESIAN_POINT ( 'NONE',  ( 121.7023481442452777, -9.261995988541697145, -16.69588392320189030 ) ) ;
#43687 = CARTESIAN_POINT ( 'NONE',  ( 122.7234281442452755, -5.638512984488999180, -18.83840828888717311 ) ) ;
#43688 = CARTESIAN_POINT ( 'NONE',  ( 106.9404577545248145, -7.250697342233347165, -7.631215200338321125 ) ) ;
#43689 = CARTESIAN_POINT ( 'NONE',  ( 115.1787814775786387, -9.988377603198976828, -10.36322818467138340 ) ) ;
#43690 = EDGE_CURVE ( 'NONE', #4544, #2844, #6866, .T. ) ;
#43691 = EDGE_CURVE ( 'NONE', #10336, #3754, #38305, .T. ) ;
#43692 = DIRECTION ( 'NONE',  ( 0.7871354856660198740, 0.4483307682966886643, 0.4235767337848242442 ) ) ;
#43693 = ORIENTED_EDGE ( 'NONE', *, *, #35105, .T. ) ;
#43694 = CARTESIAN_POINT ( 'NONE',  ( 116.1808983795247769, -1.328464889906837199, -9.857681294405580275 ) ) ;
#43695 = CARTESIAN_POINT ( 'NONE',  ( 121.2485348109119769, -0.4660016031367893996, -10.09054647747474043 ) ) ;
#43696 = CARTESIAN_POINT ( 'NONE',  ( 119.9438214775786378, -7.893985811506177619, -18.51759400769804742 ) ) ;
#43697 = AXIS2_PLACEMENT_3D ( 'NONE', #23956, #37838, #6615 ) ;
#43698 = CARTESIAN_POINT ( 'NONE',  ( 126.5241148109119393, -9.565557343593413364, -10.61323700422348004 ) ) ;
#43699 = SHAPE_DEFINITION_REPRESENTATION ( #831, #26250 ) ;
#43700 = CARTESIAN_POINT ( 'NONE',  ( 112.5693548109119888, 0.4262465694468514643, -12.03445270309931736 ) ) ;
#43701 = CARTESIAN_POINT ( 'NONE',  ( 112.9664414775786412, -9.859900752359374465, -12.68260735090039404 ) ) ;
#43702 = CARTESIAN_POINT ( 'NONE',  ( 124.3685014775786328, -10.63000616557722466, -14.87417383870573495 ) ) ;
#43703 = B_SPLINE_CURVE_WITH_KNOTS ( 'NONE', 3,
 ( #26841, #43946, #40527, #33653 ),
 .UNSPECIFIED., .F., .F.,
 ( 4, 4 ),
 ( 0.000000000000000000, 1.000000000000000000 ),
 .UNSPECIFIED. ) ;
#43704 = CARTESIAN_POINT ( 'NONE',  ( 109.7185827545247889, -2.477300249445798297, -19.15521520033831138 ) ) ;
#43705 = AXIS2_PLACEMENT_3D ( 'NONE', #8356, #26131, #36603 ) ;
#43706 = CARTESIAN_POINT ( 'NONE',  ( 120.0005481442453146, -4.153390946401325223, -8.397313243818185668 ) ) ;
#43707 = CARTESIAN_POINT ( 'NONE',  ( 110.3436608795247764, -8.938348069036489818, -9.318865927141430916 ) ) ;
#43708 = B_SPLINE_CURVE_WITH_KNOTS ( 'NONE', 3,
 ( #22288, #28689, #32318, #32973, #12261, #7926, #39620, #8825, #40062, #36182 ),
 .UNSPECIFIED., .F., .F.,
 ( 4, 3, 3, 4 ),
 ( 6.254634441385499976E-18, 0.0002476486541971039844, 0.0004952973025691049819, 0.0009610892161188140746 ),
 .UNSPECIFIED. ) ;
#43709 = DIRECTION ( 'NONE',  ( 0.5735764363510498232, -0.3127926500124802445, 0.7570804645221007600 ) ) ;
#43710 = ORIENTED_EDGE ( 'NONE', *, *, #16992, .F. ) ;
#43711 = CIRCLE ( 'NONE', #24064, 2.445500000000004448 ) ;
#43712 = CARTESIAN_POINT ( 'NONE',  ( 123.2855641859119942, -8.321307733199551748, -9.223433127585318303 ) ) ;
#43713 = CARTESIAN_POINT ( 'NONE',  ( 124.0848681442452772, -4.089484607189486809, -7.948022111789456723 ) ) ;
#43714 = EDGE_CURVE ( 'NONE', #38815, #32422, #534, .T. ) ;
#43715 = LINE ( 'NONE', #16814, #8749 ) ;
#43716 = CARTESIAN_POINT ( 'NONE',  ( 125.3563494635826743, 1.791320624781802318, -11.07214261843091663 ) ) ;
#43717 = LINE ( 'NONE', #15221, #44222 ) ;
#43718 = B_SPLINE_CURVE_WITH_KNOTS ( 'NONE', 3,
 ( #10147, #30436, #41165, #3067, #37493, #44131, #6495, #41394, #44355, #20633 ),
 .UNSPECIFIED., .F., .F.,
 ( 4, 3, 3, 4 ),
 ( 0.000000000000000000, 0.0002476486447139085055, 0.0004952972925464399923, 0.0009604418836934780143 ),
 .UNSPECIFIED. ) ;
#43719 = CARTESIAN_POINT ( 'NONE',  ( 119.4900081442453086, -7.643976991954077427, -18.09477374809248928 ) ) ;
#43720 = CARTESIAN_POINT ( 'NONE',  ( 67.59280524186679884, -0.2640895998874671635, -16.39321520033831447 ) ) ;
#43721 = DIRECTION ( 'NONE',  ( -0.9908103287288504424, 0.1352586133457951423, 0.000000000000000000 ) ) ;
#43722 = EDGE_CURVE ( 'NONE', #15763, #34483, #7325, .T. ) ;
#43723 = CARTESIAN_POINT ( 'NONE',  ( 123.1772414775786189, -5.574606645277164318, -18.38911715685844683 ) ) ;
#43724 = CARTESIAN_POINT ( 'NONE',  ( 70.19189222814998175, -54.83461124330791847, -35.13666250696951465 ) ) ;
#43725 = CARTESIAN_POINT ( 'NONE',  ( 123.5176014775786228, -0.8288870151387760510, -10.36305467784173118 ) ) ;
#43726 = ADVANCED_FACE ( 'NONE', ( #8374 ), #5165, .T. ) ;
#43727 = CARTESIAN_POINT ( 'NONE',  ( 125.2293180859949899, -12.02800175804190630, -14.77921087193282546 ) ) ;
#43728 = CARTESIAN_POINT ( 'NONE',  ( 125.2194014775786286, -10.30919188438810075, -12.61870101168855918 ) ) ;
#43729 = CARTESIAN_POINT ( 'NONE',  ( 118.3554748109119998, -9.565557343593413364, -10.61323700422348004 ) ) ;
#43730 = CARTESIAN_POINT ( 'NONE',  ( 125.7299414775786346, -10.15424416112533912, -14.75197769757731336 ) ) ;
#43731 = EDGE_LOOP ( 'NONE', ( #29017, #21269, #43671, #44045 ) ) ;
#43732 = CARTESIAN_POINT ( 'NONE',  ( 124.7088614775786226, 0.2603800115204892296, -16.42320221600525088 ) ) ;
#43733 = CARTESIAN_POINT ( 'NONE',  ( 113.9307948109119906, 0.9020085738987339008, -11.91225656197089222 ) ) ;
#43734 = CARTESIAN_POINT ( 'NONE',  ( 114.0941296295247867, -4.863998795839590272, -8.388885654883775800 ) ) ;
#43735 = CARTESIAN_POINT ( 'NONE',  ( 138.2184548109119930, -11.79424454490141017, -12.40746986932944473 ) ) ;
#43736 = CARTESIAN_POINT ( 'NONE',  ( 124.9357681442453014, -7.643976991954077427, -18.09477374809248928 ) ) ;
#43737 = CARTESIAN_POINT ( 'NONE',  ( 123.2339681442453241, -6.344957434206665248, -7.627207830600338134 ) ) ;
#43738 = CARTESIAN_POINT ( 'NONE',  ( 116.5249890045247980, 0.8980012041604421569, -15.77991374673208469 ) ) ;
#43739 = CARTESIAN_POINT ( 'NONE',  ( 110.2742077545248094, -2.791137627527939813, -18.39754474579286025 ) ) ;
#43740 = FACE_OUTER_BOUND ( 'NONE', #41085, .T. ) ;
#43741 = DIRECTION ( 'NONE',  ( 0.8636456077245086016, -0.5040994586965593660, 0.000000000000000000 ) ) ;
#43742 = AXIS2_PLACEMENT_3D ( 'NONE', #338, #42077, #24732 ) ;
#43743 = DIRECTION ( 'NONE',  ( 1.000000000000000000, 0.000000000000000000, -0.000000000000000000 ) ) ;
#43744 = CARTESIAN_POINT ( 'NONE',  ( 111.9410827545248708, -6.936859964151250502, -8.388885654883777576 ) ) ;
#43745 = ORIENTED_EDGE ( 'NONE', *, *, #42664, .T. ) ;
#43746 = AXIS2_PLACEMENT_3D ( 'NONE', #26471, #38017, #6793 ) ;
#43747 = ADVANCED_FACE ( 'NONE', ( #12479, #22281 ), #43939, .F. ) ;
#43748 = CARTESIAN_POINT ( 'NONE',  ( 123.7445081442452874, -7.894159318335828068, -9.358103419637847864 ) ) ;
#43749 = CARTESIAN_POINT ( 'NONE',  ( 123.7717360609119623, -6.564341423271550902, -7.887810678476487425 ) ) ;
#43750 = CARTESIAN_POINT ( 'NONE',  ( 120.6463454359119822, -11.07370829466463569, -12.81314460846529002 ) ) ;
#43751 = EDGE_CURVE ( 'NONE', #35294, #13294, #9272, .T. ) ;
#43752 = EDGE_CURVE ( 'NONE', #41400, #36736, #43158, .T. ) ;
#43753 = VERTEX_POINT ( 'NONE', #32746 ) ;
#43754 = CARTESIAN_POINT ( 'NONE',  ( 70.19189222814998175, -100.0979043305785581, -53.24182196210380624 ) ) ;
#43755 = CARTESIAN_POINT ( 'NONE',  ( 105.2041296295248287, -4.863998795839590272, -8.388885654883775800 ) ) ;
#43756 = ORIENTED_EDGE ( 'NONE', *, *, #38937, .F. ) ;
#43757 = CARTESIAN_POINT ( 'NONE',  ( 119.7169148109119874, -9.988377603198976828, -10.36322818467138340 ) ) ;
#43758 = CARTESIAN_POINT ( 'NONE',  ( 124.4819548109119722, -2.084020599724406786, -8.691656652584148546 ) ) ;
#43759 = CARTESIAN_POINT ( 'NONE',  ( 115.4056881442453459, -2.084020599724406786, -8.691656652584148546 ) ) ;
#43760 = CARTESIAN_POINT ( 'NONE',  ( 116.2443561498677269, -2.324775150319240868, -18.02356106541842351 ) ) ;
#43761 = CARTESIAN_POINT ( 'NONE',  ( 114.8056076054816259, -2.287189184988692059, -18.07361239780447448 ) ) ;
#43762 = CARTESIAN_POINT ( 'NONE',  ( 115.1220548109119761, -8.166667518702817929, -8.995218007635861213 ) ) ;
#43763 = CARTESIAN_POINT ( 'NONE',  ( 111.1770983795247787, -8.402594152722688392, -16.93181055722141792 ) ) ;
#43764 = AXIS2_PLACEMENT_3D ( 'NONE', #40316, #32337, #15021 ) ;
#43765 = CARTESIAN_POINT ( 'NONE',  ( 124.5386814775786206, -5.638512984488999180, -18.83840828888717311 ) ) ;
#43766 = DIRECTION ( 'NONE',  ( 0.000000000000000000, 0.9284778069183720062, 0.3713878862591650232 ) ) ;
#43767 = EDGE_LOOP ( 'NONE', ( #33692, #34386, #18966, #41837 ) ) ;
#43768 = CARTESIAN_POINT ( 'NONE',  ( 116.0864081442453113, -9.988377603198976828, -10.36322818467138340 ) ) ;
#43769 = CARTESIAN_POINT ( 'NONE',  ( 114.0442481442453300, -7.643976991954077427, -18.09477374809248928 ) ) ;
#43770 = CARTESIAN_POINT ( 'NONE',  ( 94.20708369096698220, -25.99489077589524300, -13.39321520033831447 ) ) ;
#43771 = CARTESIAN_POINT ( 'NONE',  ( 112.2857214775786474, -4.089484607189486809, -7.948022111789456723 ) ) ;
#43772 = VERTEX_POINT ( 'NONE', #40054 ) ;
#43773 = CONICAL_SURFACE ( 'NONE', #11744, 2.999999999999999556, 0.9599310885968830309 ) ;
#43774 = CARTESIAN_POINT ( 'NONE',  ( 122.8936081442453059, 0.2603800115204892296, -16.42320221600525088 ) ) ;
#43775 = CARTESIAN_POINT ( 'NONE',  ( 85.70478001548416103, -25.23119213852205789, -15.24166438581092109 ) ) ;
#43776 = CARTESIAN_POINT ( 'NONE',  ( 67.30914723170953096, -56.95110010363538322, -36.87775856471080260 ) ) ;
#43777 = AXIS2_PLACEMENT_3D ( 'NONE', #7753, #22114, #7523 ) ;
#43778 = CARTESIAN_POINT ( 'NONE',  ( 82.31000308962319423, -13.76004065658516673, -9.893215200338316251 ) ) ;
#43779 = CARTESIAN_POINT ( 'NONE',  ( 137.0596819398155617, -3.051825027028553627, -8.284924315246177784 ) ) ;
#43780 = CARTESIAN_POINT ( 'NONE',  ( 114.1577014775786552, -3.505236298600246325, -18.68346056562440793 ) ) ;
#43781 = CARTESIAN_POINT ( 'NONE',  ( 86.36631847702263087, -25.99489077589524300, -13.39321520033831447 ) ) ;
#43782 = CARTESIAN_POINT ( 'NONE',  ( 125.2070578882556475, -3.534371629016498151, -20.61203076238330567 ) ) ;
#43783 = CARTESIAN_POINT ( 'NONE',  ( 112.7395348109119766, -4.153390946401321671, -8.397313243818183892 ) ) ;
#43784 = CARTESIAN_POINT ( 'NONE',  ( 113.5904348109119866, -7.893985811506177619, -18.51759400769804742 ) ) ;
#43785 = CARTESIAN_POINT ( 'NONE',  ( 123.8411891859119862, -1.406689858478933353, -17.56299727309130887 ) ) ;
#43786 = CARTESIAN_POINT ( 'NONE',  ( 112.6260814775786514, -9.261995988541697145, -16.69588392320189030 ) ) ;
#43787 = CARTESIAN_POINT ( 'NONE',  ( 114.5547881442453217, -4.153390946401321671, -8.397313243818183892 ) ) ;
#43788 = CARTESIAN_POINT ( 'NONE',  ( 122.7801548109119665, -3.383040157471821630, -19.15922257007629170 ) ) ;
#43789 = EDGE_CURVE ( 'NONE', #28148, #44662, #16198, .T. ) ;
#43790 = CARTESIAN_POINT ( 'NONE',  ( 123.3474214775786209, -9.988377603198976828, -10.36322818467138340 ) ) ;
#43791 = VERTEX_POINT ( 'NONE', #19990 ) ;
#43792 = CARTESIAN_POINT ( 'NONE',  ( 113.8173414775786512, 0.2603800115204892296, -16.42320221600525088 ) ) ;
#43793 = CARTESIAN_POINT ( 'NONE',  ( 113.0523327545247838, -2.477300249445798297, -19.15521520033831138 ) ) ;
#43794 = CARTESIAN_POINT ( 'NONE',  ( 109.7185827545247889, -6.936859964151250502, -8.388885654883777576 ) ) ;
#43795 = CARTESIAN_POINT ( 'NONE',  ( 109.3018640045248304, 0.1403307496149616695, -15.46607636864997204 ) ) ;
#43796 = AXIS2_PLACEMENT_3D ( 'NONE', #20842, #16987, #6935 ) ;
#43797 = CARTESIAN_POINT ( 'NONE',  ( 64.53707254195585108, -37.45440240364068529, -5.176427727597975093 ) ) ;
#43798 = CARTESIAN_POINT ( 'NONE',  ( 119.2631014775786298, 0.2603800115204892296, -16.42320221600525088 ) ) ;
#43799 = VERTEX_POINT ( 'NONE', #30701 ) ;
#43800 = LINE ( 'NONE', #12565, #28900 ) ;
#43801 = CARTESIAN_POINT ( 'NONE',  ( 124.1884548109119777, -2.527210466738037731, -8.967976844669125924 ) ) ;
#43802 = CARTESIAN_POINT ( 'NONE',  ( 85.04324155394569118, -25.23119213852205789, -15.24166438581092109 ) ) ;
#43803 = CARTESIAN_POINT ( 'NONE',  ( 113.3635281442453504, -0.1624402480850797581, -16.17319339645315424 ) ) ;
#43804 = CARTESIAN_POINT ( 'NONE',  ( 106.1070202545248407, 0.1403307496149616695, -11.32035403202665336 ) ) ;
#43805 = CARTESIAN_POINT ( 'NONE',  ( 120.6245414775786458, -9.988377603198976828, -10.36322818467138340 ) ) ;
#43806 = CARTESIAN_POINT ( 'NONE',  ( 109.7185827545247889, -2.477300249445798297, -19.15521520033831138 ) ) ;
#43807 = DIRECTION ( 'NONE',  ( 1.000000000000000000, 0.000000000000000000, 0.000000000000000000 ) ) ;
#43808 = ORIENTED_EDGE ( 'NONE', *, *, #30047, .T. ) ;
#43809 = DIRECTION ( 'NONE',  ( 0.9848077530122080203, -0.1736481776669309973, 0.000000000000000000 ) ) ;
#43810 = AXIS2_PLACEMENT_3D ( 'NONE', #1164, #18945, #43345 ) ;
#43811 = CARTESIAN_POINT ( 'NONE',  ( 121.1918081442452859, -10.15424416112533912, -14.75197769757731336 ) ) ;
#43812 = CARTESIAN_POINT ( 'NONE',  ( 118.1852948109119836, -5.638512984488999180, -18.83840828888717311 ) ) ;
#43813 = CARTESIAN_POINT ( 'NONE',  ( 114.6682414775786469, -7.894159318335828068, -9.358103419637847864 ) ) ;
#43814 = CARTESIAN_POINT ( 'NONE',  ( 115.8595014775786609, -1.834011780172310813, -8.268836392978581529 ) ) ;
#43815 = FACE_OUTER_BOUND ( 'NONE', #24642, .T. ) ;
#43816 = ADVANCED_FACE ( 'NONE', ( #3329 ), #13636, .F. ) ;
#43817 = CARTESIAN_POINT ( 'NONE',  ( 122.8368814775786291, -7.894159318335828068, -9.358103419637847864 ) ) ;
#43818 = CARTESIAN_POINT ( 'NONE',  ( 118.5823814775786360, -7.643976991954077427, -18.09477374809248928 ) ) ;
#43819 = ORIENTED_EDGE ( 'NONE', *, *, #9602, .F. ) ;
#43820 =( GEOMETRIC_REPRESENTATION_CONTEXT ( 3 ) GLOBAL_UNCERTAINTY_ASSIGNED_CONTEXT ( ( #14645 ) ) GLOBAL_UNIT_ASSIGNED_CONTEXT ( ( #31677, #40907, #44549 ) ) REPRESENTATION_CONTEXT ( 'NONE', 'WORKASPACE' ) );
#43821 = CARTESIAN_POINT ( 'NONE',  ( 123.0077516859119839, -9.665098340737509730, -17.37397104707595474 ) ) ;
#43822 = CARTESIAN_POINT ( 'NONE',  ( 112.1722681442453222, -0.4660016031367893996, -10.09054647747474043 ) ) ;
#43823 = CARTESIAN_POINT ( 'NONE',  ( 120.5110881442453206, -3.505236298600246325, -18.68346056562440793 ) ) ;
#43824 = ORIENTED_EDGE ( 'NONE', *, *, #5061, .T. ) ;
#43825 = CARTESIAN_POINT ( 'NONE',  ( 123.2855641859119942, -8.321307733199551748, -9.223433127585318303 ) ) ;
#43826 = CARTESIAN_POINT ( 'NONE',  ( 118.0718414775786300, -9.261995988541697145, -16.69588392320189030 ) ) ;
#43827 = CARTESIAN_POINT ( 'NONE',  ( 111.8021765045248372, -7.250697342233347165, -19.15521520033831138 ) ) ;
#43828 = CARTESIAN_POINT ( 'NONE',  ( 115.2355081442453155, 0.1319031606808879209, -14.10382304977623669 ) ) ;
#43829 = ORIENTED_EDGE ( 'NONE', *, *, #44643, .T. ) ;
#43830 = ORIENTED_EDGE ( 'NONE', *, *, #7604, .F. ) ;
#43831 = CONICAL_SURFACE ( 'NONE', #25637, 3077.683537175320453, 1.256637061435923686 ) ;
#43832 = CARTESIAN_POINT ( 'NONE',  ( 124.7655881442452852, -9.859900752359378018, -12.68260735090039759 ) ) ;
#43833 = CARTESIAN_POINT ( 'NONE',  ( 119.4332814775786318, -8.899110576539710493, -16.42337572283490132 ) ) ;
#43834 = CARTESIAN_POINT ( 'NONE',  ( 66.50565249108366572, -35.53029877516337365, -14.39321520033831625 ) ) ;
#43835 = ORIENTED_EDGE ( 'NONE', *, *, #35841, .T. ) ;
#43836 = CARTESIAN_POINT ( 'NONE',  ( 119.4332814775786318, -0.4660016031367893996, -10.09054647747474043 ) ) ;
#43837 = CARTESIAN_POINT ( 'NONE',  ( 106.2459265045248173, -7.250697342233347165, -19.15521520033831138 ) ) ;
#43838 = AXIS2_PLACEMENT_3D ( 'NONE', #42161, #39176, #42609 ) ;
#43839 = CARTESIAN_POINT ( 'NONE',  ( 117.3343948109119737, -3.383040157471821630, -19.15922257007629170 ) ) ;
#43841 = CARTESIAN_POINT ( 'NONE',  ( 116.1998614775786507, 0.4262465694468514643, -12.03445270309931736 ) ) ;
#43840 = CARTESIAN_POINT ( 'NONE',  ( 116.7671281442453335, -1.834011780172310813, -8.268836392978581529 ) ) ;
#43842 = CARTESIAN_POINT ( 'NONE',  ( 125.1626748109119802, -0.1624402480850797581, -16.17319339645315424 ) ) ;
#43843 = CARTESIAN_POINT ( 'NONE',  ( 113.8173414775786512, 0.2603800115204892296, -16.42320221600525088 ) ) ;
#43844 = ORIENTED_EDGE ( 'NONE', *, *, #29504, .F. ) ;
#43845 = CARTESIAN_POINT ( 'NONE',  ( 123.1205148109119563, -7.643976991954077427, -18.09477374809248928 ) ) ;
#43846 = CARTESIAN_POINT ( 'NONE',  ( 138.2184548109119930, -5.044325091639137781, -11.90409383958792411 ) ) ;
#43847 = CARTESIAN_POINT ( 'NONE',  ( 83.46705746533213244, -32.83968548964498524, -23.89321520033831803 ) ) ;
#43848 = CARTESIAN_POINT ( 'NONE',  ( 113.9552233795247815, -8.938348069036489818, -17.46756447353520159 ) ) ;
#43849 = CARTESIAN_POINT ( 'NONE',  ( 113.3995983795247895, -8.402594152722688392, -16.93181055722141792 ) ) ;
#43850 = CARTESIAN_POINT ( 'NONE',  ( 111.0381921295247878, 0.8980012041604618078, -13.39321520033831447 ) ) ;
#43851 = CARTESIAN_POINT ( 'NONE',  ( 118.9794681442453026, -9.261995988541697145, -16.69588392320189030 ) ) ;
#43852 = ORIENTED_EDGE ( 'NONE', *, *, #24744, .T. ) ;
#43853 = CARTESIAN_POINT ( 'NONE',  ( 120.4543614775786295, -4.089484607189486809, -7.948022111789456723 ) ) ;
#43854 = CARTESIAN_POINT ( 'NONE',  ( 112.7395348109119766, -4.153390946401321671, -8.397313243818183892 ) ) ;
#43855 = CARTESIAN_POINT ( 'NONE',  ( 107.7738952545248310, 0.8980012041604421569, -11.00651665394454071 ) ) ;
#43856 = CARTESIAN_POINT ( 'NONE',  ( 120.0572748109119772, -3.383040157471821630, -19.15922257007629170 ) ) ;
#43857 = CARTESIAN_POINT ( 'NONE',  ( 121.6456214775786293, -10.63000616557722466, -14.87417383870573495 ) ) ;
#43858 = CARTESIAN_POINT ( 'NONE',  ( 67.18674234710391602, -1.717770130243481574, -17.23327264932555281 ) ) ;
#43859 = CARTESIAN_POINT ( 'NONE',  ( 120.6075460087703988, -6.176492496456559955, -18.59847741292036716 ) ) ;
#43860 = VERTEX_POINT ( 'NONE', #44172 ) ;
#43861 = CARTESIAN_POINT ( 'NONE',  ( -3.049798262687883010, -7.199197394943047890, -7.393215200338317139 ) ) ;
#43862 = DIRECTION ( 'NONE',  ( 1.000000000000000000, 0.000000000000000000, -0.000000000000000000 ) ) ;
#43863 = CIRCLE ( 'NONE', #17650, 4.699999999999999289 ) ;
#43864 = CARTESIAN_POINT ( 'NONE',  ( 122.6099748109119929, -0.8288870151387760510, -10.36305467784173118 ) ) ;
#43865 = EDGE_CURVE ( 'NONE', #2517, #17793, #13397, .T. ) ;
#43866 = CARTESIAN_POINT ( 'NONE',  ( 111.2465515045248168, -6.936859964151250502, -18.39754474579286025 ) ) ;
#43867 = CARTESIAN_POINT ( 'NONE',  ( 109.9963952545248134, -9.868328341294098749, -15.46607636864997204 ) ) ;
#43868 = CARTESIAN_POINT ( 'NONE',  ( 116.5969481442453031, -9.859900752359374465, -12.68260735090039404 ) ) ;
#43869 = CARTESIAN_POINT ( 'NONE',  ( 86.34560043013698305, -9.320000780048239619, -18.64321520033831803 ) ) ;
#43870 = CARTESIAN_POINT ( 'NONE',  ( 69.20676056990819802, -25.74134712006483738, -5.871647083323465743 ) ) ;
#43871 = CARTESIAN_POINT ( 'NONE',  ( 111.5482748109120053, -0.1624402480850797581, -16.17319339645315424 ) ) ;
#43872 = CARTESIAN_POINT ( 'NONE',  ( 124.1983214775786166, -8.166667518702819706, -8.995218007635861213 ) ) ;
#43873 = VERTEX_POINT ( 'NONE', #33645 ) ;
#43874 = CARTESIAN_POINT ( 'NONE',  ( 122.5532481442453019, 0.4262465694468514643, -12.03445270309931736 ) ) ;
#43875 = AXIS2_PLACEMENT_3D ( 'NONE', #19821, #8881, #43542 ) ;
#43876 = CARTESIAN_POINT ( 'NONE',  ( 116.6536748109119941, 0.9020085738987339008, -11.91225656197089222 ) ) ;
#43877 = CARTESIAN_POINT ( 'NONE',  ( 122.5532481442453019, -10.63000616557722466, -14.87417383870573495 ) ) ;
#43878 = CARTESIAN_POINT ( 'NONE',  ( 121.7590748109119687, -2.084020599724406786, -8.691656652584148546 ) ) ;
#43879 = ORIENTED_EDGE ( 'NONE', *, *, #23426, .T. ) ;
#43880 = CARTESIAN_POINT ( 'NONE',  ( 91.38554522942851577, -25.99489077589524300, -13.39321520033831625 ) ) ;
#43881 = CARTESIAN_POINT ( 'NONE',  ( 124.2550481442452792, -9.988377603198980381, -10.36322818467138518 ) ) ;
#43882 = EDGE_CURVE ( 'NONE', #41097, #12584, #34720, .T. ) ;
#43883 = CARTESIAN_POINT ( 'NONE',  ( 112.9664414775786412, -9.859900752359374465, -12.68260735090039404 ) ) ;
#43884 = CARTESIAN_POINT ( 'NONE',  ( 111.8886348109120092, -6.222761293078241884, -8.102969835052219238 ) ) ;
#43885 = CARTESIAN_POINT ( 'NONE',  ( 108.7462390045248242, 0.8980012041604421569, -15.77991374673208469 ) ) ;
#43886 = FACE_OUTER_BOUND ( 'NONE', #938, .T. ) ;
#43887 = AXIS2_PLACEMENT_3D ( 'NONE', #4541, #32129, #1344 ) ;
#43888 = CARTESIAN_POINT ( 'NONE',  ( 127.9519950909192261, -3.021983423502168087, -14.59726296296260273 ) ) ;
#43889 = CARTESIAN_POINT ( 'NONE',  ( 107.5655358795247736, -8.402594152722688392, -9.854619843455216355 ) ) ;
#43890 = VECTOR ( 'NONE', #23572, 1000.000000000000000 ) ;
#43891 = CARTESIAN_POINT ( 'NONE',  ( 81.31761596104672662, -0.9606231062294252609, -12.39321520033831447 ) ) ;
#43892 = CARTESIAN_POINT ( 'NONE',  ( 120.7379948109119709, 0.4262465694468514643, -12.03445270309931736 ) ) ;
#43893 = CARTESIAN_POINT ( 'NONE',  ( 111.4915481442453142, -1.833838273342658365, -17.42832698103878286 ) ) ;
#43894 = CARTESIAN_POINT ( 'NONE',  ( 125.6164881442453094, -9.565557343593397377, -10.61323700422345695 ) ) ;
#43895 = ORIENTED_EDGE ( 'NONE', *, *, #126, .T. ) ;
#43896 = CARTESIAN_POINT ( 'NONE',  ( 116.3166296295247832, -4.863998795839590272, -8.388885654883775800 ) ) ;
#43897 =( GEOMETRIC_REPRESENTATION_CONTEXT ( 3 ) GLOBAL_UNCERTAINTY_ASSIGNED_CONTEXT ( ( #28784 ) ) GLOBAL_UNIT_ASSIGNED_CONTEXT ( ( #24795, #31629, #41912 ) ) REPRESENTATION_CONTEXT ( 'NONE', 'WORKASPACE' ) );
#43898 = CARTESIAN_POINT ( 'NONE',  ( 117.8449348109119938, -1.833838273342659253, -17.42832698103878286 ) ) ;
#43899 = CARTESIAN_POINT ( 'NONE',  ( 113.4769814775786330, 0.4262465694468514643, -12.03445270309931736 ) ) ;
#43900 = CARTESIAN_POINT ( 'NONE',  ( 67.40573139832108041, -0.1776877719995537119, -10.39321520033831625 ) ) ;
#43901 = CARTESIAN_POINT ( 'NONE',  ( -2.802086886829308732, -7.125079315770471489, -19.36905904446185289 ) ) ;
#43903 = CARTESIAN_POINT ( 'NONE',  ( 123.5743281442453139, -7.893985811506177619, -18.51759400769804742 ) ) ;
#43902 = CARTESIAN_POINT ( 'NONE',  ( 70.50211253258815702, -26.42392322955106465, -5.550474951698388892 ) ) ;
#43904 = CARTESIAN_POINT ( 'NONE',  ( 122.2696148109119889, -5.574606645277164318, -18.38911715685844683 ) ) ;
#43905 = ORIENTED_EDGE ( 'NONE', *, *, #36012, .F. ) ;
#43906 = CARTESIAN_POINT ( 'NONE',  ( 110.4384831777918805, -0.01829820670803256055, -14.64321520033831447 ) ) ;
#43907 = CARTESIAN_POINT ( 'NONE',  ( 126.2758031835812744, 0.06624046018700967264, -14.38341065059502455 ) ) ;
#43908 = CARTESIAN_POINT ( 'NONE',  ( 111.4549108795247747, -1.325403438956436419, -16.93181055722141792 ) ) ;
#43909 = CARTESIAN_POINT ( 'NONE',  ( 120.7379948109119709, 0.4262465694468514643, -12.03445270309931736 ) ) ;
#43910 = CARTESIAN_POINT ( 'NONE',  ( 119.6034614775786196, -3.505236298600246325, -18.68346056562440793 ) ) ;
#43911 = CARTESIAN_POINT ( 'NONE',  ( 119.2988998611595832, -1.036737761566197014, -17.24079555149560861 ) ) ;
#43912 = CARTESIAN_POINT ( 'NONE',  ( 112.9134265045247645, -2.791137627527939813, -8.388885654883777576 ) ) ;
#43913 = CARTESIAN_POINT ( 'NONE',  ( 116.7671281442453193, -1.834011780172314143, -8.268836392978577976 ) ) ;
#43914 = DIRECTION ( 'NONE',  ( 1.000000000000000000, 0.000000000000000000, -0.000000000000000000 ) ) ;
#43915 = CARTESIAN_POINT ( 'NONE',  ( 112.3991748109119868, -1.833838273342658809, -17.42832698103878286 ) ) ;
#43916 = CARTESIAN_POINT ( 'NONE',  ( 112.4967077545247633, -7.250697342233347165, -7.631215200338321125 ) ) ;
#43917 = CARTESIAN_POINT ( 'NONE',  ( -12.68878346039663363, -4.256507409708595091, -19.36568748919502880 ) ) ;
#43918 = CARTESIAN_POINT ( 'NONE',  ( 112.5661608795247872, -8.938348069036489818, -9.318865927141430916 ) ) ;
#43919 = CARTESIAN_POINT ( 'NONE',  ( 120.2274548109119934, 0.5811942927096110934, -14.16772938898807510 ) ) ;
#43920 = CARTESIAN_POINT ( 'NONE',  ( 122.6667014775786413, -7.893985811506177619, -18.51759400769804742 ) ) ;
#43921 = CARTESIAN_POINT ( 'NONE',  ( 105.6903015045248253, -2.477300249445798297, -7.631215200338321125 ) ) ;
#43922 = CARTESIAN_POINT ( 'NONE',  ( 117.3911214775786505, -1.561330072975668504, -17.79121239304076951 ) ) ;
#43923 = CARTESIAN_POINT ( 'NONE',  ( 112.1155414775786454, 0.9020085738987339008, -11.91225656197089222 ) ) ;
#43924 = ORIENTED_EDGE ( 'NONE', *, *, #30102, .T. ) ;
#43925 = CARTESIAN_POINT ( 'NONE',  ( 85.56953267055843071, -21.30583187727814121, -6.893215200338315363 ) ) ;
#43926 = AXIS2_PLACEMENT_3D ( 'NONE', #30747, #6579, #10232 ) ;
#43927 = CARTESIAN_POINT ( 'NONE',  ( 111.3780948109119890, -5.574606645277164318, -18.38911715685844683 ) ) ;
#43928 = AXIS2_PLACEMENT_3D ( 'NONE', #9693, #13347, #35574 ) ;
#43929 = CARTESIAN_POINT ( 'NONE',  ( 121.7023481442452777, -9.261995988541697145, -16.69588392320189030 ) ) ;
#43930 = CARTESIAN_POINT ( 'NONE',  ( 111.7751814775786556, -7.893985811506177619, -18.51759400769804742 ) ) ;
#43931 = CONTEXT_DEPENDENT_SHAPE_REPRESENTATION ( #34921, #15049 ) ;
#43932 = CARTESIAN_POINT ( 'NONE',  ( 114.2711548109119803, -0.1624402480850797581, -16.17319339645315424 ) ) ;
#43933 = ORIENTED_EDGE ( 'NONE', *, *, #7456, .F. ) ;
#43934 = CARTESIAN_POINT ( 'NONE',  ( 117.9583881442453048, 0.1319031606808879209, -14.10382304977623669 ) ) ;
#43935 = CARTESIAN_POINT ( 'NONE',  ( 124.1415948109119540, -6.344957434206665248, -7.627207830600338134 ) ) ;
#43936 = CARTESIAN_POINT ( 'NONE',  ( 109.0935046295247872, -4.863998795839590272, -7.631215200338315796 ) ) ;
#43937 = VECTOR ( 'NONE', #12307, 1000.000000000000227 ) ;
#43938 = CARTESIAN_POINT ( 'NONE',  ( 121.3052614775786111, -7.643976991954077427, -18.09477374809248928 ) ) ;
#43939 = PLANE ( 'NONE',  #15803 ) ;
#43940 = FACE_OUTER_BOUND ( 'NONE', #35593, .T. ) ;
#43941 = EDGE_LOOP ( 'NONE', ( #18879, #29509, #30636, #19191, #31101, #17704 ) ) ;
#43942 = CARTESIAN_POINT ( 'NONE',  ( 121.2019704359119743, -10.25716656981731489, -12.88942061488890545 ) ) ;
#43943 = CARTESIAN_POINT ( 'NONE',  ( 124.3685014775786328, -10.63000616557722466, -14.87417383870573495 ) ) ;
#43944 = LINE ( 'NONE', #12709, #31300 ) ;
#43945 = CARTESIAN_POINT ( 'NONE',  ( 122.1048610609119720, -3.163656168406932423, -18.89861972220013797 ) ) ;
#43946 = CARTESIAN_POINT ( 'NONE',  ( 95.62170725701130891, -25.45311294428598003, -12.61215234878372726 ) ) ;
#43947 = CARTESIAN_POINT ( 'NONE',  ( 105.0652233795248378, -1.325403438956436419, -9.854619843455211026 ) ) ;
#43948 = EDGE_CURVE ( 'NONE', #22604, #27606, #42044, .T. ) ;
#43949 = CARTESIAN_POINT ( 'NONE',  ( 109.3272331777918822, -0.01829820670803256055, -14.64321520033831447 ) ) ;
#43950 = AXIS2_PLACEMENT_3D ( 'NONE', #5153, #29557, #39821 ) ;
#43951 = CARTESIAN_POINT ( 'NONE',  ( 125.0492214775786266, -3.505236298600246325, -18.68346056562440793 ) ) ;
#43952 = CIRCLE ( 'NONE', #3900, 11.00000000000000000 ) ;
#43953 = CARTESIAN_POINT ( 'NONE',  ( 124.8099926109736657, -11.79476081310281010, -16.82845685095609412 ) ) ;
#43954 = CARTESIAN_POINT ( 'NONE',  ( 123.7749110609119754, -3.388519251034822766, -18.17055338314092694 ) ) ;
#43955 = CARTESIAN_POINT ( 'NONE',  ( 117.9016614775786280, -0.1624402480850797581, -16.17319339645315424 ) ) ;
#43956 = CARTESIAN_POINT ( 'NONE',  ( 119.7434548109119703, -0.02790360340439231729, -15.74607173546667482 ) ) ;
#43957 = ORIENTED_EDGE ( 'NONE', *, *, #9156, .T. ) ;
#43958 = CARTESIAN_POINT ( 'NONE',  ( 123.2339681442453241, -6.344957434206665248, -7.627207830600338134 ) ) ;
#43959 = CARTESIAN_POINT ( 'NONE',  ( 115.2922348109119781, -10.63000616557722466, -14.87417383870573495 ) ) ;
#43960 = CARTESIAN_POINT ( 'NONE',  ( 113.3995983795247895, -8.402594152722688392, -16.93181055722141792 ) ) ;
#43961 = DIRECTION ( 'NONE',  ( -0.9908103287288504424, 0.1352586133457950868, 0.000000000000000000 ) ) ;
#43962 = CARTESIAN_POINT ( 'NONE',  ( 123.4041481442452834, 0.1319031606808879209, -14.10382304977623669 ) ) ;
#43963 = CARTESIAN_POINT ( 'NONE',  ( 124.5954081442453116, -3.383040157471821630, -19.15922257007629170 ) ) ;
#43964 = CARTESIAN_POINT ( 'NONE',  ( 112.9134265045247645, -7.250697342233347165, -19.15521520033831138 ) ) ;
#43965 = CARTESIAN_POINT ( 'NONE',  ( 110.1353015045248469, -6.936859964151250502, -18.39754474579286025 ) ) ;
#43966 = CARTESIAN_POINT ( 'NONE',  ( 82.61796790274630098, -31.77134309784167243, -23.02235920239622047 ) ) ;
#43967 = CIRCLE ( 'NONE', #989, 2.999999999999999556 ) ;
#43968 = CARTESIAN_POINT ( 'NONE',  ( 117.1642148109119859, -0.8288870151387760510, -10.36305467784173118 ) ) ;
#43969 = CARTESIAN_POINT ( 'NONE',  ( 114.9518748109119883, -7.643976991954077427, -18.09477374809248928 ) ) ;
#43970 = CARTESIAN_POINT ( 'NONE',  ( 61.69189222814998175, -58.16308431783641453, -34.89321520033831092 ) ) ;
#43971 = CARTESIAN_POINT ( 'NONE',  ( 112.1494421295248003, -9.868328341294093420, -13.39321520033831447 ) ) ;
#43972 = ORIENTED_EDGE ( 'NONE', *, *, #32280, .F. ) ;
#43973 = FACE_OUTER_BOUND ( 'NONE', #6904, .T. ) ;
#43974 = CARTESIAN_POINT ( 'NONE',  ( 126.3539348109119800, -4.153390946401325223, -8.397313243818185668 ) ) ;
#43975 = CARTESIAN_POINT ( 'NONE',  ( 122.1743141859119817, -0.8832429491016019485, -18.19431474523657855 ) ) ;
#43976 = CARTESIAN_POINT ( 'NONE',  ( 119.7434548109119703, -7.554583864224885481, -18.48844787311982785 ) ) ;
#43977 = ORIENTED_EDGE ( 'NONE', *, *, #36192, .T. ) ;
#43978 = DIRECTION ( 'NONE',  ( -0.3135808629537518155, -0.9495615000563051300, -0.000000000000000000 ) ) ;
#43979 = CARTESIAN_POINT ( 'NONE',  ( 116.9118497693529690, -11.61451501706865308, -21.52314428506147337 ) ) ;
#43980 = ADVANCED_FACE ( 'NONE', ( #13157 ), #25275, .F. ) ;
#43981 = ORIENTED_EDGE ( 'NONE', *, *, #45138, .F. ) ;
#43982 = CARTESIAN_POINT ( 'NONE',  ( 120.2274548109119934, 0.5811942927096110934, -14.16772938898807510 ) ) ;
#43983 = CARTESIAN_POINT ( 'NONE',  ( 125.7866681442452688, -8.899110576539710493, -16.42337572283490132 ) ) ;
#43984 = CARTESIAN_POINT ( 'NONE',  ( 114.7249681442453237, -9.565557343593413364, -10.61323700422348004 ) ) ;
#43985 = DIRECTION ( 'NONE',  ( 0.000000000000000000, 0.9284778069183720062, 0.3713878862591650232 ) ) ;
#43986 = CARTESIAN_POINT ( 'NONE',  ( 124.3117748109119844, -10.30919188438810075, -12.61870101168855918 ) ) ;
#43987 = EDGE_CURVE ( 'NONE', #18085, #1795, #6304, .T. ) ;
#43988 = CARTESIAN_POINT ( 'NONE',  ( 115.0653281442453277, -6.344957434206662583, -7.627207830600332805 ) ) ;
#43989 = B_SPLINE_CURVE_WITH_KNOTS ( 'NONE', 3,
 ( #24915, #42477, #10791, #21270, #31750, #7579, #37927, #28122, #20615, #14428, #38577, #6921, #35152, #20828, #17850, #73, #21493, #28338, #42251, #38360, #11014, #4157, #34490, #25811, #29234, #39271, #1627, #8033, #18525, #35831 ),
 .UNSPECIFIED., .F., .F.,
 ( 4, 2, 2, 1, 2, 2, 2, 1, 1, 2, 2, 2, 1, 1, 1, 2, 2, 4 ),
 ( 0.000000000000000000, 0.03125000000001906114, 0.06250000000003812228, 0.09375000000005717649, 0.1093750000000654754, 0.1250000000000737743, 0.1875000000000648370, 0.2187500000000515976, 0.2343750000000364708, 0.2421875000000286438, 0.2500000000000208167, 0.3749999999999322209, 0.4374999999998873679, 0.4687499999998644973, 0.4843749999998639977, 0.4921874999998633871, 0.4999999999998627764, 1.000000000000000000 ),
 .UNSPECIFIED. ) ;
#43990 = AXIS2_PLACEMENT_3D ( 'NONE', #26728, #33313, #16013 ) ;
#43991 = EDGE_CURVE ( 'NONE', #38344, #9298, #40578, .T. ) ;
#43992 = CARTESIAN_POINT ( 'NONE',  ( 111.3854577545248645, -2.791137627527939813, -18.39754474579286025 ) ) ;
#43993 = CARTESIAN_POINT ( 'NONE',  ( 123.6310548109119765, -5.638512984488999180, -18.83840828888717311 ) ) ;
#43994 = ORIENTED_EDGE ( 'NONE', *, *, #20658, .F. ) ;
#43995 = CARTESIAN_POINT ( 'NONE',  ( 113.4202548109119846, -10.30919188438810075, -12.61870101168855918 ) ) ;
#43996 = CARTESIAN_POINT ( 'NONE',  ( 114.1577014775786552, -3.505236298600246325, -18.68346056562440793 ) ) ;
#43997 = EDGE_CURVE ( 'NONE', #18302, #36520, #8519, .T. ) ;
#43998 = DIRECTION ( 'NONE',  ( 0.05270788615228318846, -0.9986099732815399976, 2.696077241641140828E-16 ) ) ;
#43999 = CARTESIAN_POINT ( 'NONE',  ( 112.6260814775786514, -9.261995988541697145, -16.69588392320189030 ) ) ;
#44000 = VERTEX_POINT ( 'NONE', #21098 ) ;
#44001 = CARTESIAN_POINT ( 'NONE',  ( 122.8368814775786291, -1.561330072975668948, -17.79121239304076951 ) ) ;
#44002 = CARTESIAN_POINT ( 'NONE',  ( 119.7434548109119703, -2.316996251443989241, -21.63995271010855248 ) ) ;
#44003 = CARTESIAN_POINT ( 'NONE',  ( 120.1569985609119726, -9.641336978641936284, -14.86869474514246647 ) ) ;
#44004 = ADVANCED_FACE ( 'NONE', ( #32027 ), #38869, .T. ) ;
#44005 = DIRECTION ( 'NONE',  ( 0.7871354856660198740, 0.4483307682966886643, 0.4235767337848242442 ) ) ;
#44006 = EDGE_CURVE ( 'NONE', #19823, #4387, #35671, .T. ) ;
#44007 = EDGE_CURVE ( 'NONE', #32876, #4821, #21622, .T. ) ;
#44008 = CARTESIAN_POINT ( 'NONE',  ( 135.3184548109119874, -2.475900776146298110, -7.888945235271312306 ) ) ;
#44009 = CARTESIAN_POINT ( 'NONE',  ( 112.5693548109119888, 0.4262465694468514643, -12.03445270309931736 ) ) ;
#44010 = DIRECTION ( 'NONE',  ( 1.000000000000000000, 0.000000000000000000, 0.000000000000000000 ) ) ;
#44011 = CARTESIAN_POINT ( 'NONE',  ( 121.2623705389825233, -6.126425863531494542, -18.50366489541501380 ) ) ;
#44012 = CARTESIAN_POINT ( 'NONE',  ( 115.2355081442453155, 0.1319031606808879209, -14.10382304977623669 ) ) ;
#44013 = CARTESIAN_POINT ( 'NONE',  ( 114.9518748109119883, -1.834011780172310813, -8.268836392978581529 ) ) ;
#44014 = CARTESIAN_POINT ( 'NONE',  ( 122.0354079359119908, -4.360204210389833968, -8.000047426360245240 ) ) ;
#44015 = CARTESIAN_POINT ( 'NONE',  ( 125.8433948109119456, -7.643976991954077427, -18.09477374809248928 ) ) ;
#44016 = CARTESIAN_POINT ( 'NONE',  ( 114.1577014775786552, -3.505236298600246325, -18.68346056562440793 ) ) ;
#44017 = CARTESIAN_POINT ( 'NONE',  ( 122.4965214775786251, -10.30919188438810075, -12.61870101168855918 ) ) ;
#44018 = CIRCLE ( 'NONE', #22166, 3.000000000000003997 ) ;
#44019 = CARTESIAN_POINT ( 'NONE',  ( 121.7590748109119687, -7.893985811506177619, -18.51759400769804742 ) ) ;
#44020 = VERTEX_POINT ( 'NONE', #1022 ) ;
#44021 = CARTESIAN_POINT ( 'NONE',  ( 111.8319081442453182, -5.638512984488999180, -18.83840828888717311 ) ) ;
#44022 = CARTESIAN_POINT ( 'NONE',  ( 112.6356140045247827, -10.62599879583958717, -11.00651665394454604 ) ) ;
#44023 = CARTESIAN_POINT ( 'NONE',  ( 111.9410827545248708, -6.936859964151250502, -8.388885654883777576 ) ) ;
#44024 = CARTESIAN_POINT ( 'NONE',  ( 108.6073327545248048, -6.936859964151250502, -8.388885654883777576 ) ) ;
#44025 = CARTESIAN_POINT ( 'NONE',  ( 128.2184548109119930, -3.719473736431747390, -16.16631137400202078 ) ) ;
#44026 = CARTESIAN_POINT ( 'NONE',  ( 117.3911214775786505, -1.561330072975668504, -17.79121239304076951 ) ) ;
#44027 = ORIENTED_EDGE ( 'NONE', *, *, #30927, .F. ) ;
#44028 = DIRECTION ( 'NONE',  ( -1.000000000000000000, 0.000000000000000000, -0.000000000000000000 ) ) ;
#44029 = CARTESIAN_POINT ( 'NONE',  ( 109.2294434778830663, -7.784931826024912738, -8.490152284657904502 ) ) ;
#44030 = DIRECTION ( 'NONE',  ( 1.000000000000000000, 0.000000000000000000, -0.000000000000000000 ) ) ;
#44031 = CARTESIAN_POINT ( 'NONE',  ( 114.6115148109119986, -6.222761293078241884, -8.102969835052219238 ) ) ;
#44032 = CARTESIAN_POINT ( 'NONE',  ( 105.2735827545248810, -6.936859964151250502, -8.388885654883777576 ) ) ;
#44033 = CARTESIAN_POINT ( 'NONE',  ( 119.3765548109119834, 0.9020085738987339008, -11.91225656197089222 ) ) ;
#44034 = CARTESIAN_POINT ( 'NONE',  ( 115.8304577545247582, -2.791137627527939813, -18.39754474579286025 ) ) ;
#44035 = DIRECTION ( 'NONE',  ( 0.9609149988134837450, -0.1028163501681639419, 0.2570431154366518145 ) ) ;
#44036 = ORIENTED_EDGE ( 'NONE', *, *, #31181, .T. ) ;
#44037 = FACE_OUTER_BOUND ( 'NONE', #2279, .T. ) ;
#44038 = CARTESIAN_POINT ( 'NONE',  ( 123.4041481442452834, 0.1319031606808879209, -14.10382304977623669 ) ) ;
#44039 = CARTESIAN_POINT ( 'NONE',  ( 120.9081748109119872, -5.638512984488999180, -18.83840828888717311 ) ) ;
#44040 = CARTESIAN_POINT ( 'NONE',  ( 112.9097148109120070, -9.565557343593413364, -10.61323700422348004 ) ) ;
#44041 = CARTESIAN_POINT ( 'NONE',  ( 115.8027748109119841, -0.4660016031367893996, -10.09054647747474043 ) ) ;
#44042 = DIRECTION ( 'NONE',  ( -0.9498278979187094739, -0.3127730236694427068, -0.000000000000000000 ) ) ;
#44043 = CARTESIAN_POINT ( 'NONE',  ( 127.1653849502244782, -1.265433638251248327, -9.268909183209913749 ) ) ;
#44044 = CARTESIAN_POINT ( 'NONE',  ( 118.9794681442453026, -0.8288870151387760510, -10.36305467784173118 ) ) ;
#44045 = ORIENTED_EDGE ( 'NONE', *, *, #10407, .T. ) ;
#44046 = EDGE_CURVE ( 'NONE', #20392, #40242, #12162, .T. ) ;
#44047 = COLOUR_RGB ( '',0.7921568627450980005, 0.8196078431372548767, 0.9333333333333333481 ) ;
#44048 = CARTESIAN_POINT ( 'NONE',  ( 119.3198281442452924, 0.5811942927096084288, -14.16772938898808931 ) ) ;
#44049 = CARTESIAN_POINT ( 'NONE',  ( 114.6115148109119986, -3.383040157471821630, -19.15922257007629170 ) ) ;
#44050 = CARTESIAN_POINT ( 'NONE',  ( 119.5467348109119712, -5.574606645277164318, -18.38911715685844683 ) ) ;
#44051 = ORIENTED_EDGE ( 'NONE', *, *, #8673, .F. ) ;
#44052 = CARTESIAN_POINT ( 'NONE',  ( 124.1190016859119680, -0.6942167230862511529, -9.935906262978006609 ) ) ;
#44053 = CARTESIAN_POINT ( 'NONE',  ( 117.9016614775786280, -9.988377603198976828, -10.36322818467138340 ) ) ;
#44054 = AXIS2_PLACEMENT_3D ( 'NONE', #22012, #11535, #38878 ) ;
#44055 = CARTESIAN_POINT ( 'NONE',  ( 113.7468640045248236, -10.62599879583958717, -11.00651665394454604 ) ) ;
#44056 = CARTESIAN_POINT ( 'NONE',  ( 114.7816948109119863, -9.859900752359374465, -12.68260735090039404 ) ) ;
#44057 = ORIENTED_EDGE ( 'NONE', *, *, #36154, .T. ) ;
#44058 = ORIENTED_EDGE ( 'NONE', *, *, #23804, .T. ) ;
#44059 = CARTESIAN_POINT ( 'NONE',  ( 125.3895814775786448, -2.084020599724406786, -8.691656652584148546 ) ) ;
#44060 = CARTESIAN_POINT ( 'NONE',  ( 122.0427081442452817, -9.859900752359378018, -12.68260735090039759 ) ) ;
#44061 = CARTESIAN_POINT ( 'NONE',  ( 66.16802772684418699, -15.11730172789017423, -16.39321520033831447 ) ) ;
#44062 = EDGE_CURVE ( 'NONE', #2526, #21997, #33527, .T. ) ;
#44063 = CARTESIAN_POINT ( 'NONE',  ( 121.9470836909669913, -25.99489077589524300, -13.39321520033831447 ) ) ;
#44064 = CARTESIAN_POINT ( 'NONE',  ( 119.1496481442453046, -3.383040157471821630, -19.15922257007629170 ) ) ;
#44065 = CARTESIAN_POINT ( 'NONE',  ( 108.1211608795247798, -8.938348069036489818, -9.318865927141430916 ) ) ;
#44066 = EDGE_CURVE ( 'NONE', #17949, #32403, #22223, .T. ) ;
#44067 = CARTESIAN_POINT ( 'NONE',  ( 119.3765548109119834, 0.9020085738987339008, -11.91225656197089222 ) ) ;
#44069 = CARTESIAN_POINT ( 'NONE',  ( 117.1074881442453233, 0.4262465694468514643, -12.03445270309931736 ) ) ;
#44068 = CARTESIAN_POINT ( 'NONE',  ( 116.4834948109119779, -1.561330072975668504, -17.79121239304076951 ) ) ;
#44070 = EDGE_CURVE ( 'NONE', #13382, #11921, #43429, .T. ) ;
#44071 = PRODUCT_RELATED_PRODUCT_CATEGORY ( 'part', '', ( #21957 ) ) ;
#44072 = CARTESIAN_POINT ( 'NONE',  ( 70.19189222814998175, -52.97765562947117957, -34.39388673445118627 ) ) ;
#44073 = CARTESIAN_POINT ( 'NONE',  ( 112.2630620330015461, -1.172797794773250413, -17.05961127468924943 ) ) ;
#44074 = VERTEX_POINT ( 'NONE', #12195 ) ;
#44075 = CARTESIAN_POINT ( 'NONE',  ( 123.5176014775786228, -0.8288870151387760510, -10.36305467784173118 ) ) ;
#44076 = LINE ( 'NONE', #13060, #36558 ) ;
#44077 = CARTESIAN_POINT ( 'NONE',  ( 82.31000308962319423, -13.76004065658516673, -18.64321520033831803 ) ) ;
#44078 = VECTOR ( 'NONE', #17367, 1000.000000000000000 ) ;
#44079 = CARTESIAN_POINT ( 'NONE',  ( 111.8716296295247901, -4.863998795839590272, -19.15521520033831493 ) ) ;
#44080 = CARTESIAN_POINT ( 'NONE',  ( 113.0523327545247838, -6.936859964151250502, -8.388885654883777576 ) ) ;
#44081 = CARTESIAN_POINT ( 'NONE',  ( 112.2883483795247770, -0.7896495226426338832, -9.318865927141430916 ) ) ;
#44082 = CARTESIAN_POINT ( 'NONE',  ( 123.6310548109119765, -5.638512984488999180, -18.83840828888717311 ) ) ;
#44083 = EDGE_LOOP ( 'NONE', ( #23844, #36487, #23263, #23344 ) ) ;
#44084 = CARTESIAN_POINT ( 'NONE',  ( 119.5467348109119712, -4.089484607189486809, -7.948022111789456723 ) ) ;
#44085 = DIRECTION ( 'NONE',  ( 0.000000000000000000, 0.6004852223388322807, -0.7996358532186280677 ) ) ;
#44086 = CYLINDRICAL_SURFACE ( 'NONE', #35040, 3.000000000000001776 ) ;
#44087 = CARTESIAN_POINT ( 'NONE',  ( 120.2274548109119934, 0.5811942927096110934, -14.16772938898807510 ) ) ;
#44088 = CARTESIAN_POINT ( 'NONE',  ( 122.4397948109119767, -9.988377603198976828, -10.36322818467138340 ) ) ;
#44090 = AXIS2_PLACEMENT_3D ( 'NONE', #7132, #6703, #3927 ) ;
#44089 = CARTESIAN_POINT ( 'NONE',  ( 62.57128181610967488, -3.480577623552236766, -19.20948089883370713 ) ) ;
#44091 = CARTESIAN_POINT ( 'NONE',  ( 125.6732148109119862, -9.859900752359378018, -12.68260735090039759 ) ) ;
#44092 = CARTESIAN_POINT ( 'NONE',  ( 93.44708369096697709, -28.02818487991510921, -14.23328370144882093 ) ) ;
#44093 = CARTESIAN_POINT ( 'NONE',  ( 31.33087284928346605, -19.31933043625826230, -8.593215200338315540 ) ) ;
#44094 = ORIENTED_EDGE ( 'NONE', *, *, #30928, .T. ) ;
#44095 = CARTESIAN_POINT ( 'NONE',  ( -1.667125314829374982, -6.784308280680000358, -8.532095462264171815 ) ) ;
#44096 = CARTESIAN_POINT ( 'NONE',  ( 114.1934435773848833, -2.467220198592768199, -17.83387418641523325 ) ) ;
#44097 = CARTESIAN_POINT ( 'NONE',  ( 124.6521348109119884, -7.894159318335828068, -9.358103419637847864 ) ) ;
#44098 = CARTESIAN_POINT ( 'NONE',  ( 108.6073327545248048, -6.936859964151250502, -8.388885654883777576 ) ) ;
#44099 = CARTESIAN_POINT ( 'NONE',  ( 112.7050671295247923, 0.1403307496149613920, -13.39321520033831447 ) ) ;
#44100 = CARTESIAN_POINT ( 'NONE',  ( 117.1642148109119859, -0.8288870151387760510, -10.36305467784173118 ) ) ;
#44101 = CARTESIAN_POINT ( 'NONE',  ( 61.69189222814998175, -58.16308431783641453, -34.89321520033831092 ) ) ;
#44102 = CARTESIAN_POINT ( 'NONE',  ( 68.68839935636917460, -25.95913848132418522, -5.893215200338315363 ) ) ;
#44103 = CARTESIAN_POINT ( 'NONE',  ( 113.4769814775786330, 0.4262465694468514643, -12.03445270309931736 ) ) ;
#44104 = CARTESIAN_POINT ( 'NONE',  ( 122.9503348109119827, 0.5811942927096110934, -14.16772938898807510 ) ) ;
#44105 = ORIENTED_EDGE ( 'NONE', *, *, #9520, .T. ) ;
#44106 = CARTESIAN_POINT ( 'NONE',  ( 123.5176014775786228, -0.8288870151387760510, -10.36305467784173118 ) ) ;
#44107 = CARTESIAN_POINT ( 'NONE',  ( 113.9307948109119906, 0.9020085738987339008, -11.91225656197089222 ) ) ;
#44108 = CARTESIAN_POINT ( 'NONE',  ( 123.3474214775786209, -9.988377603198976828, -10.36322818467138340 ) ) ;
#44109 = CARTESIAN_POINT ( 'NONE',  ( 124.6521348109119884, -7.894159318335828068, -9.358103419637847864 ) ) ;
#44110 = VERTEX_POINT ( 'NONE', #15161 ) ;
#44111 = LINE ( 'NONE', #16059, #23063 ) ;
#44112 = ADVANCED_FACE ( 'NONE', ( #16062 ), #18034, .T. ) ;
#44113 = CARTESIAN_POINT ( 'NONE',  ( 123.0070614775786169, 0.9020085738987339008, -11.91225656197089222 ) ) ;
#44114 = CARTESIAN_POINT ( 'NONE',  ( 114.3846081442453197, 0.4262465694468514643, -12.03445270309931736 ) ) ;
#44115 = CARTESIAN_POINT ( 'NONE',  ( 124.9924948109119924, -4.089484607189486809, -7.948022111789456723 ) ) ;
#44116 = CARTESIAN_POINT ( 'NONE',  ( 106.9404577545248145, -7.250697342233347165, -7.631215200338321125 ) ) ;
#44117 = CIRCLE ( 'NONE', #39738, 0.8509999999999994236 ) ;
#44118 = LINE ( 'NONE', #32697, #24979 ) ;
#44119 = ORIENTED_EDGE ( 'NONE', *, *, #4967, .F. ) ;
#44120 = CARTESIAN_POINT ( 'NONE',  ( 137.8430364429465840, -1.575724663492070965, -16.52305390663654450 ) ) ;
#44121 = CARTESIAN_POINT ( 'NONE',  ( 108.5378796295247810, -4.863998795839590272, -8.388885654883775800 ) ) ;
#44122 = EDGE_CURVE ( 'NONE', #23072, #11415, #28018, .T. ) ;
#44123 = B_SPLINE_CURVE_WITH_KNOTS ( 'NONE', 3,
 ( #257, #21011, #25780, #36476, #4343, #39687 ),
 .UNSPECIFIED., .F., .F.,
 ( 4, 2, 4 ),
 ( -8.394000326495523731E-06, 0.0005522989975109767087, 0.001112991995348449085 ),
 .UNSPECIFIED. ) ;
#44124 = DIRECTION ( 'NONE',  ( -0.9908103287288505534, 0.1352586133457944206, 0.000000000000000000 ) ) ;
#44125 = CARTESIAN_POINT ( 'NONE',  ( 120.9081748109119872, -4.153390946401325223, -8.397313243818185668 ) ) ;
#44126 = CARTESIAN_POINT ( 'NONE',  ( 112.3424481442453384, -3.505236298600246325, -18.68346056562440793 ) ) ;
#44127 = CARTESIAN_POINT ( 'NONE',  ( 126.8024586715757778, -6.490782095255248407, -18.42897405940419020 ) ) ;
#44128 = ORIENTED_EDGE ( 'NONE', *, *, #37835, .F. ) ;
#44129 = CARTESIAN_POINT ( 'NONE',  ( 115.7914926669217834, -2.334846009198389805, -18.01015021110788439 ) ) ;
#44130 = CARTESIAN_POINT ( 'NONE',  ( 117.3911214775786505, -7.894159318335828068, -9.358103419637847864 ) ) ;
#44131 = CARTESIAN_POINT ( 'NONE',  ( 116.3148066399283778, 0.4261359969231631739, -14.64321520033831447 ) ) ;
#44132 = LINE ( 'NONE', #15629, #29361 ) ;
#44133 = CARTESIAN_POINT ( 'NONE',  ( 112.1155414775786454, -10.15424416112533912, -14.75197769757731336 ) ) ;
#44135 = CARTESIAN_POINT ( 'NONE',  ( 121.3052614775786111, -1.834011780172310813, -8.268836392978581529 ) ) ;
#44134 = CARTESIAN_POINT ( 'NONE',  ( 114.4099712410415748, 0.7607806665037644134, -12.14321520033829316 ) ) ;
#44136 = AXIS2_PLACEMENT_3D ( 'NONE', #26808, #9708, #2622 ) ;
#44137 = CARTESIAN_POINT ( 'NONE',  ( 126.2972081442452890, -2.084020599724406786, -8.691656652584148546 ) ) ;
#44138 = ORIENTED_EDGE ( 'NONE', *, *, #25920, .F. ) ;
#44139 = CARTESIAN_POINT ( 'NONE',  ( 114.3339130180080758, 0.7607806665038616689, -14.64321520033833579 ) ) ;
#44140 = CARTESIAN_POINT ( 'NONE',  ( 89.67401078471493747, -25.99489077589524300, -13.39321520033831447 ) ) ;
#44141 = CARTESIAN_POINT ( 'NONE',  ( 114.7192077545248594, -7.250697342233347165, -7.631215200338321125 ) ) ;
#44142 = CARTESIAN_POINT ( 'NONE',  ( 125.7866681442452688, -8.899110576539710493, -16.42337572283490132 ) ) ;
#44143 = CARTESIAN_POINT ( 'NONE',  ( 120.4543614775786295, -5.574606645277164318, -18.38911715685844683 ) ) ;
#44144 = CARTESIAN_POINT ( 'NONE',  ( 87.14323352029596492, -25.23119213852205789, -15.24166438581092109 ) ) ;
#44145 = CARTESIAN_POINT ( 'NONE',  ( 112.5661608795247872, -1.325403438956436419, -16.93181055722141792 ) ) ;
#44146 = AXIS2_PLACEMENT_3D ( 'NONE', #15281, #4788, #1144 ) ;
#44147 = CARTESIAN_POINT ( 'NONE',  ( 90.06246830635160450, -26.60966817898065884, -11.90521360603286816 ) ) ;
#44148 = CARTESIAN_POINT ( 'NONE',  ( 120.2542535264548889, -8.247323210606168686, -17.08054893949881148 ) ) ;
#44149 = CARTESIAN_POINT ( 'NONE',  ( 113.2500748109119968, -3.505236298600246325, -18.68346056562440793 ) ) ;
#44150 = CARTESIAN_POINT ( 'NONE',  ( 112.4272546295247821, -4.863998795839590272, -7.631215200338315796 ) ) ;
#44151 = LINE ( 'NONE', #6046, #13891 ) ;
#44152 = CARTESIAN_POINT ( 'NONE',  ( 112.6356140045247827, -10.62599879583958717, -11.00651665394454604 ) ) ;
#44153 = CARTESIAN_POINT ( 'NONE',  ( 125.3328548109119964, -9.261995988541697145, -16.69588392320189030 ) ) ;
#44154 = CARTESIAN_POINT ( 'NONE',  ( 120.9649014775786355, -3.383040157471821630, -19.15922257007629170 ) ) ;
#44155 = CARTESIAN_POINT ( 'NONE',  ( 114.6497546295247929, -4.863998795839590272, -7.631215200338315796 ) ) ;
#44156 = CARTESIAN_POINT ( 'NONE',  ( 116.7104014775786425, -0.4660016031367893996, -10.09054647747474043 ) ) ;
#44157 = CARTESIAN_POINT ( 'NONE',  ( 112.3991748109119868, -8.166667518702817929, -8.995218007635859436 ) ) ;
#44158 = VERTEX_POINT ( 'NONE', #30984 ) ;
#44159 = CARTESIAN_POINT ( 'NONE',  ( 112.7395348109119766, -4.153390946401321671, -8.397313243818183892 ) ) ;
#44160 = CIRCLE ( 'NONE', #11405, 2.999999999999999556 ) ;
#44161 = CARTESIAN_POINT ( 'NONE',  ( 124.9357681442453014, -1.834011780172310813, -8.268836392978581529 ) ) ;
#44162 = CARTESIAN_POINT ( 'NONE',  ( 118.4689281442453392, 0.9020085738987339008, -11.91225656197089222 ) ) ;
#44163 = CARTESIAN_POINT ( 'NONE',  ( 112.7962614775786676, -3.383040157471821630, -19.15922257007629170 ) ) ;
#44164 = CARTESIAN_POINT ( 'NONE',  ( 125.8433948109119456, -1.834011780172310813, -8.268836392978581529 ) ) ;
#44165 = EDGE_LOOP ( 'NONE', ( #15898, #41534, #35939, #12053, #9162 ) ) ;
#44166 = CARTESIAN_POINT ( 'NONE',  ( 119.3765548109119834, -10.15424416112533912, -14.75197769757731336 ) ) ;
#44167 =( BOUNDED_CURVE ( )  B_SPLINE_CURVE ( 2, ( #8145, #8592, #40043, #22490, #18630, #4708, #43694, #36832, #36384 ),
 .UNSPECIFIED., .F., .F. ) 
 B_SPLINE_CURVE_WITH_KNOTS ( ( 3, 2, 2, 2, 3 ),
 ( 0.5030750193655179059, 0.6250000000000000000, 0.7500000000000000000, 0.8750000000000000000, 0.9595335776365219171 ),
 .UNSPECIFIED. ) 
 CURVE ( )  GEOMETRIC_REPRESENTATION_ITEM ( )  RATIONAL_B_SPLINE_CURVE ( ( 0.9963469806983950017, 0.9257521078044069762, 1.000000000000000000, 0.9238795325112869605, 1.000000000000000000, 0.9238795325112869605, 1.000000000000000000, 0.9485221164145160033, 0.9666699875272299902 ) ) 
 REPRESENTATION_ITEM ( '' )  );
#44168 = CARTESIAN_POINT ( 'NONE',  ( 125.3328548109119964, -9.261995988541697145, -16.69588392320189030 ) ) ;
#44169 = B_SPLINE_CURVE_WITH_KNOTS ( 'NONE', 3,
 ( #27185, #34880, #34669, #24213, #23772, #2778, #22904, #20348, #36797, #17154 ),
 .UNSPECIFIED., .F., .F.,
 ( 4, 3, 3, 4 ),
 ( 0.000000000000000000, 0.0001671877548681239927, 0.0003343755096277624991, 0.0006463528481650629171 ),
 .UNSPECIFIED. ) ;
#44170 = CARTESIAN_POINT ( 'NONE',  ( 107.4960827545248350, -2.477300249445798297, -19.15521520033831138 ) ) ;
#44171 = CARTESIAN_POINT ( 'NONE',  ( 122.9503348109119827, -9.859900752359378018, -12.68260735090039759 ) ) ;
#44172 = CARTESIAN_POINT ( 'NONE',  ( 128.2184548109119930, -8.536181032868617180, -18.13822074491315561 ) ) ;
#44173 = DIRECTION ( 'NONE',  ( -0.2768435750659241079, -0.3568721902840695792, 0.8921882507333129819 ) ) ;
#44174 = ORIENTED_EDGE ( 'NONE', *, *, #13884, .T. ) ;
#44175 = CARTESIAN_POINT ( 'NONE',  ( 122.1048610609119720, -6.340755971794695078, -8.611740276972781771 ) ) ;
#44176 = CARTESIAN_POINT ( 'NONE',  ( 122.4965214775786251, -10.30919188438810075, -12.61870101168855918 ) ) ;
#44177 = AXIS2_PLACEMENT_3D ( 'NONE', #24332, #38216, #27976 ) ;
#44178 = CARTESIAN_POINT ( 'NONE',  ( 119.7434548109119703, -7.411001340234434132, -5.146477690568067587 ) ) ;
#44179 = FILL_AREA_STYLE_COLOUR ( '', #14353 ) ;
#44180 = EDGE_CURVE ( 'NONE', #9192, #44761, #10470, .T. ) ;
#44181 = CARTESIAN_POINT ( 'NONE',  ( 112.7855738145250513, -3.807985514183288345, -19.09877912889401230 ) ) ;
#44182 = CARTESIAN_POINT ( 'NONE',  ( 90.71204046351577688, -10.71075648645643774, -8.143215200338314474 ) ) ;
#44183 = CARTESIAN_POINT ( 'NONE',  ( 107.1488171295248861, 0.1403307496149613920, -13.39321520033831447 ) ) ;
#44184 = CARTESIAN_POINT ( 'NONE',  ( 121.4103298109119748, -2.173413727453599176, -8.297982527556802879 ) ) ;
#44185 = AXIS2_PLACEMENT_3D ( 'NONE', #18702, #2256, #36013 ) ;
#44186 = LINE ( 'NONE', #27526, #33272 ) ;
#44187 = CARTESIAN_POINT ( 'NONE',  ( 125.1235803781499953, -2.490773129849583434, -17.80250993700375517 ) ) ;
#44188 = CARTESIAN_POINT ( 'NONE',  ( 124.6521348109119884, -1.561330072975668948, -17.79121239304076951 ) ) ;
#44189 = CARTESIAN_POINT ( 'NONE',  ( 120.1140014775786398, -7.894159318335828068, -9.358103419637847864 ) ) ;
#44190 = CARTESIAN_POINT ( 'NONE',  ( 119.7434548109119703, 0.3824594525549545043, -13.03383199448628460 ) ) ;
#44191 = ORIENTED_EDGE ( 'NONE', *, *, #32152, .T. ) ;
#44192 = CARTESIAN_POINT ( 'NONE',  ( 122.6667014775786413, -7.893985811506177619, -18.51759400769804742 ) ) ;
#44193 = CARTESIAN_POINT ( 'NONE',  ( 117.7882081442453170, -6.344957434206665248, -7.627207830600338134 ) ) ;
#44194 = CARTESIAN_POINT ( 'NONE',  ( 116.2471765045247594, -2.791137627527939813, -8.388885654883777576 ) ) ;
#44195 = CARTESIAN_POINT ( 'NONE',  ( 113.1933481442453058, -5.574606645277164318, -18.38911715685844683 ) ) ;
#44196 = CARTESIAN_POINT ( 'NONE',  ( 112.0588148109119828, 0.5811942927096154232, -14.16772938898807155 ) ) ;
#44197 = CARTESIAN_POINT ( 'NONE',  ( 125.1626748109119802, -9.988377603198980381, -10.36322818467138518 ) ) ;
#44198 = CARTESIAN_POINT ( 'NONE',  ( 110.5520202545248054, -10.62599879583958717, -15.77991374673208469 ) ) ;
#44199 = CARTESIAN_POINT ( 'NONE',  ( 109.3018640045248304, 0.1403307496149616695, -15.46607636864997204 ) ) ;
#44200 = CARTESIAN_POINT ( 'NONE',  ( 116.3166296295247832, -4.863998795839590272, -19.15521520033831493 ) ) ;
#44201 = CARTESIAN_POINT ( 'NONE',  ( 117.7314814775786260, -5.574606645277164318, -18.38911715685844683 ) ) ;
#44202 = CARTESIAN_POINT ( 'NONE',  ( 115.9729548109119861, -3.505236298600246325, -18.68346056562440793 ) ) ;
#44203 = CARTESIAN_POINT ( 'NONE',  ( 73.07463722459043254, -55.50355580373558695, -34.50973010800571927 ) ) ;
#44204 = CIRCLE ( 'NONE', #1216, 2.999999999999999556 ) ;
#44205 = CARTESIAN_POINT ( 'NONE',  ( 114.6497546295247929, -4.863998795839590272, -18.39754474579285315 ) ) ;
#44206 = ORIENTED_EDGE ( 'NONE', *, *, #36723, .T. ) ;
#44207 = CARTESIAN_POINT ( 'NONE',  ( 119.7821199480702603, -6.365377317481695663, -18.95617363400926081 ) ) ;
#44208 = CARTESIAN_POINT ( 'NONE',  ( 126.2972081442452890, -2.084020599724406786, -8.691656652584148546 ) ) ;
#44209 = CARTESIAN_POINT ( 'NONE',  ( 120.9241579359119925, -4.360204210389833968, -8.000047426360245240 ) ) ;
#44210 = CARTESIAN_POINT ( 'NONE',  ( 120.1601735609119856, -9.645473719204776586, -14.86997237629376656 ) ) ;
#44211 = ORIENTED_EDGE ( 'NONE', *, *, #30653, .T. ) ;
#44212 = LINE ( 'NONE', #16848, #42880 ) ;
#44213 = CARTESIAN_POINT ( 'NONE',  ( 111.4926360275532176, -1.279900991230100260, -16.91698735540673226 ) ) ;
#44214 = CIRCLE ( 'NONE', #1227, 2.999999999999999556 ) ;
#44215 = EDGE_LOOP ( 'NONE', ( #15152, #13243, #3711, #38359, #26172, #10021, #26646, #22740, #4156, #32191, #18644, #13936, #28733 ) ) ;
#44216 = CARTESIAN_POINT ( 'NONE',  ( 119.8870948109119752, -9.261995988541697145, -16.69588392320189030 ) ) ;
#44217 = CARTESIAN_POINT ( 'NONE',  ( 123.4041481442452834, 0.1319031606808879209, -14.10382304977623669 ) ) ;
#44218 = CARTESIAN_POINT ( 'NONE',  ( 115.8595014775786609, -7.643976991954077427, -18.09477374809248928 ) ) ;
#44219 = DIRECTION ( 'NONE',  ( 1.000000000000000000, 0.000000000000000000, 0.000000000000000000 ) ) ;
#44220 = CARTESIAN_POINT ( 'NONE',  ( 120.5678148109119832, -8.166667518702819706, -8.995218007635861213 ) ) ;
#44221 = CARTESIAN_POINT ( 'NONE',  ( 113.1366214775786432, -1.834011780172310813, -8.268836392978581529 ) ) ;
#44222 = VECTOR ( 'NONE', #39622, 1000.000000000000000 ) ;
#44223 = CARTESIAN_POINT ( 'NONE',  ( 113.4690515045247992, -6.936859964151250502, -18.39754474579286025 ) ) ;
#44224 = CARTESIAN_POINT ( 'NONE',  ( 122.8936081442453059, 0.2603800115204892296, -16.42320221600525088 ) ) ;
#44225 = CARTESIAN_POINT ( 'NONE',  ( 123.2184548109119788, -3.410847707154505137, -16.57729307524250828 ) ) ;
#44226 = ORIENTED_EDGE ( 'NONE', *, *, #13644, .F. ) ;
#44227 = CARTESIAN_POINT ( 'NONE',  ( 119.6034614775786196, -6.344957434206665248, -7.627207830600338134 ) ) ;
#44228 = CARTESIAN_POINT ( 'NONE',  ( 113.9307948109119764, -10.15424416112533912, -14.75197769757731336 ) ) ;
#44229 = DIRECTION ( 'NONE',  ( 1.000000000000000000, 0.000000000000000000, -0.000000000000000000 ) ) ;
#44230 = CARTESIAN_POINT ( 'NONE',  ( 113.4202548109119846, -10.30919188438810075, -12.61870101168855918 ) ) ;
#44231 = EDGE_LOOP ( 'NONE', ( #2872, #21161, #26085, #21255, #26759, #14169 ) ) ;
#44232 = CARTESIAN_POINT ( 'NONE',  ( 120.6812681442452941, -10.30919188438810075, -12.61870101168855918 ) ) ;
#44234 = DIRECTION ( 'NONE',  ( 0.000000000000000000, 0.000000000000000000, 1.000000000000000000 ) ) ;
#44233 = AXIS2_PLACEMENT_3D ( 'NONE', #17629, #27900, #35378 ) ;
#44235 = CARTESIAN_POINT ( 'NONE',  ( 109.4154010812577837, -0.01829820670803256055, -12.14321520033831625 ) ) ;
#44236 = DIRECTION ( 'NONE',  ( 0.9609149988134837450, -0.1028163501681639419, 0.2570431154366518145 ) ) ;
#44237 = CARTESIAN_POINT ( 'NONE',  ( 116.7104014775786425, -8.899110576539710493, -16.42337572283490132 ) ) ;
#44238 = CARTESIAN_POINT ( 'NONE',  ( 137.3527759848290088, -3.463350433249969829, -8.419698276038079854 ) ) ;
#44239 = CARTESIAN_POINT ( 'NONE',  ( 119.4332814775786318, -8.899110576539710493, -16.42337572283490132 ) ) ;
#44240 = ADVANCED_FACE ( 'NONE', ( #38702 ), #29172, .T. ) ;
#44241 = CARTESIAN_POINT ( 'NONE',  ( 117.1500671295247713, 0.1403307496149613920, -13.39321520033831447 ) ) ;
#44242 = CARTESIAN_POINT ( 'NONE',  ( 128.2184548109119930, -10.36826876090625760, -11.00511718064540467 ) ) ;
#44243 = CARTESIAN_POINT ( 'NONE',  ( 116.4267681442453153, -6.222761293078241884, -8.102969835052219238 ) ) ;
#44244 = CARTESIAN_POINT ( 'NONE',  ( 114.5547881442453217, -5.638512984488999180, -18.83840828888717311 ) ) ;
#44245 = CARTESIAN_POINT ( 'NONE',  ( 120.2990798109119766, -2.173413727453600508, -8.297982527556802879 ) ) ;
#44246 = CARTESIAN_POINT ( 'NONE',  ( 125.7299414775786346, -10.15424416112533912, -14.75197769757731336 ) ) ;
#44247 = CARTESIAN_POINT ( 'NONE',  ( 116.3700414775786527, -4.153390946401321671, -8.397313243818183892 ) ) ;
#44248 = CARTESIAN_POINT ( 'NONE',  ( 123.7445081442452874, -1.561330072975668948, -17.79121239304076951 ) ) ;
#44249 = CIRCLE ( 'NONE', #10748, 0.5000000000000004441 ) ;
#44250 = CARTESIAN_POINT ( 'NONE',  ( 123.1205148109119563, -1.834011780172310813, -8.268836392978581529 ) ) ;
#44251 = ORIENTED_EDGE ( 'NONE', *, *, #27157, .F. ) ;
#44252 = CARTESIAN_POINT ( 'NONE',  ( 114.2144281442453178, -8.166667518702817929, -8.995218007635859436 ) ) ;
#44253 = EDGE_CURVE ( 'NONE', #41752, #21031, #34102, .T. ) ;
#44254 = CARTESIAN_POINT ( 'NONE',  ( 113.6774108795247997, -8.938348069036489818, -9.318865927141430916 ) ) ;
#44255 = CARTESIAN_POINT ( 'NONE',  ( 105.2735827545248810, -6.936859964151250502, -8.388885654883777576 ) ) ;
#44256 = CARTESIAN_POINT ( 'NONE',  ( 104.9957702545248566, 0.1403307496149616695, -11.32035403202665336 ) ) ;
#44257 = CARTESIAN_POINT ( 'NONE',  ( 27.57768543387103222, -14.97172645945875935, -7.393215200338315363 ) ) ;
#44258 = CARTESIAN_POINT ( 'NONE',  ( 117.5045748109119756, 0.5811942927096110934, -14.16772938898807510 ) ) ;
#44259 = EDGE_LOOP ( 'NONE', ( #92, #23564, #44191, #18068 ) ) ;
#44260 = CARTESIAN_POINT ( 'NONE',  ( 126.1837548109119211, -10.63000616557722466, -14.87417383870573495 ) ) ;
#44261 = DIRECTION ( 'NONE',  ( 0.000000000000000000, 0.000000000000000000, 1.000000000000000000 ) ) ;
#44262 = CARTESIAN_POINT ( 'NONE',  ( 113.5337081442453240, -0.8288870151387760510, -10.36305467784173118 ) ) ;
#44263 = CARTESIAN_POINT ( 'NONE',  ( 124.8790414775786246, -8.899110576539426276, -16.42337572283528146 ) ) ;
#44264 = CARTESIAN_POINT ( 'NONE',  ( 122.7801548109119665, -3.383040157471821630, -19.15922257007629170 ) ) ;
#44265 = CARTESIAN_POINT ( 'NONE',  ( 105.6208483795248299, -0.7896495226426338832, -9.318865927141430916 ) ) ;
#44266 = DIRECTION ( 'NONE',  ( 0.000000000000000000, 0.000000000000000000, -1.000000000000000000 ) ) ;
#44267 = ORIENTED_EDGE ( 'NONE', *, *, #33948, .F. ) ;
#44268 = DIRECTION ( 'NONE',  ( -0.000000000000000000, 0.9284778069183718952, 0.3713878862591650232 ) ) ;
#44269 = CARTESIAN_POINT ( 'NONE',  ( 122.8368814775786291, -7.894159318335828068, -9.358103419637847864 ) ) ;
#44270 = CARTESIAN_POINT ( 'NONE',  ( 118.9227414775786400, -10.63000616557722466, -14.87417383870573495 ) ) ;
#44271 = CIRCLE ( 'NONE', #39887, 5.999999999999997335 ) ;
#44272 = CARTESIAN_POINT ( 'NONE',  ( 115.0086014775786509, -5.574606645277164318, -18.38911715685844683 ) ) ;
#44273 = CARTESIAN_POINT ( 'NONE',  ( 115.5758681442453053, -1.561330072975668060, -17.79121239304076951 ) ) ;
#44274 = EDGE_CURVE ( 'NONE', #9931, #21884, #2711, .T. ) ;
#44275 = DIRECTION ( 'NONE',  ( 0.3127730236694426513, -0.9498278979187093629, 0.000000000000000000 ) ) ;
#44276 = CARTESIAN_POINT ( 'NONE',  ( 125.4463081442452932, -4.153390946401325223, -8.397313243818185668 ) ) ;
#44277 = CARTESIAN_POINT ( 'NONE',  ( 120.5678148109119832, -1.833838273342659253, -17.42832698103878286 ) ) ;
#44278 = ORIENTED_EDGE ( 'NONE', *, *, #7486, .F. ) ;
#44279 = EDGE_CURVE ( 'NONE', #11415, #40595, #5282, .T. ) ;
#44280 = EDGE_CURVE ( 'NONE', #31011, #43660, #18738, .T. ) ;
#44281 = CARTESIAN_POINT ( 'NONE',  ( 122.9382985609119743, -10.36940331770106916, -15.09355782777062061 ) ) ;
#44282 = CARTESIAN_POINT ( 'NONE',  ( 113.8173414775786512, 0.2603800115204892296, -16.42320221600525088 ) ) ;
#44283 = CARTESIAN_POINT ( 'NONE',  ( 120.0005481442453146, -4.153390946401325223, -8.397313243818185668 ) ) ;
#44284 = ORIENTED_EDGE ( 'NONE', *, *, #44897, .F. ) ;
#44285 = CARTESIAN_POINT ( 'NONE',  ( 121.7575954359119805, 0.5291689781388270175, -13.89700978578772705 ) ) ;
#44286 = CARTESIAN_POINT ( 'NONE',  ( 117.4478481442453131, 0.2603800115204892296, -16.42320221600525088 ) ) ;
#44287 = CARTESIAN_POINT ( 'NONE',  ( 113.1217858795247935, -0.7896495226426338832, -17.46756447353520159 ) ) ;
#44288 = CARTESIAN_POINT ( 'NONE',  ( 115.4056881442453459, -2.084020599724406786, -8.691656652584148546 ) ) ;
#44289 = VERTEX_POINT ( 'NONE', #32538 ) ;
#44290 = ORIENTED_EDGE ( 'NONE', *, *, #13048, .F. ) ;
#44291 = CARTESIAN_POINT ( 'NONE',  ( 112.1155414775786454, 0.9020085738987339008, -11.91225656197089222 ) ) ;
#44292 = CARTESIAN_POINT ( 'NONE',  ( 120.5678148109119832, -1.833838273342659253, -17.42832698103878286 ) ) ;
#44293 = DIRECTION ( 'NONE',  ( 0.000000000000000000, 0.000000000000000000, 1.000000000000000000 ) ) ;
#44294 = CARTESIAN_POINT ( 'NONE',  ( 70.19189222814998175, -53.54563792646638376, -34.62107767336419073 ) ) ;
#44295 = CARTESIAN_POINT ( 'NONE',  ( 119.9438214775786378, -7.893985811506177619, -18.51759400769804742 ) ) ;
#44296 = EDGE_CURVE ( 'NONE', #36562, #40329, #28216, .T. ) ;
#44297 = CARTESIAN_POINT ( 'NONE',  ( 108.0517077545248696, -7.250697342233347165, -7.631215200338321125 ) ) ;
#44298 = CARTESIAN_POINT ( 'NONE',  ( 118.4122014775786340, 0.5811942927096110934, -14.16772938898807510 ) ) ;
#44300 = CARTESIAN_POINT ( 'NONE',  ( 119.9438214775786378, -2.084020599724406786, -8.691656652584148546 ) ) ;
#44299 = CARTESIAN_POINT ( 'NONE',  ( 119.9438214775786378, -7.893985811506177619, -18.51759400769804742 ) ) ;
#44301 = CARTESIAN_POINT ( 'NONE',  ( 124.5386814775786206, -4.153390946401325223, -8.397313243818185668 ) ) ;
#44302 = CARTESIAN_POINT ( 'NONE',  ( 112.8529881442453302, -1.561330072975668060, -17.79121239304076596 ) ) ;
#44303 = ORIENTED_EDGE ( 'NONE', *, *, #12554, .T. ) ;
#44304 = CARTESIAN_POINT ( 'NONE',  ( 123.0070614775786169, -10.15424416112533912, -14.75197769757731336 ) ) ;
#44305 = FACE_OUTER_BOUND ( 'NONE', #24204, .T. ) ;
#44306 = EDGE_CURVE ( 'NONE', #17767, #27212, #15220, .T. ) ;
#44307 = CARTESIAN_POINT ( 'NONE',  ( 121.0543159103642239, -8.454079026182057532, -17.47208793939445215 ) ) ;
#44308 = CARTESIAN_POINT ( 'NONE',  ( 106.1764733795248219, -8.938348069036489818, -17.46756447353520159 ) ) ;
#44309 = CARTESIAN_POINT ( 'NONE',  ( 112.2883483795247770, -8.402594152722688392, -16.93181055722141792 ) ) ;
#44310 = CARTESIAN_POINT ( 'NONE',  ( 107.9128015045248219, -2.477300249445798297, -7.631215200338321125 ) ) ;
#44311 = CARTESIAN_POINT ( 'NONE',  ( 122.2696148109119889, -4.089484607189486809, -7.948022111789456723 ) ) ;
#44312 = CARTESIAN_POINT ( 'NONE',  ( 122.9503348109119827, -9.859900752359378018, -12.68260735090039759 ) ) ;
#44313 = ORIENTED_EDGE ( 'NONE', *, *, #12029, .T. ) ;
#44314 = CARTESIAN_POINT ( 'NONE',  ( 123.8579614775786126, 0.5811942927096110934, -14.16772938898807510 ) ) ;
#44315 = CARTESIAN_POINT ( 'NONE',  ( 113.7606148109119886, -7.894159318335828068, -9.358103419637847864 ) ) ;
#44316 = CARTESIAN_POINT ( 'NONE',  ( 59.62174278132244609, -14.86814543204979522, -18.19321520033831874 ) ) ;
#44317 = CARTESIAN_POINT ( 'NONE',  ( 119.9438214775786378, -7.893985811506177619, -18.51759400769804742 ) ) ;
#44318 = CARTESIAN_POINT ( 'NONE',  ( 122.7234281442452755, -5.638512984488999180, -18.83840828888717311 ) ) ;
#44319 = CARTESIAN_POINT ( 'NONE',  ( 62.51884409362852324, -3.500628399893147336, -19.21898247060032006 ) ) ;
#44320 = CARTESIAN_POINT ( 'NONE',  ( 124.3685014775786328, 0.4262465694468514643, -12.03445270309931736 ) ) ;
#44321 = DIRECTION ( 'NONE',  ( 0.000000000000000000, -0.3818493186865927203, 0.9242245927363029745 ) ) ;
#44322 = DIRECTION ( 'NONE',  ( 0.9498278979187092519, 0.3127730236694430399, -0.000000000000000000 ) ) ;
#44323 = ORIENTED_EDGE ( 'NONE', *, *, #11060, .T. ) ;
#44324 = CARTESIAN_POINT ( 'NONE',  ( -1.637506834317629112, -6.775152287193631828, -8.718355983560822864 ) ) ;
#44325 = CARTESIAN_POINT ( 'NONE',  ( 84.10862215250544693, -25.99489077589524300, -13.39321520033831625 ) ) ;
#44326 = CARTESIAN_POINT ( 'NONE',  ( 122.8936081442453059, -9.565557343593413364, -10.61323700422348004 ) ) ;
#44327 = CARTESIAN_POINT ( 'NONE',  ( 106.5237390045248418, -9.868328341294098749, -11.32035403202665869 ) ) ;
#44328 = CARTESIAN_POINT ( 'NONE',  ( 113.2606921295247702, -9.868328341294093420, -13.39321520033831447 ) ) ;
#44329 = CARTESIAN_POINT ( 'NONE',  ( 116.3700414775786527, -4.153390946401321671, -8.397313243818183892 ) ) ;
#44330 = CARTESIAN_POINT ( 'NONE',  ( 114.3846081442453197, 0.4262465694468514643, -12.03445270309931736 ) ) ;
#44331 = CARTESIAN_POINT ( 'NONE',  ( 123.5176014775786228, -9.261995988541697145, -16.69588392320189030 ) ) ;
#44332 = ORIENTED_EDGE ( 'NONE', *, *, #7095, .F. ) ;
#44333 = CARTESIAN_POINT ( 'NONE',  ( 122.2128881442453263, -7.643976991954077427, -18.09477374809248928 ) ) ;
#44334 = CARTESIAN_POINT ( 'NONE',  ( 117.7314814775786260, -4.089484607189486809, -7.948022111789456723 ) ) ;
#44335 = CARTESIAN_POINT ( 'NONE',  ( 125.1059481442452750, -8.166667518702819706, -8.995218007635861213 ) ) ;
#44336 = CARTESIAN_POINT ( 'NONE',  ( 123.8012348109119642, -9.565557343593413364, -10.61323700422348004 ) ) ;
#44337 = EDGE_LOOP ( 'NONE', ( #3269, #15132, #15589, #8903 ) ) ;
#44338 = EDGE_CURVE ( 'NONE', #3386, #5770, #41717, .T. ) ;
#44339 = CARTESIAN_POINT ( 'NONE',  ( 123.2697102440515238, -2.467220198592778413, -17.83387418641524391 ) ) ;
#44340 = CARTESIAN_POINT ( 'NONE',  ( 123.6877814775786533, -3.383040157471821630, -19.15922257007629170 ) ) ;
#44341 = CARTESIAN_POINT ( 'NONE',  ( 114.6115148109119986, -6.222761293078241884, -8.102969835052219238 ) ) ;
#44342 = CARTESIAN_POINT ( 'NONE',  ( 123.9714148109119805, -0.4660016031367893996, -10.09054647747474043 ) ) ;
#44343 = CARTESIAN_POINT ( 'NONE',  ( 106.6626452545248611, 0.8980012041604421569, -11.00651665394454071 ) ) ;
#44344 = CARTESIAN_POINT ( 'NONE',  ( 122.8688454359119646, 0.5291689781388270175, -13.89700978578772705 ) ) ;
#44345 = ORIENTED_EDGE ( 'NONE', *, *, #790, .F. ) ;
#44346 = DIRECTION ( 'NONE',  ( -0.000000000000000000, -0.9284778069183721172, -0.3713878862591650232 ) ) ;
#44347 = CARTESIAN_POINT ( 'NONE',  ( 109.3018640045248304, 0.1403307496149616695, -15.46607636864997204 ) ) ;
#44348 = CARTESIAN_POINT ( 'NONE',  ( 70.19189222814998175, -60.97346038181336070, -37.59218076343751136 ) ) ;
#44349 = CARTESIAN_POINT ( 'NONE',  ( 118.8660148109119774, 0.1319031606808879209, -14.10382304977623669 ) ) ;
#44350 = CARTESIAN_POINT ( 'NONE',  ( 112.9097148109120070, -9.565557343593413364, -10.61323700422348004 ) ) ;
#44351 = CARTESIAN_POINT ( 'NONE',  ( 124.3521044615884392, -7.410781304726307361, -20.93588303426278685 ) ) ;
#44352 = ORIENTED_EDGE ( 'NONE', *, *, #38003, .F. ) ;
#44353 = CARTESIAN_POINT ( 'NONE',  ( 67.84197459855160162, -58.29708508664516842, -37.25081299080650865 ) ) ;
#44354 = CARTESIAN_POINT ( 'NONE',  ( 121.0216281442452981, -7.894159318335828068, -9.358103419637847864 ) ) ;
#44355 = CARTESIAN_POINT ( 'NONE',  ( 116.0852504229301729, 0.1075849324168598464, -14.64321520033831447 ) ) ;
#44356 = CARTESIAN_POINT ( 'NONE',  ( 69.69189222814998175, -41.76310523276723785, -7.393215200338315363 ) ) ;
#44357 = CARTESIAN_POINT ( 'NONE',  ( 111.6155414775786596, 0.3778260857407392814, -12.04688916545883792 ) ) ;
#44359 = CARTESIAN_POINT ( 'NONE',  ( 123.7445081442452874, -1.561330072975668948, -17.79121239304076951 ) ) ;
#44358 = CARTESIAN_POINT ( 'NONE',  ( 70.26514696789978132, -26.36317451685219027, -5.635745540951655030 ) ) ;
#44360 = CARTESIAN_POINT ( 'NONE',  ( 126.1837548109119496, 0.4262465694468514643, -12.03445270309931736 ) ) ;
#44361 = VERTEX_POINT ( 'NONE', #40063 ) ;
#44362 = CARTESIAN_POINT ( 'NONE',  ( 112.6260814775786514, -9.261995988541697145, -16.69588392320189030 ) ) ;
#44363 = DIRECTION ( 'NONE',  ( 0.000000000000000000, 0.000000000000000000, -1.000000000000000000 ) ) ;
#44364 = CARTESIAN_POINT ( 'NONE',  ( 114.8581140045248361, -10.62599879583958717, -11.00651665394454604 ) ) ;
#44365 = EDGE_CURVE ( 'NONE', #8725, #42142, #8034, .T. ) ;
#44366 = CARTESIAN_POINT ( 'NONE',  ( 112.0020881442453344, 0.2603800115204892296, -16.42320221600525088 ) ) ;
#44367 = CARTESIAN_POINT ( 'NONE',  ( 119.4332814775786318, -8.899110576539710493, -16.42337572283490132 ) ) ;
#44368 = CARTESIAN_POINT ( 'NONE',  ( 59.69399050597295542, -13.58096788970640567, -18.18301750815651374 ) ) ;
#44369 = CARTESIAN_POINT ( 'NONE',  ( 113.1217858795247935, -8.402594152722688392, -9.854619843455216355 ) ) ;
#44370 = CARTESIAN_POINT ( 'NONE',  ( 61.69189222814998175, -66.36873802749349238, -42.40236911872441539 ) ) ;
#44371 = DIRECTION ( 'NONE',  ( -0.5735764363510446051, 0.3127926500124816878, -0.7570804645221042017 ) ) ;
#44372 = CARTESIAN_POINT ( 'NONE',  ( 114.8384214775786489, -10.15424416112533912, -14.75197769757731336 ) ) ;
#44373 = CARTESIAN_POINT ( 'NONE',  ( 109.0935046295247872, -4.863998795839590272, -7.631215200338315796 ) ) ;
#44374 = CARTESIAN_POINT ( 'NONE',  ( 61.69189222814998175, -49.76310523276723785, -7.393215200338315363 ) ) ;
#44375 = CARTESIAN_POINT ( 'NONE',  ( 114.0941296295247867, -4.863998795839590272, -19.15521520033831493 ) ) ;
#44376 = CARTESIAN_POINT ( 'NONE',  ( 124.3117748109119844, -10.30919188438810075, -12.61870101168855918 ) ) ;
#44377 = CARTESIAN_POINT ( 'NONE',  ( 120.7947214775786193, -9.261995988541697145, -16.69588392320189030 ) ) ;
#44378 = LINE ( 'NONE', #6050, #40855 ) ;
#44379 = CARTESIAN_POINT ( 'NONE',  ( 121.9859814775786333, 0.2603800115204892296, -16.42320221600525088 ) ) ;
#44380 = FACE_OUTER_BOUND ( 'NONE', #14887, .T. ) ;
#44381 = VERTEX_POINT ( 'NONE', #2828 ) ;
#44382 = CARTESIAN_POINT ( 'NONE',  ( 112.1722681442453222, -8.899110576539710493, -16.42337572283490132 ) ) ;
#44383 = CARTESIAN_POINT ( 'NONE',  ( 124.8223148109119762, 0.9020085738987339008, -11.91225656197089222 ) ) ;
#44384 = CARTESIAN_POINT ( 'NONE',  ( 123.8579614775786126, 0.5811942927096110934, -14.16772938898807510 ) ) ;
#44385 = CARTESIAN_POINT ( 'NONE',  ( 114.2711548109119803, -9.988377603198976828, -10.36322818467138340 ) ) ;
#44386 = CARTESIAN_POINT ( 'NONE',  ( 113.9307948109119764, -10.15424416112533912, -14.75197769757731336 ) ) ;
#44387 = ORIENTED_EDGE ( 'NONE', *, *, #22776, .T. ) ;
#44388 = CARTESIAN_POINT ( 'NONE',  ( 116.9940348109119839, -0.1624402480850797581, -16.17319339645315424 ) ) ;
#44389 = CARTESIAN_POINT ( 'NONE',  ( 105.7597546295248350, -4.863998795839590272, -7.631215200338315796 ) ) ;
#44390 = CARTESIAN_POINT ( 'NONE',  ( 112.7745202545247878, 0.1403307496149616695, -11.32035403202665336 ) ) ;
#44391 = CIRCLE ( 'NONE', #21821, 5.000000000000004441 ) ;
#44392 = CARTESIAN_POINT ( 'NONE',  ( 122.4965214775786251, 0.1319031606808879209, -14.10382304977623669 ) ) ;
#44393 = CARTESIAN_POINT ( 'NONE',  ( 116.8497197753081451, -0.6930611473297154657, -16.59100722635417213 ) ) ;
#44394 = CARTESIAN_POINT ( 'NONE',  ( 113.2606921295247702, 0.8980012041604618078, -13.39321520033831447 ) ) ;
#44395 = EDGE_LOOP ( 'NONE', ( #34710, #16694 ) ) ;
#44396 = VECTOR ( 'NONE', #38064, 1000.000000000000000 ) ;
#44397 = CARTESIAN_POINT ( 'NONE',  ( 114.5700137256649072, -1.063912429576158614, -17.20460841810473696 ) ) ;
#44398 = CARTESIAN_POINT ( 'NONE',  ( 70.19189222814998175, -59.47700027789979060, -36.99360193826534271 ) ) ;
#44399 = CARTESIAN_POINT ( 'NONE',  ( 112.8439733795247832, -1.325403438956533675, -9.854619843455175499 ) ) ;
#44400 = CARTESIAN_POINT ( 'NONE',  ( 112.6260814775786514, -9.261995988541697145, -16.69588392320189030 ) ) ;
#44401 = CARTESIAN_POINT ( 'NONE',  ( 112.8337832127138682, -2.191907684172563986, -18.20049396185734025 ) ) ;
#44402 = CARTESIAN_POINT ( 'NONE',  ( 123.2184548109119788, -6.965697074025154478, -10.59448971407311646 ) ) ;
#44403 = CARTESIAN_POINT ( 'NONE',  ( 107.2182702545248105, 0.1403307496149616695, -11.32035403202665336 ) ) ;
#44404 = CARTESIAN_POINT ( 'NONE',  ( 111.0884957829843813, 0.6362173239733635022, -14.64321520033831447 ) ) ;
#44405 = CARTESIAN_POINT ( 'NONE',  ( 119.0361948109119652, -7.893985811506177619, -18.51759400769804742 ) ) ;
#44406 = CARTESIAN_POINT ( 'NONE',  ( 123.1466579359119891, -4.360204210389825086, -8.000047426360248792 ) ) ;
#44407 = CYLINDRICAL_SURFACE ( 'NONE', #30328, 3.000000000000001776 ) ;
#44408 = CARTESIAN_POINT ( 'NONE',  ( 124.8790414775786246, -0.4660016031367893996, -10.09054647747474043 ) ) ;
#44409 = CARTESIAN_POINT ( 'NONE',  ( 122.0994348109119443, -10.15424416112533912, -14.75197769757731336 ) ) ;
#44410 = CARTESIAN_POINT ( 'NONE',  ( 124.8790414775786246, -8.899110576539710493, -16.42337572283490132 ) ) ;
#44411 = ORIENTED_EDGE ( 'NONE', *, *, #10836, .T. ) ;
#44412 = CARTESIAN_POINT ( 'NONE',  ( 124.0281414775786146, -1.834011780172310813, -8.268836392978581529 ) ) ;
#44413 = CARTESIAN_POINT ( 'NONE',  ( 117.9583881442453048, -10.30919188438810075, -12.61870101168855918 ) ) ;
#44414 = LINE ( 'NONE', #20913, #22635 ) ;
#44415 = FACE_OUTER_BOUND ( 'NONE', #7447, .T. ) ;
#44416 = CARTESIAN_POINT ( 'NONE',  ( 122.3263414775786373, -6.344957434206665248, -7.627207830600338134 ) ) ;
#44417 = CARTESIAN_POINT ( 'NONE',  ( 112.8439733795247832, -8.938348069036489818, -17.46756447353520159 ) ) ;
#44418 = CARTESIAN_POINT ( 'NONE',  ( 105.7597546295248350, -4.863998795839590272, -18.39754474579285315 ) ) ;
#44419 = CARTESIAN_POINT ( 'NONE',  ( 96.46827370896536991, -25.99489077589524300, -13.39321520033831447 ) ) ;
#44420 = CARTESIAN_POINT ( 'NONE',  ( 116.3700414775786527, -4.153390946401321671, -8.397313243818183892 ) ) ;
#44421 = CARTESIAN_POINT ( 'NONE',  ( 118.3554748109119998, -9.565557343593413364, -10.61323700422348004 ) ) ;
#44422 = VECTOR ( 'NONE', #1815, 1000.000000000000114 ) ;
#44423 = CARTESIAN_POINT ( 'NONE',  ( 112.8914883310706898, 0.1843591316377651834, -12.14321520033831625 ) ) ;
#44424 = CARTESIAN_POINT ( 'NONE',  ( 112.7050671295247923, 0.1403307496149613920, -13.39321520033831447 ) ) ;
#44425 = ORIENTED_EDGE ( 'NONE', *, *, #23925, .F. ) ;
#44426 = CARTESIAN_POINT ( 'NONE',  ( 41.72636039845269096, -11.37347657059392070, -8.893215200338314474 ) ) ;
#44427 = CARTESIAN_POINT ( 'NONE',  ( 115.1220548109119761, -8.166667518702817929, -8.995218007635861213 ) ) ;
#44428 = FACE_OUTER_BOUND ( 'NONE', #26869, .T. ) ;
#44429 = CARTESIAN_POINT ( 'NONE',  ( 124.1884548109119777, -7.554583864224885481, -18.48844787311982785 ) ) ;
#44430 = CARTESIAN_POINT ( 'NONE',  ( 122.5215798109119874, -7.200787124940443817, -17.81845355600750835 ) ) ;
#44431 = VERTEX_POINT ( 'NONE', #1750 ) ;
#44432 = CARTESIAN_POINT ( 'NONE',  ( 70.86891319097370001, -49.31949126737637812, -35.46156944284200563 ) ) ;
#44433 = CARTESIAN_POINT ( 'NONE',  ( 116.6114517406422380, -11.86984128825793228, -21.21871708423150693 ) ) ;
#44434 = ORIENTED_EDGE ( 'NONE', *, *, #9214, .F. ) ;
#44435 = CARTESIAN_POINT ( 'NONE',  ( 117.0507614775786465, -10.30919188438810075, -12.61870101168855918 ) ) ;
#44436 = VECTOR ( 'NONE', #41271, 1000.000000000000000 ) ;
#44437 = CARTESIAN_POINT ( 'NONE',  ( 124.0848681442452772, -5.574606645277164318, -18.38911715685844683 ) ) ;
#44438 = ADVANCED_FACE ( 'NONE', ( #29578 ), #26028, .T. ) ;
#44439 = CARTESIAN_POINT ( 'NONE',  ( 117.5045748109119756, -9.859900752359374465, -12.68260735090039404 ) ) ;
#44440 = CONICAL_SURFACE ( 'NONE', #40057, 2.999999999999999556, 0.9599310885968830309 ) ;
#44441 = CARTESIAN_POINT ( 'NONE',  ( 71.02242295334774269, -56.90992360313401122, -39.07158786529310390 ) ) ;
#44442 = CARTESIAN_POINT ( 'NONE',  ( 123.1205148109119563, -1.834011780172310813, -8.268836392978581529 ) ) ;
#44443 = CARTESIAN_POINT ( 'NONE',  ( 119.9438214775786378, -7.893985811506177619, -18.51759400769804742 ) ) ;
#44444 = CARTESIAN_POINT ( 'NONE',  ( 111.3160046295247838, -4.863998795839590272, -18.39754474579285315 ) ) ;
#44445 = CARTESIAN_POINT ( 'NONE',  ( 113.5337081442453240, -0.8288870151387760510, -10.36305467784173118 ) ) ;
#44446 = FACE_OUTER_BOUND ( 'NONE', #36459, .T. ) ;
#44447 = ORIENTED_EDGE ( 'NONE', *, *, #20334, .F. ) ;
#44448 = CARTESIAN_POINT ( 'NONE',  ( 118.5823814775786360, -1.834011780172310813, -8.268836392978581529 ) ) ;
#44449 = CARTESIAN_POINT ( 'NONE',  ( 126.6827570900183844, -4.792845811650923160, -18.62498157970546941 ) ) ;
#44450 = CARTESIAN_POINT ( 'NONE',  ( 111.8886348109120092, -3.383040157471821630, -19.15922257007629170 ) ) ;
#44451 = VERTEX_POINT ( 'NONE', #36627 ) ;
#44452 = CARTESIAN_POINT ( 'NONE',  ( 121.8725281442453223, -3.383040157471821630, -19.15922257007629170 ) ) ;
#44453 = CIRCLE ( 'NONE', #24779, 2.000000000000000444 ) ;
#44454 = LINE ( 'NONE', #26666, #29619 ) ;
#44455 = CARTESIAN_POINT ( 'NONE',  ( 112.9664414775786412, -9.859900752359374465, -12.68260735090039404 ) ) ;
#44456 = CARTESIAN_POINT ( 'NONE',  ( 70.19189222814998175, -61.90193818873174791, -37.96356864969668266 ) ) ;
#44457 = CARTESIAN_POINT ( 'NONE',  ( 117.9016614775786280, -0.1624402480850797581, -16.17319339645315424 ) ) ;
#44458 = CARTESIAN_POINT ( 'NONE',  ( 123.7017273619992466, -4.637278545147846209, -14.94411704847414946 ) ) ;
#44459 = CARTESIAN_POINT ( 'NONE',  ( 118.5256548109119876, -8.899110576539710493, -16.42337572283490132 ) ) ;
#44460 = DIRECTION ( 'NONE',  ( -0.000000000000000000, -0.9284778069183718952, -0.3713878862591649677 ) ) ;
#44461 = CARTESIAN_POINT ( 'NONE',  ( 114.1009748109119784, -5.574606645277164318, -18.38911715685844683 ) ) ;
#44462 = AXIS2_PLACEMENT_3D ( 'NONE', #27856, #17587, #251 ) ;
#44463 = CARTESIAN_POINT ( 'NONE',  ( 114.7249681442453237, 0.2603800115204892296, -16.42320221600525088 ) ) ;
#44464 = CARTESIAN_POINT ( 'NONE',  ( 122.7299391859119737, -1.406689858478933353, -17.56299727309130887 ) ) ;
#44465 = CARTESIAN_POINT ( 'NONE',  ( 112.9097148109120070, 0.2603800115204892296, -16.42320221600525088 ) ) ;
#44466 = CARTESIAN_POINT ( 'NONE',  ( 115.2355081442453155, 0.1319031606808879209, -14.10382304977623669 ) ) ;
#44467 = CARTESIAN_POINT ( 'NONE',  ( 124.1983214775786166, -8.166667518702819706, -8.995218007635861213 ) ) ;
#44468 = CARTESIAN_POINT ( 'NONE',  ( 116.3700414775786527, -4.153390946401321671, -8.397313243818183892 ) ) ;
#44469 = ORIENTED_EDGE ( 'NONE', *, *, #5532, .F. ) ;
#44470 = CARTESIAN_POINT ( 'NONE',  ( 113.4202548109119846, -10.30919188438810075, -12.61870101168855918 ) ) ;
#44471 = CARTESIAN_POINT ( 'NONE',  ( 105.5513952545248060, 0.8980012041604421569, -11.00651665394454071 ) ) ;
#44472 = CARTESIAN_POINT ( 'NONE',  ( 85.04324155394569118, -24.14644159042263993, -12.62951656296512937 ) ) ;
#44473 = LINE ( 'NONE', #16432, #8705 ) ;
#44474 = CARTESIAN_POINT ( 'NONE',  ( 64.61935771200890599, -37.86087448816891765, -4.893215200338314474 ) ) ;
#44475 = CARTESIAN_POINT ( 'NONE',  ( 120.6245414775786458, -9.988377603198976828, -10.36322818467138340 ) ) ;
#44476 = ORIENTED_EDGE ( 'NONE', *, *, #38622, .T. ) ;
#44477 = DIRECTION ( 'NONE',  ( -1.000000000000000000, 0.000000000000000000, 0.000000000000000000 ) ) ;
#44478 = CARTESIAN_POINT ( 'NONE',  ( 120.5861007241439324, -2.443475742715334853, -17.86549347949429389 ) ) ;
#44479 = CARTESIAN_POINT ( 'NONE',  ( 117.7882081442453170, -3.505236298600246325, -18.68346056562440793 ) ) ;
#44480 = CARTESIAN_POINT ( 'NONE',  ( 88.46631044337289040, -25.99489077589524300, -13.39321520033831625 ) ) ;
#44481 = CARTESIAN_POINT ( 'NONE',  ( 124.8223148109119762, 0.9020085738987339008, -11.91225656197089222 ) ) ;
#44482 = CARTESIAN_POINT ( 'NONE',  ( 106.4542858795248179, -0.7896495226426338832, -17.46756447353520159 ) ) ;
#44483 = CARTESIAN_POINT ( 'NONE',  ( 89.15006894847832086, -10.38507692083869038, -14.05253605978568743 ) ) ;
#44484 = EDGE_LOOP ( 'NONE', ( #41540, #20814, #21181, #21379, #21384 ) ) ;
#44485 = CARTESIAN_POINT ( 'NONE',  ( 111.8886348109120092, -3.383040157471821630, -19.15922257007629170 ) ) ;
#44486 = CARTESIAN_POINT ( 'NONE',  ( 124.1415948109119540, -3.505236298600246325, -18.68346056562440793 ) ) ;
#44487 = CARTESIAN_POINT ( 'NONE',  ( 120.1140014775786398, -1.561330072975668504, -17.79121239304076951 ) ) ;
#44488 = AXIS2_PLACEMENT_3D ( 'NONE', #19845, #2504, #26910 ) ;
#44489 = CARTESIAN_POINT ( 'NONE',  ( 114.1009748109119784, -5.574606645277164318, -18.38911715685844683 ) ) ;
#44490 = CARTESIAN_POINT ( 'NONE',  ( 118.0718414775786300, -9.261995988541697145, -16.69588392320189030 ) ) ;
#44491 = CARTESIAN_POINT ( 'NONE',  ( 80.41643495664496299, -3.865424785743139857, -15.89321520033831447 ) ) ;
#44492 = CARTESIAN_POINT ( 'NONE',  ( 119.7434548109119703, -3.874292970208447873, -21.33175929725637587 ) ) ;
#44493 = CARTESIAN_POINT ( 'NONE',  ( 117.7314814775786260, -5.574606645277164318, -18.38911715685844683 ) ) ;
#44494 = VERTEX_POINT ( 'NONE', #16985 ) ;
#44495 = CARTESIAN_POINT ( 'NONE',  ( 121.4103298109119748, -2.173413727453600508, -8.297982527556802879 ) ) ;
#44496 = CIRCLE ( 'NONE', #4409, 5.999999999999997335 ) ;
#44497 = CARTESIAN_POINT ( 'NONE',  ( 115.8595014775786609, -1.834011780172310813, -8.268836392978581529 ) ) ;
#44498 = CARTESIAN_POINT ( 'NONE',  ( 121.0216281442452981, -7.894159318335828068, -9.358103419637847864 ) ) ;
#44499 = VERTEX_POINT ( 'NONE', #30877 ) ;
#44500 = VECTOR ( 'NONE', #22791, 1000.000000000000114 ) ;
#44501 = CARTESIAN_POINT ( 'NONE',  ( 122.3826735609119680, -9.645473719204776586, -14.86997237629376656 ) ) ;
#44502 = CARTESIAN_POINT ( 'NONE',  ( 61.93073106961468000, -12.47488654111867312, -9.789137930298094759 ) ) ;
#44503 = CARTESIAN_POINT ( 'NONE',  ( 117.0507614775786465, -10.30919188438810075, -12.61870101168855918 ) ) ;
#44504 = CARTESIAN_POINT ( 'NONE',  ( 111.0381921295247878, 0.8980012041604618078, -13.39321520033831447 ) ) ;
#44505 = CARTESIAN_POINT ( 'NONE',  ( 115.6893214775786447, -9.859900752359374465, -12.68260735090039404 ) ) ;
#44506 = ORIENTED_EDGE ( 'NONE', *, *, #40982, .T. ) ;
#44507 = VERTEX_POINT ( 'NONE', #44796 ) ;
#44508 = CARTESIAN_POINT ( 'NONE',  ( 112.5126281442453120, -10.30919188438810075, -12.61870101168855918 ) ) ;
#44509 = CARTESIAN_POINT ( 'NONE',  ( 125.6164881442453094, -9.565557343593413364, -10.61323700422348004 ) ) ;
#44510 = DIRECTION ( 'NONE',  ( -0.1352586133457950590, -0.9908103287288504424, 0.000000000000000000 ) ) ;
#44511 = CYLINDRICAL_SURFACE ( 'NONE', #14129, 1.999999999999998890 ) ;
#44512 = CARTESIAN_POINT ( 'NONE',  ( 122.8936081442453059, 0.2603800115204892296, -16.42320221600525088 ) ) ;
#44513 = DIRECTION ( 'NONE',  ( -1.000000000000000000, 0.000000000000000000, 0.000000000000000000 ) ) ;
#44514 = DIRECTION ( 'NONE',  ( -0.2768435750659241079, -0.3568721902840695792, 0.8921882507333129819 ) ) ;
#44515 = CARTESIAN_POINT ( 'NONE',  ( 121.1350814775786233, 0.5811942927096110934, -14.16772938898807510 ) ) ;
#44517 = CARTESIAN_POINT ( 'NONE',  ( 119.7736414775786358, 0.1319031606808879209, -14.10382304977623669 ) ) ;
#44516 = CARTESIAN_POINT ( 'NONE',  ( 119.8870948109119752, -9.261995988541697145, -16.69588392320189030 ) ) ;
#44518 = CARTESIAN_POINT ( 'NONE',  ( 124.0281414775786146, -7.643976991954077427, -18.09477374809248928 ) ) ;
#44519 = CARTESIAN_POINT ( 'NONE',  ( 113.0231681442453322, 0.9020085738987339008, -11.91225656197089222 ) ) ;
#44520 = ADVANCED_FACE ( 'NONE', ( #41386 ), #23831, .T. ) ;
#44521 = ORIENTED_EDGE ( 'NONE', *, *, #23105, .T. ) ;
#44522 = CARTESIAN_POINT ( 'NONE',  ( 125.0492214775786266, -3.505236298600246325, -18.68346056562440793 ) ) ;
#44523 = CARTESIAN_POINT ( 'NONE',  ( 122.3255085810856997, -1.220279397241718966, -16.99638242193886484 ) ) ;
#44524 = CARTESIAN_POINT ( 'NONE',  ( 121.3655035264548872, -8.247323210606168686, -17.08054893949881148 ) ) ;
#44525 = CARTESIAN_POINT ( 'NONE',  ( 109.5796765045248122, -7.250697342233347165, -19.15521520033831138 ) ) ;
#44526 = AXIS2_PLACEMENT_3D ( 'NONE', #8086, #14927, #8982 ) ;
#44527 = CARTESIAN_POINT ( 'NONE',  ( 111.3160046295247838, -4.863998795839590272, -18.39754474579285315 ) ) ;
#44528 = CARTESIAN_POINT ( 'NONE',  ( 106.6626452545248611, 0.8980012041604421569, -11.00651665394454071 ) ) ;
#44529 = CARTESIAN_POINT ( 'NONE',  ( 122.4397948109119767, -9.988377603198976828, -10.36322818467138340 ) ) ;
#44530 = CARTESIAN_POINT ( 'NONE',  ( 121.5321681442453183, -0.1624402480850797581, -16.17319339645315424 ) ) ;
#44531 = EDGE_CURVE ( 'NONE', #41378, #15181, #17284, .T. ) ;
#44532 = ORIENTED_EDGE ( 'NONE', *, *, #29013, .T. ) ;
#44533 = CARTESIAN_POINT ( 'NONE',  ( 123.0637881442452937, -0.4660016031367893996, -10.09054647747474043 ) ) ;
#44534 = CARTESIAN_POINT ( 'NONE',  ( 114.1577014775786552, -3.505236298600246325, -18.68346056562440793 ) ) ;
#44535 = CARTESIAN_POINT ( 'NONE',  ( 121.8158014775786171, -4.153390946401271933, -8.397313243818190998 ) ) ;
#44536 = CARTESIAN_POINT ( 'NONE',  ( 121.3619881442452879, -4.089484607189486809, -7.948022111789456723 ) ) ;
#44537 = CARTESIAN_POINT ( 'NONE',  ( 120.2841814775786276, 0.9020085738987339008, -11.91225656197089222 ) ) ;
#44538 = FACE_OUTER_BOUND ( 'NONE', #31047, .T. ) ;
#44539 = CARTESIAN_POINT ( 'NONE',  ( 126.5808414775786446, -9.859900752359378018, -12.68260735090039759 ) ) ;
#44540 = CARTESIAN_POINT ( 'NONE',  ( 111.6573126359456012, -1.179503403430504527, -17.05068175419384957 ) ) ;
#44541 = CARTESIAN_POINT ( 'NONE',  ( 105.6903015045248253, -2.477300249445798297, -7.631215200338321125 ) ) ;
#44542 = VERTEX_POINT ( 'NONE', #38823 ) ;
#44543 = CARTESIAN_POINT ( 'NONE',  ( 78.69189222814998175, -50.16718729050182191, 3.106784799661685526 ) ) ;
#44544 = CARTESIAN_POINT ( 'NONE',  ( 112.2289948109119848, -7.643976991954077427, -18.09477374809248928 ) ) ;
#44545 = CARTESIAN_POINT ( 'NONE',  ( 125.2194014775786286, 0.1319031606808879209, -14.10382304977623669 ) ) ;
#44546 = CARTESIAN_POINT ( 'NONE',  ( 108.3295202545248657, 0.1403307496149616695, -11.32035403202665336 ) ) ;
#44547 = CARTESIAN_POINT ( 'NONE',  ( 109.6491296295247793, -4.863998795839590272, -8.388885654883775800 ) ) ;
#44548 = CARTESIAN_POINT ( 'NONE',  ( 120.5678148109119832, -1.833838273342659253, -17.42832698103878286 ) ) ;
#44549 =( NAMED_UNIT ( * ) SI_UNIT ( $, .STERADIAN. ) SOLID_ANGLE_UNIT ( ) );
#44550 = CARTESIAN_POINT ( 'NONE',  ( 114.9518748109119883, -7.643976991954077427, -18.09477374809248928 ) ) ;
#44551 = CARTESIAN_POINT ( 'NONE',  ( 124.8223148109119762, 0.9020085738987339008, -11.91225656197089222 ) ) ;
#44552 = ORIENTED_EDGE ( 'NONE', *, *, #14501, .F. ) ;
#44553 = EDGE_CURVE ( 'NONE', #26397, #2604, #19993, .T. ) ;
#44554 = CARTESIAN_POINT ( 'NONE',  ( 121.6456214775786293, 0.4262465694468514643, -12.03445270309931736 ) ) ;
#44555 = CARTESIAN_POINT ( 'NONE',  ( 118.2987481442453088, -1.561330072975668504, -17.79121239304076951 ) ) ;
#44556 = CARTESIAN_POINT ( 'NONE',  ( 123.6310548109119765, -5.638512984488999180, -18.83840828888717311 ) ) ;
#44557 = CARTESIAN_POINT ( 'NONE',  ( 122.8368814775786291, -7.894159318335828068, -9.358103419637847864 ) ) ;
#44558 = VERTEX_POINT ( 'NONE', #39283 ) ;
#44559 = FACE_OUTER_BOUND ( 'NONE', #11992, .T. ) ;
#44560 =( BOUNDED_SURFACE ( )  B_SPLINE_SURFACE ( 1, 2, ( 
 ( #39437, #35996, #18468, #1347, #18236, #4991, #35314, #4085, #32132, #900, #18009, #31908, #14590, #28508, #11179, #14819, #28732, #11403, #25310, #40567, #40796, #6125, #37117, #29395, #1566, #44221, #20044, #12752, #12302, #8648, #15489, #19582, #8871, #12075, #33016, #9551, #40108, #43306, #25979, #19133, #26429, #26652, #9327, #9100, #23467, #23234, #40335, #26202, #5889, #30076, #33463, #22770, #33700, #12528, #19811, #29845, #2470, #30295, #16396, #43988, #43762, #19360, #33246, #15944, #12982, #26878, #1791, #37353, #39885, #2020, #23001, #22548, #36669, #36447, #5216, #43533, #15716, #2241, #29618, #5440, #36893, #5663, #16172, #13655, #24579, #17080, #10015, #6810, #173, #20271, #44896, #2928, #14089, #17300, #31405, #41914, #27109, #6359, #41476, #41031, #37586, #28006, #16857, #44672, #24141, #31192, #30749, #30972, #34597, #10234, #27561, #17507, #34157, #38464, #7025, #45111, #7237, #20497, #13434, #38033, #34378, #38246, #10677, #6581, #3159, #20717, #30521, #13869, #27780, #3381, #41693, #27337, #3595, #10456, #24359, #41258, #23924, #13210, #33927, #2697, #23699, #16626, #37806, #20935, #34809, #44443, #9785, #15210, #25702, #11571, #3809, #21153, #18635, #39609, #32306, #31855, #28230, #35026, #39151, #28451, #31631, #7455, #29115, #14536, #17733, #399, #38690, #843, #1073, #14985, #28678, #43027, #42810, #14763, #624, #25478, #4492, #7916, #42360, #8149, #32076, #39384, #4262, #28899, #4715, #35946, #18414, #18181, #38916, #7687, #35488, #32523, #22053, #21374, #1298, #11795, #21601, #42580, #14314, #11122, #42137, #10898, #17956, #24798, #21826, #35257, #4034, #25022, #11343, #25254, #35720, #12931, #43484, #5392, #19310, #43257, #26374, #9048, #22948, #43935, #33640, #1966, #30016, #43702, #5609, #29790, #39831, #36841, #36617, #19533, #22718, #26829, #16116, #37063, #8370, #5836, #5161, #22276, #33409, #12475, #44168, #1517, #36170, #4936, #15436, #18851, #33191, #19758, #40284, #2186, #12701, #23185, #15893, #26601, #8817, #2416, #26147 ),
 ( #40514, #32743, #9277, #16342, #15664, #29343, #12251, #30245, #12022, #25925, #8597, #32964, #22495, #36390, #19078, #1741, #29566, #40049, #729, #31748, #71, #515, #17848, #13768, #31298, #13983, #3928, #24913, #10570, #17627, #14651, #6065, #10789, #31082, #17191, #27678, #41592, #24257, #27898, #35150, #11012, #38809, #9497, #31522, #7577, #10348, #21491, #24467, #41813, #35376, #38358, #45009, #292, #24686, #23412, #14426, #34919, #14206, #3707, #18071, #40740, #38145, #3492, #3266, #21044, #28120, #38574, #42248, #4155, #28336, #6919, #7133, #42027, #20826, #34488, #7352, #21268, #31964, #34706, #37296, #19984, #17409, #18965, #11236, #28566, #26036, #33074, #39718, #39268, #35605, #1846, #1404, #35829, #39039, #14879, #36507, #21937, #42475, #25145, #963, #8258, #8483, #22387, #36057, #5279, #5050, #22163, #8030, #32854, #11909, #15321, #4603, #15545, #39495, #1625, #11684, #36282, #12134, #43365, #25809, #25590, #1189, #15101, #42919, #39942, #29450, #28791, #8703, #22608, #29010, #4826, #19197, #18523, #4378, #7810, #25369, #21719, #29232, #18295, #11466, #32190, #42697, #32416, #18747, #32638, #43139, #44050, #36949, #33762, #27168, #2077, #26715, #29908, #41089, #44283, #13262, #23756, #8933, #33301, #23291, #22834, #19415, #9847, #43823, #26493, #5949, #13036, #12589, #12814, #16457, #37175, #40624, #44498, #16001, #6420, #33991, #26935, #34214, #2303, #40397, #19873, #16233, #20105, #37646, #33523, #30136, #2530, #12361, #40857, #9611, #30358, #23530, #9161, #30578, #9381, #37416, #23065, #5720, #40169, #20328, #15775, #5494, #29677, #19638, #6185, #2759, #43589, #16685, #26261, #36728, #14147, #21437, #34652, #20551, #38302, #3437, #7296, #14372, #20772, #17356, #10511, #44731, #28062, #41971, #7081, #10737, #41533, #17792, #41751, #20990, #27619, #38088, #27395, #31688, #10955, #37864, #7521, #3211, #34864, #24636, #34432, #38518, #42194, #2986, #21213, #30807, #16913, #456, #13490, #35090, #13712, #10076, #41317, #3651, #10291, #23978, #17137 ) ),
 .UNSPECIFIED., .F., .F., .T. ) 
 B_SPLINE_SURFACE_WITH_KNOTS ( ( 2, 2 ),
 ( 3, 2, 2, 2, 2, 2, 2, 2, 2, 2, 2, 2, 2, 2, 2, 2, 2, 2, 2, 2, 2, 2, 2, 2, 2, 2, 2, 2, 2, 2, 2, 2, 2, 2, 2, 2, 2, 2, 2, 2, 2, 2, 2, 2, 2, 2, 2, 2, 2, 2, 2, 2, 2, 2, 2, 2, 2, 2, 2, 2, 2, 2, 2, 2, 2, 2, 2, 2, 2, 2, 2, 2, 2, 2, 2, 2, 2, 2, 2, 2, 2, 2, 2, 2, 2, 2, 2, 2, 2, 2, 2, 2, 2, 2, 2, 2, 2, 2, 2, 2, 2, 2, 2, 2, 2, 2, 2, 2, 2, 2, 2, 2, 2, 2, 2, 2, 2, 2, 2, 2, 2, 2, 2, 2, 2, 2, 2, 2, 3 ),
 ( 0.000000000000000000, 1.000000000000000000 ),
 ( 0.000000000000000000, 0.007812500000000000000, 0.01562500000000000000, 0.02343750000000000000, 0.03125000000000000000, 0.03906250000000000000, 0.04687500000000000000, 0.05468750000000000000, 0.06250000000000000000, 0.07031250000000000000, 0.07812500000000000000, 0.08593750000000000000, 0.09375000000000000000, 0.1015625000000000000, 0.1093750000000000000, 0.1171875000000000000, 0.1250000000000000000, 0.1328125000000000000, 0.1406250000000000000, 0.1484375000000000000, 0.1562500000000000000, 0.1640625000000000000, 0.1718750000000000000, 0.1796875000000000000, 0.1875000000000000000, 0.1953125000000000000, 0.2031250000000000000, 0.2109375000000000000, 0.2187500000000000000, 0.2265625000000000000, 0.2343750000000000000, 0.2421875000000000000, 0.2500000000000000000, 0.2578125000000000000, 0.2656250000000000000, 0.2734375000000000000, 0.2812500000000000000, 0.2890625000000000000, 0.2968750000000000000, 0.3046875000000000000, 0.3125000000000000000, 0.3203125000000000000, 0.3281250000000000000, 0.3359375000000000000, 0.3437500000000000000, 0.3515625000000000000, 0.3593750000000000000, 0.3671875000000000000, 0.3750000000000000000, 0.3828125000000000000, 0.3906250000000000000, 0.3984375000000000000, 0.4062500000000000000, 0.4140625000000000000, 0.4218750000000000000, 0.4296875000000000000, 0.4375000000000000000, 0.4453125000000000000, 0.4531250000000000000, 0.4609375000000000000, 0.4687500000000000000, 0.4765625000000000000, 0.4843750000000000000, 0.4921875000000000000, 0.5000000000000000000, 0.5078125000000000000, 0.5156250000000000000, 0.5234375000000000000, 0.5312500000000000000, 0.5390625000000000000, 0.5468750000000000000, 0.5546875000000000000, 0.5625000000000000000, 0.5703125000000000000, 0.5781250000000000000, 0.5859375000000000000, 0.5937500000000000000, 0.6015625000000000000, 0.6093750000000000000, 0.6171875000000000000, 0.6250000000000000000, 0.6328125000000000000, 0.6406250000000000000, 0.6484375000000000000, 0.6562500000000000000, 0.6640625000000000000, 0.6718750000000000000, 0.6796875000000000000, 0.6875000000000000000, 0.6953125000000000000, 0.7031250000000000000, 0.7109375000000000000, 0.7187500000000000000, 0.7265625000000000000, 0.7343750000000000000, 0.7421875000000000000, 0.7500000000000000000, 0.7578125000000000000, 0.7656250000000000000, 0.7734375000000000000, 0.7812500000000000000, 0.7890625000000000000, 0.7968750000000000000, 0.8046875000000000000, 0.8125000000000000000, 0.8203125000000000000, 0.8281250000000000000, 0.8359375000000000000, 0.8437500000000000000, 0.8515625000000000000, 0.8593750000000000000, 0.8671875000000000000, 0.8750000000000000000, 0.8828125000000000000, 0.8906250000000000000, 0.8984375000000000000, 0.9062500000000000000, 0.9140625000000000000, 0.9218750000000000000, 0.9296875000000000000, 0.9375000000000000000, 0.9453125000000000000, 0.9531250000000000000, 0.9609375000000000000, 0.9687500000000000000, 0.9765625000000000000, 0.9843750000000000000, 0.9921875000000000000, 1.000000000000000000 ),
 .UNSPECIFIED. ) 
 GEOMETRIC_REPRESENTATION_ITEM ( )  RATIONAL_B_SPLINE_SURFACE ( (
 ( 1.000000000000000000, 0.9238795325112869605, 1.000000000000000000, 0.9238795325112869605, 1.000000000000000000, 0.9238795325112869605, 1.000000000000000000, 0.9238795325112869605, 1.000000000000000000, 0.9238795325112869605, 1.000000000000000000, 0.9238795325112869605, 1.000000000000000000, 0.9238795325112869605, 1.000000000000000000, 0.9238795325112869605, 1.000000000000000000, 0.9238795325112869605, 1.000000000000000000, 0.9238795325112869605, 1.000000000000000000, 0.9238795325112869605, 1.000000000000000000, 0.9238795325112869605, 1.000000000000000000, 0.9238795325112869605, 1.000000000000000000, 0.9238795325112869605, 1.000000000000000000, 0.9238795325112869605, 1.000000000000000000, 0.9238795325112869605, 1.000000000000000000, 0.9238795325112869605, 1.000000000000000000, 0.9238795325112869605, 1.000000000000000000, 0.9238795325112869605, 1.000000000000000000, 0.9238795325112869605, 1.000000000000000000, 0.9238795325112869605, 1.000000000000000000, 0.9238795325112869605, 1.000000000000000000, 0.9238795325112869605, 1.000000000000000000, 0.9238795325112869605, 1.000000000000000000, 0.9238795325112869605, 1.000000000000000000, 0.9238795325112869605, 1.000000000000000000, 0.9238795325112869605, 1.000000000000000000, 0.9238795325112869605, 1.000000000000000000, 0.9238795325112869605, 1.000000000000000000, 0.9238795325112869605, 1.000000000000000000, 0.9238795325112869605, 1.000000000000000000, 0.9238795325112869605, 1.000000000000000000, 0.9238795325112869605, 1.000000000000000000, 0.9238795325112869605, 1.000000000000000000, 0.9238795325112869605, 1.000000000000000000, 0.9238795325112869605, 1.000000000000000000, 0.9238795325112869605, 1.000000000000000000, 0.9238795325112869605, 1.000000000000000000, 0.9238795325112869605, 1.000000000000000000, 0.9238795325112869605, 1.000000000000000000, 0.9238795325112869605, 1.000000000000000000, 0.9238795325112869605, 1.000000000000000000, 0.9238795325112869605, 1.000000000000000000, 0.9238795325112869605, 1.000000000000000000, 0.9238795325112869605, 1.000000000000000000, 0.9238795325112869605, 1.000000000000000000, 0.9238795325112869605, 1.000000000000000000, 0.9238795325112869605, 1.000000000000000000, 0.9238795325112869605, 1.000000000000000000, 0.9238795325112869605, 1.000000000000000000, 0.9238795325112869605, 1.000000000000000000, 0.9238795325112869605, 1.000000000000000000, 0.9238795325112869605, 1.000000000000000000, 0.9238795325112869605, 1.000000000000000000, 0.9238795325112869605, 1.000000000000000000, 0.9238795325112869605, 1.000000000000000000, 0.9238795325112869605, 1.000000000000000000, 0.9238795325112869605, 1.000000000000000000, 0.9238795325112869605, 1.000000000000000000, 0.9238795325112869605, 1.000000000000000000, 0.9238795325112869605, 1.000000000000000000, 0.9238795325112869605, 1.000000000000000000, 0.9238795325112869605, 1.000000000000000000, 0.9238795325112869605, 1.000000000000000000, 0.9238795325112869605, 1.000000000000000000, 0.9238795325112869605, 1.000000000000000000, 0.9238795325112869605, 1.000000000000000000, 0.9238795325112869605, 1.000000000000000000, 0.9238795325112869605, 1.000000000000000000, 0.9238795325112869605, 1.000000000000000000, 0.9238795325112869605, 1.000000000000000000, 0.9238795325112869605, 1.000000000000000000, 0.9238795325112869605, 1.000000000000000000, 0.9238795325112869605, 1.000000000000000000, 0.9238795325112869605, 1.000000000000000000, 0.9238795325112869605, 1.000000000000000000, 0.9238795325112869605, 1.000000000000000000, 0.9238795325112869605, 1.000000000000000000, 0.9238795325112869605, 1.000000000000000000, 0.9238795325112869605, 1.000000000000000000, 0.9238795325112869605, 1.000000000000000000, 0.9238795325112869605, 1.000000000000000000, 0.9238795325112869605, 1.000000000000000000, 0.9238795325112869605, 1.000000000000000000, 0.9238795325112869605, 1.000000000000000000, 0.9238795325112869605, 1.000000000000000000, 0.9238795325112869605, 1.000000000000000000, 0.9238795325112869605, 1.000000000000000000, 0.9238795325112869605, 1.000000000000000000, 0.9238795325112869605, 1.000000000000000000, 0.9238795325112869605, 1.000000000000000000, 0.9238795325112869605, 1.000000000000000000, 0.9238795325112869605, 1.000000000000000000, 0.9238795325112869605, 1.000000000000000000, 0.9238795325112869605, 1.000000000000000000, 0.9238795325112869605, 1.000000000000000000, 0.9238795325112869605, 1.000000000000000000, 0.9238795325112869605, 1.000000000000000000, 0.9238795325112869605, 1.000000000000000000, 0.9238795325112869605, 1.000000000000000000, 0.9238795325112869605, 1.000000000000000000, 0.9238795325112869605, 1.000000000000000000, 0.9238795325112869605, 1.000000000000000000, 0.9238795325112869605, 1.000000000000000000, 0.9238795325112869605, 1.000000000000000000, 0.9238795325112869605, 1.000000000000000000, 0.9238795325112869605, 1.000000000000000000, 0.9238795325112869605, 1.000000000000000000, 0.9238795325112869605, 1.000000000000000000, 0.9238795325112869605, 1.000000000000000000, 0.9238795325112869605, 1.000000000000000000, 0.9238795325112869605, 1.000000000000000000, 0.9238795325112869605, 1.000000000000000000, 0.9238795325112869605, 1.000000000000000000, 0.9238795325112869605, 1.000000000000000000, 0.9238795325112869605, 1.000000000000000000, 0.9238795325112869605, 1.000000000000000000, 0.9238795325112869605, 1.000000000000000000, 0.9238795325112869605, 1.000000000000000000, 0.9238795325112869605, 1.000000000000000000, 0.9238795325112869605, 1.000000000000000000, 0.9238795325112869605, 1.000000000000000000, 0.9238795325112869605, 1.000000000000000000, 0.9238795325112869605, 1.000000000000000000, 0.9238795325112869605, 1.000000000000000000, 0.9238795325112869605, 1.000000000000000000, 0.9238795325112869605, 1.000000000000000000, 0.9238795325112869605, 1.000000000000000000),
 ( 1.000000000000000000, 0.9238795325112869605, 1.000000000000000000, 0.9238795325112869605, 1.000000000000000000, 0.9238795325112869605, 1.000000000000000000, 0.9238795325112869605, 1.000000000000000000, 0.9238795325112869605, 1.000000000000000000, 0.9238795325112869605, 1.000000000000000000, 0.9238795325112869605, 1.000000000000000000, 0.9238795325112869605, 1.000000000000000000, 0.9238795325112869605, 1.000000000000000000, 0.9238795325112869605, 1.000000000000000000, 0.9238795325112869605, 1.000000000000000000, 0.9238795325112869605, 1.000000000000000000, 0.9238795325112869605, 1.000000000000000000, 0.9238795325112869605, 1.000000000000000000, 0.9238795325112869605, 1.000000000000000000, 0.9238795325112869605, 1.000000000000000000, 0.9238795325112869605, 1.000000000000000000, 0.9238795325112869605, 1.000000000000000000, 0.9238795325112869605, 1.000000000000000000, 0.9238795325112869605, 1.000000000000000000, 0.9238795325112869605, 1.000000000000000000, 0.9238795325112869605, 1.000000000000000000, 0.9238795325112869605, 1.000000000000000000, 0.9238795325112869605, 1.000000000000000000, 0.9238795325112869605, 1.000000000000000000, 0.9238795325112869605, 1.000000000000000000, 0.9238795325112869605, 1.000000000000000000, 0.9238795325112869605, 1.000000000000000000, 0.9238795325112869605, 1.000000000000000000, 0.9238795325112869605, 1.000000000000000000, 0.9238795325112869605, 1.000000000000000000, 0.9238795325112869605, 1.000000000000000000, 0.9238795325112869605, 1.000000000000000000, 0.9238795325112869605, 1.000000000000000000, 0.9238795325112869605, 1.000000000000000000, 0.9238795325112869605, 1.000000000000000000, 0.9238795325112869605, 1.000000000000000000, 0.9238795325112869605, 1.000000000000000000, 0.9238795325112869605, 1.000000000000000000, 0.9238795325112869605, 1.000000000000000000, 0.9238795325112869605, 1.000000000000000000, 0.9238795325112869605, 1.000000000000000000, 0.9238795325112869605, 1.000000000000000000, 0.9238795325112869605, 1.000000000000000000, 0.9238795325112869605, 1.000000000000000000, 0.9238795325112869605, 1.000000000000000000, 0.9238795325112869605, 1.000000000000000000, 0.9238795325112869605, 1.000000000000000000, 0.9238795325112869605, 1.000000000000000000, 0.9238795325112869605, 1.000000000000000000, 0.9238795325112869605, 1.000000000000000000, 0.9238795325112869605, 1.000000000000000000, 0.9238795325112869605, 1.000000000000000000, 0.9238795325112869605, 1.000000000000000000, 0.9238795325112869605, 1.000000000000000000, 0.9238795325112869605, 1.000000000000000000, 0.9238795325112869605, 1.000000000000000000, 0.9238795325112869605, 1.000000000000000000, 0.9238795325112869605, 1.000000000000000000, 0.9238795325112869605, 1.000000000000000000, 0.9238795325112869605, 1.000000000000000000, 0.9238795325112869605, 1.000000000000000000, 0.9238795325112869605, 1.000000000000000000, 0.9238795325112869605, 1.000000000000000000, 0.9238795325112869605, 1.000000000000000000, 0.9238795325112869605, 1.000000000000000000, 0.9238795325112869605, 1.000000000000000000, 0.9238795325112869605, 1.000000000000000000, 0.9238795325112869605, 1.000000000000000000, 0.9238795325112869605, 1.000000000000000000, 0.9238795325112869605, 1.000000000000000000, 0.9238795325112869605, 1.000000000000000000, 0.9238795325112869605, 1.000000000000000000, 0.9238795325112869605, 1.000000000000000000, 0.9238795325112869605, 1.000000000000000000, 0.9238795325112869605, 1.000000000000000000, 0.9238795325112869605, 1.000000000000000000, 0.9238795325112869605, 1.000000000000000000, 0.9238795325112869605, 1.000000000000000000, 0.9238795325112869605, 1.000000000000000000, 0.9238795325112869605, 1.000000000000000000, 0.9238795325112869605, 1.000000000000000000, 0.9238795325112869605, 1.000000000000000000, 0.9238795325112869605, 1.000000000000000000, 0.9238795325112869605, 1.000000000000000000, 0.9238795325112869605, 1.000000000000000000, 0.9238795325112869605, 1.000000000000000000, 0.9238795325112869605, 1.000000000000000000, 0.9238795325112869605, 1.000000000000000000, 0.9238795325112869605, 1.000000000000000000, 0.9238795325112869605, 1.000000000000000000, 0.9238795325112869605, 1.000000000000000000, 0.9238795325112869605, 1.000000000000000000, 0.9238795325112869605, 1.000000000000000000, 0.9238795325112869605, 1.000000000000000000, 0.9238795325112869605, 1.000000000000000000, 0.9238795325112869605, 1.000000000000000000, 0.9238795325112869605, 1.000000000000000000, 0.9238795325112869605, 1.000000000000000000, 0.9238795325112869605, 1.000000000000000000, 0.9238795325112869605, 1.000000000000000000, 0.9238795325112869605, 1.000000000000000000, 0.9238795325112869605, 1.000000000000000000, 0.9238795325112869605, 1.000000000000000000, 0.9238795325112869605, 1.000000000000000000, 0.9238795325112869605, 1.000000000000000000, 0.9238795325112869605, 1.000000000000000000, 0.9238795325112869605, 1.000000000000000000, 0.9238795325112869605, 1.000000000000000000, 0.9238795325112869605, 1.000000000000000000, 0.9238795325112869605, 1.000000000000000000, 0.9238795325112869605, 1.000000000000000000, 0.9238795325112869605, 1.000000000000000000, 0.9238795325112869605, 1.000000000000000000, 0.9238795325112869605, 1.000000000000000000, 0.9238795325112869605, 1.000000000000000000, 0.9238795325112869605, 1.000000000000000000, 0.9238795325112869605, 1.000000000000000000, 0.9238795325112869605, 1.000000000000000000, 0.9238795325112869605, 1.000000000000000000, 0.9238795325112869605, 1.000000000000000000, 0.9238795325112869605, 1.000000000000000000, 0.9238795325112869605, 1.000000000000000000, 0.9238795325112869605, 1.000000000000000000, 0.9238795325112869605, 1.000000000000000000, 0.9238795325112869605, 1.000000000000000000, 0.9238795325112869605, 1.000000000000000000, 0.9238795325112869605, 1.000000000000000000) ) ) 
 REPRESENTATION_ITEM ( '' )  SURFACE ( )  );
#44561 = ADVANCED_FACE ( 'NONE', ( #35622 ), #14218, .T. ) ;
#44562 = EDGE_CURVE ( 'NONE', #25646, #7972, #29747, .T. ) ;
#44563 = CARTESIAN_POINT ( 'NONE',  ( 123.7445081442452874, -1.561330072975668948, -17.79121239304076951 ) ) ;
#44564 = CARTESIAN_POINT ( 'NONE',  ( 115.0086014775786509, -5.574606645277164318, -18.38911715685844683 ) ) ;
#44565 = CARTESIAN_POINT ( 'NONE',  ( 125.6164881442453094, 0.2603800115204892296, -16.42320221600525088 ) ) ;
#44566 = DIRECTION ( 'NONE',  ( 1.000000000000000000, 0.000000000000000000, 0.000000000000000000 ) ) ;
#44567 = CARTESIAN_POINT ( 'NONE',  ( 122.4521266859119635, -9.033780868592240054, -16.85052413769862056 ) ) ;
#44568 = ORIENTED_EDGE ( 'NONE', *, *, #33629, .F. ) ;
#44569 = ADVANCED_FACE ( 'NONE', ( #7144 ), #17863, .T. ) ;
#44570 = CARTESIAN_POINT ( 'NONE',  ( 111.2646414775786496, -8.899110576539710493, -16.42337572283490132 ) ) ;
#44571 = CARTESIAN_POINT ( 'NONE',  ( 125.3296504289692876, 1.783059037167336491, -10.84170924441004402 ) ) ;
#44572 = CARTESIAN_POINT ( 'NONE',  ( 116.1082702545247827, -10.62599879583958717, -15.77991374673208469 ) ) ;
#44573 = CARTESIAN_POINT ( 'NONE',  ( 89.78938736644981589, -25.23119213852205789, -15.24166438581092109 ) ) ;
#44574 = EDGE_CURVE ( 'NONE', #14664, #40056, #354, .T. ) ;
#44575 = CARTESIAN_POINT ( 'NONE',  ( 121.2485348109119769, -8.899110576539710493, -16.42337572283490132 ) ) ;
#44576 = CARTESIAN_POINT ( 'NONE',  ( 115.3489614775786407, -0.8288870151387760510, -10.36305467784173118 ) ) ;
#44577 = CARTESIAN_POINT ( 'NONE',  ( 126.3999550322131284, -0.5085153482442246187, -10.75768242470931213 ) ) ;
#44578 = EDGE_CURVE ( 'NONE', #35636, #42996, #12149, .T. ) ;
#44579 = EDGE_CURVE ( 'NONE', #32876, #36279, #29247, .T. ) ;
#44580 = ORIENTED_EDGE ( 'NONE', *, *, #41842, .F. ) ;
#44581 = LINE ( 'NONE', #23371, #35284 ) ;
#44582 = CARTESIAN_POINT ( 'NONE',  ( 112.6828081442453282, -2.084020599724406786, -8.691656652584148546 ) ) ;
#44584 = AXIS2_PLACEMENT_3D ( 'NONE', #13, #7078, #41530 ) ;
#44583 = CARTESIAN_POINT ( 'NONE',  ( 111.6379010812576809, -0.01829820670803256055, -12.14321520033831625 ) ) ;
#44585 = CARTESIAN_POINT ( 'NONE',  ( 71.37572422742091760, -11.86958442233774313, -21.39321520033831447 ) ) ;
#44587 = CARTESIAN_POINT ( 'NONE',  ( 126.2404814775786264, -9.261995988541697145, -16.69588392320189030 ) ) ;
#44586 = DIRECTION ( 'NONE',  ( -0.9063289528979890930, -0.4225728684367167087, 0.000000000000000000 ) ) ;
#44588 = CARTESIAN_POINT ( 'NONE',  ( 113.1933481442453058, -4.089484607189486809, -7.948022111789456723 ) ) ;
#44589 = ORIENTED_EDGE ( 'NONE', *, *, #26167, .T. ) ;
#44590 = CARTESIAN_POINT ( 'NONE',  ( 113.4202548109119846, -10.30919188438810075, -12.61870101168855918 ) ) ;
#44591 = CARTESIAN_POINT ( 'NONE',  ( 126.4852516627934023, 0.09531265143840929321, -14.71874934724275974 ) ) ;
#44592 = CARTESIAN_POINT ( 'NONE',  ( 115.8999108795247821, -8.938348069036489818, -9.318865927141430916 ) ) ;
#44593 = CARTESIAN_POINT ( 'NONE',  ( 125.2194014775786286, 0.1319031606808879209, -14.10382304977623669 ) ) ;
#44594 = CARTESIAN_POINT ( 'NONE',  ( 122.5532481442453019, 0.4262465694468514643, -12.03445270309931736 ) ) ;
#44595 = DIRECTION ( 'NONE',  ( 0.000000000000000000, 0.000000000000000000, 1.000000000000000000 ) ) ;
#44596 = CARTESIAN_POINT ( 'NONE',  ( 105.5513952545248060, 0.8980012041604421569, -11.00651665394454071 ) ) ;
#44597 = AXIS2_PLACEMENT_3D ( 'NONE', #35526, #27600, #41514 ) ;
#44598 = CARTESIAN_POINT ( 'NONE',  ( 117.1642148109119859, -9.261995988541702474, -16.69588392320188319 ) ) ;
#44599 = DIRECTION ( 'NONE',  ( 0.000000000000000000, 0.000000000000000000, -1.000000000000000000 ) ) ;
#44600 = CARTESIAN_POINT ( 'NONE',  ( 112.4559014775786778, -0.1624402480850797581, -16.17319339645315424 ) ) ;
#44601 = CARTESIAN_POINT ( 'NONE',  ( 108.5378796295247810, -4.863998795839590272, -19.15521520033831493 ) ) ;
#44602 = FACE_OUTER_BOUND ( 'NONE', #41361, .T. ) ;
#44603 = CARTESIAN_POINT ( 'NONE',  ( 111.8021765045248372, -7.250697342233347165, -19.15521520033831138 ) ) ;
#44604 = CARTESIAN_POINT ( 'NONE',  ( 125.0492214775786266, -6.344957434206665248, -7.627207830600338134 ) ) ;
#44605 = CARTESIAN_POINT ( 'NONE',  ( 123.0070614775786169, 0.9020085738987339008, -11.91225656197089222 ) ) ;
#44606 = CARTESIAN_POINT ( 'NONE',  ( 115.2053796295247849, -4.863998795839590272, -19.15521520033831493 ) ) ;
#44607 = CARTESIAN_POINT ( 'NONE',  ( 120.3409081442453044, -0.4660016031367893996, -10.09054647747474043 ) ) ;
#44608 = CARTESIAN_POINT ( 'NONE',  ( 111.8886348109120092, -3.383040157471821630, -19.15922257007629170 ) ) ;
#44609 = ORIENTED_EDGE ( 'NONE', *, *, #31852, .T. ) ;
#44610 = CARTESIAN_POINT ( 'NONE',  ( 112.3991748109119868, -1.833838273342658809, -17.42832698103878286 ) ) ;
#44611 = CARTESIAN_POINT ( 'NONE',  ( 112.5126281442453120, 0.1319031606808879209, -14.10382304977623669 ) ) ;
#44612 = CARTESIAN_POINT ( 'NONE',  ( 124.0281414775786146, -1.834011780172310813, -8.268836392978581529 ) ) ;
#44613 = CARTESIAN_POINT ( 'NONE',  ( 114.6115148109119986, -3.383040157471821630, -19.15922257007629170 ) ) ;
#44614 = PRODUCT_CONTEXT ( 'NONE', #30024, 'mechanical' ) ;
#44615 = CARTESIAN_POINT ( 'NONE',  ( 111.7184548109119788, -0.8288870151387760510, -10.36305467784173118 ) ) ;
#44616 = ORIENTED_EDGE ( 'NONE', *, *, #10407, .F. ) ;
#44617 = CARTESIAN_POINT ( 'NONE',  ( 116.8805814775786445, -3.505236298600246325, -18.68346056562440793 ) ) ;
#44618 = CARTESIAN_POINT ( 'NONE',  ( 113.0798948109119948, -0.4660016031367893996, -10.09054647747474043 ) ) ;
#44619 = CIRCLE ( 'NONE', #8931, 2.000000000000000444 ) ;
#44620 = CARTESIAN_POINT ( 'NONE',  ( 124.7655881442452852, -9.859900752359378018, -12.68260735090039759 ) ) ;
#44621 = CARTESIAN_POINT ( 'NONE',  ( 116.8413970861548705, -0.9790246463113243536, -16.91993411223075583 ) ) ;
#44622 = CARTESIAN_POINT ( 'NONE',  ( 113.1912390045248031, 0.8980012041604421569, -15.77991374673208469 ) ) ;
#44623 = ORIENTED_EDGE ( 'NONE', *, *, #17533, .F. ) ;
#44624 = AXIS2_PLACEMENT_3D ( 'NONE', #39828, #18412, #43024 ) ;
#44625 = DIRECTION ( 'NONE',  ( -0.7071067811865480168, -0.5654279342907823080, -0.4246071727180995570 ) ) ;
#44626 = CARTESIAN_POINT ( 'NONE',  ( 113.1743144685027858, 0.6938714319018670640, -14.64321520033829316 ) ) ;
#44627 = ADVANCED_FACE ( 'NONE', ( #43155 ), #16488, .T. ) ;
#44628 = CARTESIAN_POINT ( 'NONE',  ( 119.7434548109119703, -6.339884145921025116, -18.90789653539788517 ) ) ;
#44629 = VECTOR ( 'NONE', #12084, 1000.000000000000227 ) ;
#44630 = CARTESIAN_POINT ( 'NONE',  ( 112.7962614775786676, -3.383040157471821630, -19.15922257007629170 ) ) ;
#44631 = CARTESIAN_POINT ( 'NONE',  ( 116.8076447119520083, 1.993636652035369217, -5.877315907535680672 ) ) ;
#44632 = CARTESIAN_POINT ( 'NONE',  ( 121.3655035264548872, -8.247323210606168686, -17.08054893949881148 ) ) ;
#44633 = CARTESIAN_POINT ( 'NONE',  ( 106.1764733795248219, -1.325403438956436419, -9.854619843455211026 ) ) ;
#44634 = CARTESIAN_POINT ( 'NONE',  ( 111.4548954522301898, 0.1168444861212661334, -14.64321520033828783 ) ) ;
#44635 = CARTESIAN_POINT ( 'NONE',  ( 117.6180281442453150, -0.4660016031367893996, -10.09054647747474043 ) ) ;
#44636 = DIRECTION ( 'NONE',  ( 1.000000000000000000, 0.000000000000000000, -0.000000000000000000 ) ) ;
#44637 = CARTESIAN_POINT ( 'NONE',  ( 115.6662166496844861, 0.5600166689815611054, -12.14321520033831625 ) ) ;
#44638 = CARTESIAN_POINT ( 'NONE',  ( 124.1916298109119765, -2.529232162391345184, -8.971805383623923547 ) ) ;
#44639 =( BOUNDED_SURFACE ( )  B_SPLINE_SURFACE ( 1, 2, ( 
 ( #40023, #26348, #23614, #3733, #44814, #17219, #20418, #6274, #7158, #31327, #9932, #20194, #6950, #13572, #20855, #30669, #44362, #13353, #14014, #101, #34078, #27482, #41401, #10156, #37732, #24501, #21069, #34948, #23845, #24065, #44590, #41838, #13793, #37500, #37956, #30443, #27706, #6731, #2845, #16775, #10598, #27257, #41172, #13124, #20641, #6502, #34518, #31109, #3296, #45034, #27929, #34301, #27029, #3516, #41620, #40944, #17003, #9700, #3074, #30892, #10376, #24285, #38171, #38385, #34733, #17433, #32445, #7607, #15133, #42730, #11040, #1219, #11266, #28149, #25400, #21521, #24713, #10817, #17656, #4183, #14233, #42059, #8068, #29039, #42948, #28364, #35858, #28595, #35408, #11714, #25625, #7841, #35179, #38603, #42278, #28820, #22193, #35638, #24942, #7379, #3956, #39530, #4632, #8291, #21747, #32221, #11495, #18553, #36089, #25174, #31552, #39298, #42506, #31775, #994, #21296, #39072, #38838, #18101, #320, #4414, #17878, #21971, #31996, #546, #14458, #759, #14681, #18328, #14909, #40432, #2334, #16264, #15580, #23100, #15806, #22642, #30167, #44084, #40201, #22418, #29263, #29484, #16032, #9412, #22866, #12165, #15358, #36311, #12849, #36980, #40658, #8967, #19447, #43853, #5749, #26750, #12394, #23323, #26523, #29707, #18997, #33330, #25839, #43620, #43397, #19669, #26294, #9193, #11943, #1658, #29940, #32884, #33557, #4860, #18778, #2104, #12625, #43175, #32668, #19228, #36759, #39971, #39747, #1436, #8515, #26067, #5081, #8734, #33109, #36538, #5312, #1879, #5528, #20804, #6894, #40890, #6455, #3023, #16945, #44533, #31275, #13962, #41787, #30616, #30839, #6218, #3471, #20586, #30392, #44762, #27873, #34464, #13521, #44314, #9643, #17386, #23565, #20141, #10544, #27430, #34026, #34250, #37900, #41352, #10108, #34683, #37446, #37209, #10327, #3243, #5981, #23790, #19906, #33791, #2794, #2563, #13295, #16492, #48, #6678, #26969, #13070, #27203, #16721, #17169, #41121, #9880, #31058, #37680, #20363, #24012, #44986, #13745, #27653, #41568, #24230 ),
 ( #38121, #8006, #25121, #28546, #38551, #939, #42673, #42897, #708, #7327, #21246, #35808, #14858, #28767, #28314, #11443, #25348, #39017, #269, #32170, #1162, #21915, #38784, #14628, #24444, #10768, #7555, #21470, #42450, #35353, #15078, #24664, #28990, #18274, #39242, #4578, #38335, #14404, #18503, #7112, #14178, #4129, #42226, #32393, #18049, #7787, #35123, #21022, #21696, #34895, #31942, #11216, #35582, #3684, #17605, #3906, #31721, #31498, #4354, #28096, #42004, #10989, #24891, #17824, #491, #43969, #22143, #12733, #2222, #34138, #36035, #2676, #8236, #1383, #30277, #12964, #26860, #19793, #26635, #18725, #33442, #16375, #22985, #44202, #33677, #4804, #11659, #6335, #9766, #16151, #23677, #11886, #25566, #37096, #30729, #32617, #37566, #37333, #40773, #15298, #29207, #39472, #43116, #26409, #40548, #40319, #2453, #16837, #13188, #9083, #9309, #36874, #23217, #30056, #2907, #5644, #16608, #19565, #5871, #9532, #23447, #6104, #20024, #33906, #30501, #44421, #27090, #41012, #20252, #20919, #37787, #44653, #38669, #42120, #3362, #10880, #44877, #13415, #24344, #17939, #6560, #24777, #24562, #14073, #20478, #41235, #27319, #34358, #9995, #27764, #23904, #7010, #4017, #383, #3139, #17061, #30954, #157, #14294, #17281, #31172, #10214, #13633, #35007, #38016, #34579, #17489, #3577, #27544, #38448, #7436, #34794, #41456, #3789, #28212, #27990, #31387, #24123, #21131, #17715, #6792, #41895, #20700, #45093, #21357, #31613, #35240, #13849, #41679, #10438, #10656, #38228, #7219, #8577, #15418, #1052, #8132, #5143, #18162, #14968, #28880, #22033, #42792, #22478, #32058, #36372, #25683, #1496, #29323, #607, #21806, #12002, #31838, #7668, #11553, #35699, #43237, #25461, #1279, #14746, #25905, #29095, #8351, #39364, #4694, #35928, #14518, #28430, #28658, #39132, #38898, #18614, #32505, #15191, #4475, #32288, #4917, #42344, #22255, #43006, #826, #11776, #21583, #39590, #11325, #18832, #36149, #32724, #35470, #42563, #39811, #25235, #11102, #25005, #4245, #7899, #18395 ) ),
 .UNSPECIFIED., .F., .F., .F. ) 
 B_SPLINE_SURFACE_WITH_KNOTS ( ( 2, 2 ),
 ( 3, 2, 2, 2, 2, 2, 2, 2, 2, 2, 2, 2, 2, 2, 2, 2, 2, 2, 2, 2, 2, 2, 2, 2, 2, 2, 2, 2, 2, 2, 2, 2, 2, 2, 2, 2, 2, 2, 2, 2, 2, 2, 2, 2, 2, 2, 2, 2, 2, 2, 2, 2, 2, 2, 2, 2, 2, 2, 2, 2, 2, 2, 2, 2, 2, 2, 2, 2, 2, 2, 2, 2, 2, 2, 2, 2, 2, 2, 2, 2, 2, 2, 2, 2, 2, 2, 2, 2, 2, 2, 2, 2, 2, 2, 2, 2, 2, 2, 2, 2, 2, 2, 2, 2, 2, 2, 2, 2, 2, 2, 2, 2, 2, 2, 2, 2, 2, 2, 2, 2, 2, 2, 2, 2, 2, 2, 2, 2, 3 ),
 ( 0.000000000000000000, 1.000000000000000000 ),
 ( 0.000000000000000000, 0.007812500000000000000, 0.01562500000000000000, 0.02343750000000000000, 0.03125000000000000000, 0.03906250000000000000, 0.04687500000000000000, 0.05468750000000000000, 0.06250000000000000000, 0.07031250000000000000, 0.07812500000000000000, 0.08593750000000000000, 0.09375000000000000000, 0.1015625000000000000, 0.1093750000000000000, 0.1171875000000000000, 0.1250000000000000000, 0.1328125000000000000, 0.1406250000000000000, 0.1484375000000000000, 0.1562500000000000000, 0.1640625000000000000, 0.1718750000000000000, 0.1796875000000000000, 0.1875000000000000000, 0.1953125000000000000, 0.2031250000000000000, 0.2109375000000000000, 0.2187500000000000000, 0.2265625000000000000, 0.2343750000000000000, 0.2421875000000000000, 0.2500000000000000000, 0.2578125000000000000, 0.2656250000000000000, 0.2734375000000000000, 0.2812500000000000000, 0.2890625000000000000, 0.2968750000000000000, 0.3046875000000000000, 0.3125000000000000000, 0.3203125000000000000, 0.3281250000000000000, 0.3359375000000000000, 0.3437500000000000000, 0.3515625000000000000, 0.3593750000000000000, 0.3671875000000000000, 0.3750000000000000000, 0.3828125000000000000, 0.3906250000000000000, 0.3984375000000000000, 0.4062500000000000000, 0.4140625000000000000, 0.4218750000000000000, 0.4296875000000000000, 0.4375000000000000000, 0.4453125000000000000, 0.4531250000000000000, 0.4609375000000000000, 0.4687500000000000000, 0.4765625000000000000, 0.4843750000000000000, 0.4921875000000000000, 0.5000000000000000000, 0.5078125000000000000, 0.5156250000000000000, 0.5234375000000000000, 0.5312500000000000000, 0.5390625000000000000, 0.5468750000000000000, 0.5546875000000000000, 0.5625000000000000000, 0.5703125000000000000, 0.5781250000000000000, 0.5859375000000000000, 0.5937500000000000000, 0.6015625000000000000, 0.6093750000000000000, 0.6171875000000000000, 0.6250000000000000000, 0.6328125000000000000, 0.6406250000000000000, 0.6484375000000000000, 0.6562500000000000000, 0.6640625000000000000, 0.6718750000000000000, 0.6796875000000000000, 0.6875000000000000000, 0.6953125000000000000, 0.7031250000000000000, 0.7109375000000000000, 0.7187500000000000000, 0.7265625000000000000, 0.7343750000000000000, 0.7421875000000000000, 0.7500000000000000000, 0.7578125000000000000, 0.7656250000000000000, 0.7734375000000000000, 0.7812500000000000000, 0.7890625000000000000, 0.7968750000000000000, 0.8046875000000000000, 0.8125000000000000000, 0.8203125000000000000, 0.8281250000000000000, 0.8359375000000000000, 0.8437500000000000000, 0.8515625000000000000, 0.8593750000000000000, 0.8671875000000000000, 0.8750000000000000000, 0.8828125000000000000, 0.8906250000000000000, 0.8984375000000000000, 0.9062500000000000000, 0.9140625000000000000, 0.9218750000000000000, 0.9296875000000000000, 0.9375000000000000000, 0.9453125000000000000, 0.9531250000000000000, 0.9609375000000000000, 0.9687500000000000000, 0.9765625000000000000, 0.9843750000000000000, 0.9921875000000000000, 1.000000000000000000 ),
 .UNSPECIFIED. ) 
 GEOMETRIC_REPRESENTATION_ITEM ( )  RATIONAL_B_SPLINE_SURFACE ( (
 ( 1.000000000000000000, 0.9238795325112869605, 1.000000000000000000, 0.9238795325112869605, 1.000000000000000000, 0.9238795325112869605, 1.000000000000000000, 0.9238795325112869605, 1.000000000000000000, 0.9238795325112869605, 1.000000000000000000, 0.9238795325112869605, 1.000000000000000000, 0.9238795325112869605, 1.000000000000000000, 0.9238795325112869605, 1.000000000000000000, 0.9238795325112869605, 1.000000000000000000, 0.9238795325112869605, 1.000000000000000000, 0.9238795325112869605, 1.000000000000000000, 0.9238795325112869605, 1.000000000000000000, 0.9238795325112869605, 1.000000000000000000, 0.9238795325112869605, 1.000000000000000000, 0.9238795325112869605, 1.000000000000000000, 0.9238795325112869605, 1.000000000000000000, 0.9238795325112869605, 1.000000000000000000, 0.9238795325112869605, 1.000000000000000000, 0.9238795325112869605, 1.000000000000000000, 0.9238795325112869605, 1.000000000000000000, 0.9238795325112869605, 1.000000000000000000, 0.9238795325112869605, 1.000000000000000000, 0.9238795325112869605, 1.000000000000000000, 0.9238795325112869605, 1.000000000000000000, 0.9238795325112869605, 1.000000000000000000, 0.9238795325112869605, 1.000000000000000000, 0.9238795325112869605, 1.000000000000000000, 0.9238795325112869605, 1.000000000000000000, 0.9238795325112869605, 1.000000000000000000, 0.9238795325112869605, 1.000000000000000000, 0.9238795325112869605, 1.000000000000000000, 0.9238795325112869605, 1.000000000000000000, 0.9238795325112869605, 1.000000000000000000, 0.9238795325112869605, 1.000000000000000000, 0.9238795325112869605, 1.000000000000000000, 0.9238795325112869605, 1.000000000000000000, 0.9238795325112869605, 1.000000000000000000, 0.9238795325112869605, 1.000000000000000000, 0.9238795325112869605, 1.000000000000000000, 0.9238795325112869605, 1.000000000000000000, 0.9238795325112869605, 1.000000000000000000, 0.9238795325112869605, 1.000000000000000000, 0.9238795325112869605, 1.000000000000000000, 0.9238795325112869605, 1.000000000000000000, 0.9238795325112869605, 1.000000000000000000, 0.9238795325112869605, 1.000000000000000000, 0.9238795325112869605, 1.000000000000000000, 0.9238795325112869605, 1.000000000000000000, 0.9238795325112869605, 1.000000000000000000, 0.9238795325112869605, 1.000000000000000000, 0.9238795325112869605, 1.000000000000000000, 0.9238795325112869605, 1.000000000000000000, 0.9238795325112869605, 1.000000000000000000, 0.9238795325112869605, 1.000000000000000000, 0.9238795325112869605, 1.000000000000000000, 0.9238795325112869605, 1.000000000000000000, 0.9238795325112869605, 1.000000000000000000, 0.9238795325112869605, 1.000000000000000000, 0.9238795325112869605, 1.000000000000000000, 0.9238795325112869605, 1.000000000000000000, 0.9238795325112869605, 1.000000000000000000, 0.9238795325112869605, 1.000000000000000000, 0.9238795325112869605, 1.000000000000000000, 0.9238795325112869605, 1.000000000000000000, 0.9238795325112869605, 1.000000000000000000, 0.9238795325112869605, 1.000000000000000000, 0.9238795325112869605, 1.000000000000000000, 0.9238795325112869605, 1.000000000000000000, 0.9238795325112869605, 1.000000000000000000, 0.9238795325112869605, 1.000000000000000000, 0.9238795325112869605, 1.000000000000000000, 0.9238795325112869605, 1.000000000000000000, 0.9238795325112869605, 1.000000000000000000, 0.9238795325112869605, 1.000000000000000000, 0.9238795325112869605, 1.000000000000000000, 0.9238795325112869605, 1.000000000000000000, 0.9238795325112869605, 1.000000000000000000, 0.9238795325112869605, 1.000000000000000000, 0.9238795325112869605, 1.000000000000000000, 0.9238795325112869605, 1.000000000000000000, 0.9238795325112869605, 1.000000000000000000, 0.9238795325112869605, 1.000000000000000000, 0.9238795325112869605, 1.000000000000000000, 0.9238795325112869605, 1.000000000000000000, 0.9238795325112869605, 1.000000000000000000, 0.9238795325112869605, 1.000000000000000000, 0.9238795325112869605, 1.000000000000000000, 0.9238795325112869605, 1.000000000000000000, 0.9238795325112869605, 1.000000000000000000, 0.9238795325112869605, 1.000000000000000000, 0.9238795325112869605, 1.000000000000000000, 0.9238795325112869605, 1.000000000000000000, 0.9238795325112869605, 1.000000000000000000, 0.9238795325112869605, 1.000000000000000000, 0.9238795325112869605, 1.000000000000000000, 0.9238795325112869605, 1.000000000000000000, 0.9238795325112869605, 1.000000000000000000, 0.9238795325112869605, 1.000000000000000000, 0.9238795325112869605, 1.000000000000000000, 0.9238795325112869605, 1.000000000000000000, 0.9238795325112869605, 1.000000000000000000, 0.9238795325112869605, 1.000000000000000000, 0.9238795325112869605, 1.000000000000000000, 0.9238795325112869605, 1.000000000000000000, 0.9238795325112869605, 1.000000000000000000, 0.9238795325112869605, 1.000000000000000000, 0.9238795325112869605, 1.000000000000000000, 0.9238795325112869605, 1.000000000000000000, 0.9238795325112869605, 1.000000000000000000, 0.9238795325112869605, 1.000000000000000000, 0.9238795325112869605, 1.000000000000000000, 0.9238795325112869605, 1.000000000000000000, 0.9238795325112869605, 1.000000000000000000, 0.9238795325112869605, 1.000000000000000000, 0.9238795325112869605, 1.000000000000000000, 0.9238795325112869605, 1.000000000000000000, 0.9238795325112869605, 1.000000000000000000, 0.9238795325112869605, 1.000000000000000000, 0.9238795325112869605, 1.000000000000000000, 0.9238795325112869605, 1.000000000000000000, 0.9238795325112869605, 1.000000000000000000, 0.9238795325112869605, 1.000000000000000000, 0.9238795325112869605, 1.000000000000000000, 0.9238795325112869605, 1.000000000000000000, 0.9238795325112869605, 1.000000000000000000, 0.9238795325112869605, 1.000000000000000000, 0.9238795325112869605, 1.000000000000000000, 0.9238795325112869605, 1.000000000000000000),
 ( 1.000000000000000000, 0.9238795325112869605, 1.000000000000000000, 0.9238795325112869605, 1.000000000000000000, 0.9238795325112869605, 1.000000000000000000, 0.9238795325112869605, 1.000000000000000000, 0.9238795325112869605, 1.000000000000000000, 0.9238795325112869605, 1.000000000000000000, 0.9238795325112869605, 1.000000000000000000, 0.9238795325112869605, 1.000000000000000000, 0.9238795325112869605, 1.000000000000000000, 0.9238795325112869605, 1.000000000000000000, 0.9238795325112869605, 1.000000000000000000, 0.9238795325112869605, 1.000000000000000000, 0.9238795325112869605, 1.000000000000000000, 0.9238795325112869605, 1.000000000000000000, 0.9238795325112869605, 1.000000000000000000, 0.9238795325112869605, 1.000000000000000000, 0.9238795325112869605, 1.000000000000000000, 0.9238795325112869605, 1.000000000000000000, 0.9238795325112869605, 1.000000000000000000, 0.9238795325112869605, 1.000000000000000000, 0.9238795325112869605, 1.000000000000000000, 0.9238795325112869605, 1.000000000000000000, 0.9238795325112869605, 1.000000000000000000, 0.9238795325112869605, 1.000000000000000000, 0.9238795325112869605, 1.000000000000000000, 0.9238795325112869605, 1.000000000000000000, 0.9238795325112869605, 1.000000000000000000, 0.9238795325112869605, 1.000000000000000000, 0.9238795325112869605, 1.000000000000000000, 0.9238795325112869605, 1.000000000000000000, 0.9238795325112869605, 1.000000000000000000, 0.9238795325112869605, 1.000000000000000000, 0.9238795325112869605, 1.000000000000000000, 0.9238795325112869605, 1.000000000000000000, 0.9238795325112869605, 1.000000000000000000, 0.9238795325112869605, 1.000000000000000000, 0.9238795325112869605, 1.000000000000000000, 0.9238795325112869605, 1.000000000000000000, 0.9238795325112869605, 1.000000000000000000, 0.9238795325112869605, 1.000000000000000000, 0.9238795325112869605, 1.000000000000000000, 0.9238795325112869605, 1.000000000000000000, 0.9238795325112869605, 1.000000000000000000, 0.9238795325112869605, 1.000000000000000000, 0.9238795325112869605, 1.000000000000000000, 0.9238795325112869605, 1.000000000000000000, 0.9238795325112869605, 1.000000000000000000, 0.9238795325112869605, 1.000000000000000000, 0.9238795325112869605, 1.000000000000000000, 0.9238795325112869605, 1.000000000000000000, 0.9238795325112869605, 1.000000000000000000, 0.9238795325112869605, 1.000000000000000000, 0.9238795325112869605, 1.000000000000000000, 0.9238795325112869605, 1.000000000000000000, 0.9238795325112869605, 1.000000000000000000, 0.9238795325112869605, 1.000000000000000000, 0.9238795325112869605, 1.000000000000000000, 0.9238795325112869605, 1.000000000000000000, 0.9238795325112869605, 1.000000000000000000, 0.9238795325112869605, 1.000000000000000000, 0.9238795325112869605, 1.000000000000000000, 0.9238795325112869605, 1.000000000000000000, 0.9238795325112869605, 1.000000000000000000, 0.9238795325112869605, 1.000000000000000000, 0.9238795325112869605, 1.000000000000000000, 0.9238795325112869605, 1.000000000000000000, 0.9238795325112869605, 1.000000000000000000, 0.9238795325112869605, 1.000000000000000000, 0.9238795325112869605, 1.000000000000000000, 0.9238795325112869605, 1.000000000000000000, 0.9238795325112869605, 1.000000000000000000, 0.9238795325112869605, 1.000000000000000000, 0.9238795325112869605, 1.000000000000000000, 0.9238795325112869605, 1.000000000000000000, 0.9238795325112869605, 1.000000000000000000, 0.9238795325112869605, 1.000000000000000000, 0.9238795325112869605, 1.000000000000000000, 0.9238795325112869605, 1.000000000000000000, 0.9238795325112869605, 1.000000000000000000, 0.9238795325112869605, 1.000000000000000000, 0.9238795325112869605, 1.000000000000000000, 0.9238795325112869605, 1.000000000000000000, 0.9238795325112869605, 1.000000000000000000, 0.9238795325112869605, 1.000000000000000000, 0.9238795325112869605, 1.000000000000000000, 0.9238795325112869605, 1.000000000000000000, 0.9238795325112869605, 1.000000000000000000, 0.9238795325112869605, 1.000000000000000000, 0.9238795325112869605, 1.000000000000000000, 0.9238795325112869605, 1.000000000000000000, 0.9238795325112869605, 1.000000000000000000, 0.9238795325112869605, 1.000000000000000000, 0.9238795325112869605, 1.000000000000000000, 0.9238795325112869605, 1.000000000000000000, 0.9238795325112869605, 1.000000000000000000, 0.9238795325112869605, 1.000000000000000000, 0.9238795325112869605, 1.000000000000000000, 0.9238795325112869605, 1.000000000000000000, 0.9238795325112869605, 1.000000000000000000, 0.9238795325112869605, 1.000000000000000000, 0.9238795325112869605, 1.000000000000000000, 0.9238795325112869605, 1.000000000000000000, 0.9238795325112869605, 1.000000000000000000, 0.9238795325112869605, 1.000000000000000000, 0.9238795325112869605, 1.000000000000000000, 0.9238795325112869605, 1.000000000000000000, 0.9238795325112869605, 1.000000000000000000, 0.9238795325112869605, 1.000000000000000000, 0.9238795325112869605, 1.000000000000000000, 0.9238795325112869605, 1.000000000000000000, 0.9238795325112869605, 1.000000000000000000, 0.9238795325112869605, 1.000000000000000000, 0.9238795325112869605, 1.000000000000000000, 0.9238795325112869605, 1.000000000000000000, 0.9238795325112869605, 1.000000000000000000, 0.9238795325112869605, 1.000000000000000000, 0.9238795325112869605, 1.000000000000000000, 0.9238795325112869605, 1.000000000000000000, 0.9238795325112869605, 1.000000000000000000, 0.9238795325112869605, 1.000000000000000000, 0.9238795325112869605, 1.000000000000000000, 0.9238795325112869605, 1.000000000000000000, 0.9238795325112869605, 1.000000000000000000, 0.9238795325112869605, 1.000000000000000000, 0.9238795325112869605, 1.000000000000000000, 0.9238795325112869605, 1.000000000000000000, 0.9238795325112869605, 1.000000000000000000, 0.9238795325112869605, 1.000000000000000000) ) ) 
 REPRESENTATION_ITEM ( '' )  SURFACE ( )  );
#44640 = CARTESIAN_POINT ( 'NONE',  ( 122.0427081442452817, -9.859900752359378018, -12.68260735090039759 ) ) ;
#44641 = ORIENTED_EDGE ( 'NONE', *, *, #23727, .F. ) ;
#44642 = DIRECTION ( 'NONE',  ( 0.000000000000000000, 0.000000000000000000, 1.000000000000000000 ) ) ;
#44643 = EDGE_CURVE ( 'NONE', #41318, #20631, #1477, .T. ) ;
#44644 = CARTESIAN_POINT ( 'NONE',  ( 121.1350814775786233, 0.5811942927096110934, -14.16772938898807510 ) ) ;
#44645 = CARTESIAN_POINT ( 'NONE',  ( 117.1500671295247713, 0.1403307496149613920, -13.39321520033831447 ) ) ;
#44646 = CARTESIAN_POINT ( 'NONE',  ( 116.7671281442453335, -7.643976991954077427, -18.09477374809248928 ) ) ;
#44647 = CARTESIAN_POINT ( 'NONE',  ( 125.2194014775786286, -10.30919188438810075, -12.61870101168855918 ) ) ;
#44648 = CARTESIAN_POINT ( 'NONE',  ( 109.6491296295247793, -4.863998795839590272, -19.15521520033831493 ) ) ;
#44649 = CARTESIAN_POINT ( 'NONE',  ( 95.28169473643895060, -25.99489077589524300, -13.39321520033831447 ) ) ;
#44650 = CARTESIAN_POINT ( 'NONE',  ( 115.8999108795247821, -8.938348069036489818, -9.318865927141430916 ) ) ;
#44651 = CARTESIAN_POINT ( 'NONE',  ( 116.9373081442452929, -1.833838273342659253, -17.42832698103878286 ) ) ;
#44652 = CIRCLE ( 'NONE', #20601, 2.000000000000000444 ) ;
#44653 = CARTESIAN_POINT ( 'NONE',  ( 118.6958348109119754, -3.505236298600246325, -18.68346056562440793 ) ) ;
#44654 = CARTESIAN_POINT ( 'NONE',  ( 136.0831615568885127, -1.935278198691274598, -18.54223449093250764 ) ) ;
#44655 = CARTESIAN_POINT ( 'NONE',  ( 109.6491296295247793, -4.863998795839590272, -8.388885654883775800 ) ) ;
#44656 = ORIENTED_EDGE ( 'NONE', *, *, #4213, .F. ) ;
#44657 = DIRECTION ( 'NONE',  ( 1.000000000000000000, 0.000000000000000000, 0.000000000000000000 ) ) ;
#44658 = CARTESIAN_POINT ( 'NONE',  ( 114.6682414775786469, -1.561330072975668060, -17.79121239304076596 ) ) ;
#44659 = CARTESIAN_POINT ( 'NONE',  ( 113.0686126669217799, -2.334846009198400019, -18.01015021110789149 ) ) ;
#44660 = CARTESIAN_POINT ( 'NONE',  ( 123.5633766859119760, -9.033780868592240054, -16.85052413769862056 ) ) ;
#44661 = CARTESIAN_POINT ( 'NONE',  ( 122.6604860609119640, -3.387241619883791355, -18.17469012370385073 ) ) ;
#44662 = VERTEX_POINT ( 'NONE', #14366 ) ;
#44663 = CARTESIAN_POINT ( 'NONE',  ( 93.24708369096698846, -23.96159667187537679, -12.55314669922780979 ) ) ;
#44664 = CARTESIAN_POINT ( 'NONE',  ( 104.9957702545248566, 0.1403307496149616695, -11.32035403202665336 ) ) ;
#44665 = ORIENTED_EDGE ( 'NONE', *, *, #17514, .T. ) ;
#44666 = AXIS2_PLACEMENT_3D ( 'NONE', #5786, #12199, #40692 ) ;
#44667 = CARTESIAN_POINT ( 'NONE',  ( 122.9503348109119827, 0.5811942927096110934, -14.16772938898807510 ) ) ;
#44668 = CARTESIAN_POINT ( 'NONE',  ( 114.2711548109119803, -9.988377603198976828, -10.36322818467138340 ) ) ;
#44669 = CARTESIAN_POINT ( 'NONE',  ( 117.3343948109119737, -6.222761293078241884, -8.102969835052219238 ) ) ;
#44670 = DIRECTION ( 'NONE',  ( -1.000000000000000000, 0.000000000000000000, -0.000000000000000000 ) ) ;
#44671 = CARTESIAN_POINT ( 'NONE',  ( 120.3409081442453044, -0.4660016031367893996, -10.09054647747474043 ) ) ;
#44672 = CARTESIAN_POINT ( 'NONE',  ( 117.5613014775786525, 0.9020085738987339008, -11.91225656197089222 ) ) ;
#44673 = CARTESIAN_POINT ( 'NONE',  ( 116.5249890045247980, 0.8980012041604421569, -15.77991374673208469 ) ) ;
#44674 = CARTESIAN_POINT ( 'NONE',  ( 113.0798948109119948, -8.899110576539710493, -16.42337572283490132 ) ) ;
#44675 = DIRECTION ( 'NONE',  ( 1.000000000000000000, 0.000000000000000000, 0.000000000000000000 ) ) ;
#44676 = ORIENTED_EDGE ( 'NONE', *, *, #14805, .F. ) ;
#44677 = CARTESIAN_POINT ( 'NONE',  ( 118.0151148109119816, -10.63000616557722466, -14.87417383870573495 ) ) ;
#44678 = EDGE_CURVE ( 'NONE', #18111, #33252, #21551, .T. ) ;
#44679 = CIRCLE ( 'NONE', #4586, 5.000000000000004441 ) ;
#44680 = CARTESIAN_POINT ( 'NONE',  ( 120.2296266859119953, -0.06289925094097943703, -9.412459353600674206 ) ) ;
#44681 = CARTESIAN_POINT ( 'NONE',  ( 114.8951481442453115, -0.4660016031367893996, -10.09054647747474043 ) ) ;
#44682 = VERTEX_POINT ( 'NONE', #38745 ) ;
#44683 = CIRCLE ( 'NONE', #22075, 8.800000000000000711 ) ;
#44684 = CARTESIAN_POINT ( 'NONE',  ( 120.2274548109119934, 0.5811942927096110934, -14.16772938898807510 ) ) ;
#44685 = DIRECTION ( 'NONE',  ( 0.000000000000000000, 0.000000000000000000, -1.000000000000000000 ) ) ;
#44686 = CARTESIAN_POINT ( 'NONE',  ( 112.2289948109119848, -7.643976991954077427, -18.09477374809248928 ) ) ;
#44687 = CARTESIAN_POINT ( 'NONE',  ( 125.0091119737025451, -1.196538596002817867, -17.02799684832028504 ) ) ;
#44688 = CARTESIAN_POINT ( 'NONE',  ( 114.7816948109119863, -9.859900752359374465, -12.68260735090039404 ) ) ;
#44689 = CARTESIAN_POINT ( 'NONE',  ( 111.3850766211417067, -8.962231996695310343, -16.26240453864375723 ) ) ;
#44690 = CARTESIAN_POINT ( 'NONE',  ( 116.6536748109119941, -10.15424416112533912, -14.75197769757731336 ) ) ;
#44691 = VECTOR ( 'NONE', #11126, 1000.000000000000000 ) ;
#44692 = EDGE_CURVE ( 'NONE', #2818, #44000, #37567, .T. ) ;
#44693 = DIRECTION ( 'NONE',  ( 0.000000000000000000, 0.4669533266896288004, 0.8842819633428518067 ) ) ;
#44694 = CARTESIAN_POINT ( 'NONE',  ( 116.0864081442453113, -0.1624402480850797581, -16.17319339645315424 ) ) ;
#44695 = CARTESIAN_POINT ( 'NONE',  ( 116.7104014775786425, -0.4660016031367893996, -10.09054647747474043 ) ) ;
#44696 = CARTESIAN_POINT ( 'NONE',  ( 121.2019704359119743, 1.345710702986147034, -13.97328579221134426 ) ) ;
#44697 = CARTESIAN_POINT ( 'NONE',  ( 115.9729548109119861, -6.344957434206662583, -7.627207830600332805 ) ) ;
#44698 = CARTESIAN_POINT ( 'NONE',  ( 113.7606148109119886, -7.894159318335828068, -9.358103419637847864 ) ) ;
#44699 = CARTESIAN_POINT ( 'NONE',  ( 112.1722681442453222, -8.899110576539710493, -16.42337572283490132 ) ) ;
#44700 = CARTESIAN_POINT ( 'NONE',  ( 115.7460481442453357, -10.15424416112533912, -14.75197769757731336 ) ) ;
#44701 = ORIENTED_EDGE ( 'NONE', *, *, #3333, .F. ) ;
#44702 = CARTESIAN_POINT ( 'NONE',  ( 114.7816948109119863, 0.5811942927096154232, -14.16772938898807155 ) ) ;
#44703 = CARTESIAN_POINT ( 'NONE',  ( 108.3989733795248753, -8.938348069036489818, -17.46756447353520159 ) ) ;
#44704 = CARTESIAN_POINT ( 'NONE',  ( 107.1488171295248861, 0.1403307496149613920, -13.39321520033831447 ) ) ;
#44705 = CARTESIAN_POINT ( 'NONE',  ( 105.9681140045248355, 0.1403307496149616695, -15.46607636864997204 ) ) ;
#44706 = FACE_OUTER_BOUND ( 'NONE', #33531, .T. ) ;
#44707 = CARTESIAN_POINT ( 'NONE',  ( 118.8092881442453290, -9.988377603198976828, -10.36322818467138340 ) ) ;
#44708 = ORIENTED_EDGE ( 'NONE', *, *, #6916, .T. ) ;
#44709 = CARTESIAN_POINT ( 'NONE',  ( 121.9470836909669913, -25.99489077589524300, -13.39321520033831447 ) ) ;
#44710 = CARTESIAN_POINT ( 'NONE',  ( 87.44708369096657918, -21.99489077589588604, -4.893215200338314474 ) ) ;
#44711 = CARTESIAN_POINT ( 'NONE',  ( 119.6034614775786196, -3.505236298600246325, -18.68346056562440793 ) ) ;
#44712 = CARTESIAN_POINT ( 'NONE',  ( 128.0511146350394256, 1.009132413410308571, -12.67876786587022231 ) ) ;
#44713 = CARTESIAN_POINT ( 'NONE',  ( 125.1626748109119802, -9.988377603198980381, -10.36322818467138518 ) ) ;
#44714 = PRESENTATION_LAYER_ASSIGNMENT (  '', '', ( #35187 ) ) ;
#44715 = CARTESIAN_POINT ( 'NONE',  ( 115.2748327545248657, -6.936859964151250502, -8.388885654883777576 ) ) ;
#44716 = CARTESIAN_POINT ( 'NONE',  ( 124.5930454349294365, -1.040089454026960292, -17.23633227186633476 ) ) ;
#44717 = VERTEX_POINT ( 'NONE', #31907 ) ;
#44718 = CARTESIAN_POINT ( 'NONE',  ( 112.5126281442453120, -10.30919188438810075, -12.61870101168855918 ) ) ;
#44719 = CARTESIAN_POINT ( 'NONE',  ( 121.8158014775786171, -4.153390946401325223, -8.397313243818185668 ) ) ;
#44720 = CARTESIAN_POINT ( 'NONE',  ( 125.0492214775786266, -6.344957434206665248, -7.627207830600338134 ) ) ;
#44721 = ADVANCED_FACE ( 'NONE', ( #7970 ), #33186, .T. ) ;
#44722 = CARTESIAN_POINT ( 'NONE',  ( 117.2209414775786485, -2.084020599724406786, -8.691656652584148546 ) ) ;
#44723 = CARTESIAN_POINT ( 'NONE',  ( 120.0005481442453146, -5.638512984488999180, -18.83840828888717311 ) ) ;
#44724 = CYLINDRICAL_SURFACE ( 'NONE', #30765, 0.5000000000000038858 ) ;
#44725 = CARTESIAN_POINT ( 'NONE',  ( 125.3328548109119964, -0.8288870151387760510, -10.36305467784173118 ) ) ;
#44726 = CARTESIAN_POINT ( 'NONE',  ( 121.9292548109119849, -7.894159318335828068, -9.358103419637847864 ) ) ;
#44727 = ORIENTED_EDGE ( 'NONE', *, *, #4240, .F. ) ;
#44728 = CARTESIAN_POINT ( 'NONE',  ( 63.69189222814998175, -69.76310523276724496, -16.89321520033831447 ) ) ;
#44729 = AXIS2_PLACEMENT_3D ( 'NONE', #26334, #35679, #4453 ) ;
#44730 = CARTESIAN_POINT ( 'NONE',  ( 115.1220548109119761, -8.166667518702817929, -8.995218007635861213 ) ) ;
#44731 = CARTESIAN_POINT ( 'NONE',  ( 123.8012348109119642, -9.565557343593413364, -10.61323700422348004 ) ) ;
#44732 = ORIENTED_EDGE ( 'NONE', *, *, #17958, .F. ) ;
#44733 = CARTESIAN_POINT ( 'NONE',  ( 122.5215798109119874, -2.173413727453600508, -8.297982527556802879 ) ) ;
#44734 = CARTESIAN_POINT ( 'NONE',  ( 137.2352176311277958, -1.230918739026949371, -9.566601454791083370 ) ) ;
#44735 = CARTESIAN_POINT ( 'NONE',  ( 119.9438214775786378, -7.893985811506177619, -18.51759400769804742 ) ) ;
#44736 = CARTESIAN_POINT ( 'NONE',  ( 108.3295202545248657, -10.62599879583958717, -15.77991374673208469 ) ) ;
#44737 = CARTESIAN_POINT ( 'NONE',  ( 118.4122014775786340, -9.859900752359374465, -12.68260735090039404 ) ) ;
#44738 = EDGE_LOOP ( 'NONE', ( #17823, #11860, #13439, #17540, #3935, #28457 ) ) ;
#44739 = ORIENTED_EDGE ( 'NONE', *, *, #6637, .F. ) ;
#44740 = CARTESIAN_POINT ( 'NONE',  ( 126.6942948109119840, -8.899110576539710493, -16.42337572283490132 ) ) ;
#44741 = CARTESIAN_POINT ( 'NONE',  ( 123.1205148109119563, -7.643976991954077427, -18.09477374809248928 ) ) ;
#44742 = LINE ( 'NONE', #10089, #21450 ) ;
#44743 = CIRCLE ( 'NONE', #24330, 5.000000000000004441 ) ;
#44744 = CARTESIAN_POINT ( 'NONE',  ( 121.0216281442452981, -1.561330072975668948, -17.79121239304076951 ) ) ;
#44745 = CARTESIAN_POINT ( 'NONE',  ( 111.4915825099123339, -9.071269598371342724, -16.57136686325032926 ) ) ;
#44746 = ADVANCED_FACE ( 'NONE', ( #3865 ), #7742, .T. ) ;
#44747 = DIRECTION ( 'NONE',  ( 0.4225728684367167087, -0.9063289528979890930, -0.000000000000000000 ) ) ;
#44748 = CARTESIAN_POINT ( 'NONE',  ( 120.0572748109119772, -3.383040157471821630, -19.15922257007629170 ) ) ;
#44750 = CARTESIAN_POINT ( 'NONE',  ( 121.1918081442452859, -10.15424416112533912, -14.75197769757731336 ) ) ;
#44749 = CARTESIAN_POINT ( 'NONE',  ( 118.5823814775786360, -1.834011780172310813, -8.268836392978581529 ) ) ;
#44751 = CARTESIAN_POINT ( 'NONE',  ( 124.3685014775786328, 0.4262465694468514643, -12.03445270309931736 ) ) ;
#44752 = CARTESIAN_POINT ( 'NONE',  ( 117.5613014775786525, 0.9020085738987339008, -11.91225656197089222 ) ) ;
#44753 = EDGE_LOOP ( 'NONE', ( #11740, #20399, #32048, #16031, #19645 ) ) ;
#44754 = CARTESIAN_POINT ( 'NONE',  ( 125.2761281442453054, 0.4262465694468514643, -12.03445270309931736 ) ) ;
#44755 = CARTESIAN_POINT ( 'NONE',  ( 68.89072742534011695, -72.29603325525536661, -37.25697179492874511 ) ) ;
#44756 = CARTESIAN_POINT ( 'NONE',  ( 106.5931921295248372, 0.8980012041604618078, -13.39321520033831447 ) ) ;
#44757 = CARTESIAN_POINT ( 'NONE',  ( 113.6079577545248043, -2.791137627527939813, -18.39754474579286025 ) ) ;
#44758 = CARTESIAN_POINT ( 'NONE',  ( 105.6208483795248299, -0.7896495226426338832, -9.318865927141430916 ) ) ;
#44759 = CARTESIAN_POINT ( 'NONE',  ( 121.1918081442452859, 0.9020085738987339008, -11.91225656197089222 ) ) ;
#44760 = CARTESIAN_POINT ( 'NONE',  ( 123.6310548109119765, -4.153390946401325223, -8.397313243818185668 ) ) ;
#44761 = VERTEX_POINT ( 'NONE', #21207 ) ;
#44762 = CARTESIAN_POINT ( 'NONE',  ( 123.6310548109119765, -5.638512984488999180, -18.83840828888717311 ) ) ;
#44763 = CARTESIAN_POINT ( 'NONE',  ( 111.7327233795247849, -8.938348069036489818, -17.46756447353520159 ) ) ;
#44764 = CARTESIAN_POINT ( 'NONE',  ( 113.3068014775786594, -1.833838273342658809, -17.42832698103878286 ) ) ;
#44765 = DIRECTION ( 'NONE',  ( 0.000000000000000000, 0.000000000000000000, -1.000000000000000000 ) ) ;
#44766 = CARTESIAN_POINT ( 'NONE',  ( 124.9357681442453014, -1.834011780172310813, -8.268836392978581529 ) ) ;
#44767 = CARTESIAN_POINT ( 'NONE',  ( 120.7379948109119709, -10.63000616557722466, -14.87417383870573495 ) ) ;
#44768 = CARTESIAN_POINT ( 'NONE',  ( 120.2264516859119681, -9.030173340179972641, -16.84753301250217561 ) ) ;
#44769 = CARTESIAN_POINT ( 'NONE',  ( 113.2500748109119968, -6.344957434206662583, -7.627207830600332805 ) ) ;
#44770 = CARTESIAN_POINT ( 'NONE',  ( 111.8079953496756787, -1.087735405160635382, -17.17288456429613674 ) ) ;
#44771 = CARTESIAN_POINT ( 'NONE',  ( 115.8304577545247582, -2.791137627527939813, -18.39754474579286025 ) ) ;
#44772 = AXIS2_PLACEMENT_3D ( 'NONE', #4613, #1199, #15334 ) ;
#44773 = ORIENTED_EDGE ( 'NONE', *, *, #29199, .F. ) ;
#44774 = DIRECTION ( 'NONE',  ( 0.000000000000000000, 0.6004852223388323917, -0.7996358532186279566 ) ) ;
#44775 = CARTESIAN_POINT ( 'NONE',  ( 118.5378868052895456, -1.125321370491268125, -17.12283323191015327 ) ) ;
#44776 = CARTESIAN_POINT ( 'NONE',  ( 124.2550481442452792, -0.1624402480850797581, -16.17319339645315424 ) ) ;
#44777 = CARTESIAN_POINT ( 'NONE',  ( 106.1070202545248407, 0.1403307496149616695, -11.32035403202665336 ) ) ;
#44778 = CARTESIAN_POINT ( 'NONE',  ( 107.2877233795247776, -1.325403438956436419, -9.854619843455211026 ) ) ;
#44779 = CARTESIAN_POINT ( 'NONE',  ( 123.0070614775786169, -10.15424416112533912, -14.75197769757731336 ) ) ;
#44780 = CARTESIAN_POINT ( 'NONE',  ( 116.1431348109119881, 0.1319031606808879209, -14.10382304977623669 ) ) ;
#44781 = CARTESIAN_POINT ( 'NONE',  ( 112.7395348109119766, -4.153390946401321671, -8.397313243818183892 ) ) ;
#44782 = ORIENTED_EDGE ( 'NONE', *, *, #15267, .F. ) ;
#44783 = AXIS2_PLACEMENT_3D ( 'NONE', #31207, #45129, #9805 ) ;
#44784 = CARTESIAN_POINT ( 'NONE',  ( 121.1350814775786233, -9.859900752359378018, -12.68260735090039759 ) ) ;
#44785 = CARTESIAN_POINT ( 'NONE',  ( 117.3343948109119737, -3.383040157471821630, -19.15922257007629170 ) ) ;
#44786 = DIRECTION ( 'NONE',  ( 0.000000000000000000, 0.9242245927363040847, 0.3818493186865896671 ) ) ;
#44787 = EDGE_LOOP ( 'NONE', ( #2972, #10368, #43924, #28071, #34972, #3567, #25385 ) ) ;
#44788 = CARTESIAN_POINT ( 'NONE',  ( 121.2714235609119697, -9.645473719204778362, -14.86997237629376123 ) ) ;
#44789 = EDGE_LOOP ( 'NONE', ( #43312, #37234, #5579, #7357, #23524 ) ) ;
#44790 = CARTESIAN_POINT ( 'NONE',  ( 115.7460481442453357, -10.15424416112533912, -14.75197769757731336 ) ) ;
#44791 = CARTESIAN_POINT ( 'NONE',  ( 113.9875214775786532, -8.899110576539710493, -16.42337572283490132 ) ) ;
#44792 = CARTESIAN_POINT ( 'NONE',  ( 115.0653281442453135, -6.344957434206662583, -7.627207830600333693 ) ) ;
#44793 = CARTESIAN_POINT ( 'NONE',  ( 120.0907204359119760, 1.345710702986147034, -13.97328579221134426 ) ) ;
#44794 = VERTEX_POINT ( 'NONE', #21879 ) ;
#44795 = CARTESIAN_POINT ( 'NONE',  ( 59.62174278132244609, -14.86814543204979522, -8.593215200338313764 ) ) ;
#44796 = CARTESIAN_POINT ( 'NONE',  ( 83.75466360696344736, -7.807702403958562520, -18.64321520033831803 ) ) ;
#44797 = CIRCLE ( 'NONE', #29478, 2.999999999999999556 ) ;
#44798 = CARTESIAN_POINT ( 'NONE',  ( 114.0246765045248196, -7.250697342233347165, -19.15521520033831138 ) ) ;
#44799 = CARTESIAN_POINT ( 'NONE',  ( 92.22433883960545131, -8.119819663282910938, -8.143215200338314474 ) ) ;
#44800 = CARTESIAN_POINT ( 'NONE',  ( 124.3685014775786328, 0.4262465694468514643, -12.03445270309931736 ) ) ;
#44801 = CARTESIAN_POINT ( 'NONE',  ( 113.4202548109119846, 0.1319031606808879209, -14.10382304977623669 ) ) ;
#44802 = CARTESIAN_POINT ( 'NONE',  ( 126.2561087589866275, -5.799764584263661149, -18.32404662456333000 ) ) ;
#44803 = ORIENTED_EDGE ( 'NONE', *, *, #25820, .T. ) ;
#44804 = DIRECTION ( 'NONE',  ( -0.2768435750659243300, -0.3568721902840689131, 0.8921882507333129819 ) ) ;
#44805 = CIRCLE ( 'NONE', #41164, 2.999999999999998224 ) ;
#44806 = CARTESIAN_POINT ( 'NONE',  ( 112.1722681442453222, -8.899110576539710493, -16.42337572283490132 ) ) ;
#44807 = EDGE_CURVE ( 'NONE', #7405, #20846, #1178, .T. ) ;
#44808 = CARTESIAN_POINT ( 'NONE',  ( 112.8439733795247832, -8.938348069036441856, -17.46756447353520514 ) ) ;
#44809 = DIRECTION ( 'NONE',  ( 0.000000000000000000, 0.000000000000000000, -1.000000000000000000 ) ) ;
#44811 = DIRECTION ( 'NONE',  ( 0.000000000000000000, -0.9242245927363029745, -0.3818493186865927203 ) ) ;
#44810 = CARTESIAN_POINT ( 'NONE',  ( 64.69075612292361654, -36.94291761115415795, -5.470407532193525491 ) ) ;
#44812 = CARTESIAN_POINT ( 'NONE',  ( 124.6521348109119884, -7.894159318335828068, -9.358103419637847864 ) ) ;
#44813 = ORIENTED_EDGE ( 'NONE', *, *, #4400, .T. ) ;
#44814 = CARTESIAN_POINT ( 'NONE',  ( 111.9453614775786434, -1.561330072975668060, -17.79121239304076596 ) ) ;
#44815 = DIRECTION ( 'NONE',  ( 0.000000000000000000, 0.000000000000000000, 1.000000000000000000 ) ) ;
#44816 = CARTESIAN_POINT ( 'NONE',  ( 114.2330358795247776, -0.7896495226426338832, -17.46756447353520159 ) ) ;
#44817 = CARTESIAN_POINT ( 'NONE',  ( 125.6732148109119862, -9.859900752359378018, -12.68260735090039759 ) ) ;
#44818 = CARTESIAN_POINT ( 'NONE',  ( 122.3830681442452857, -1.833838273342659697, -17.42832698103878286 ) ) ;
#44819 = EDGE_CURVE ( 'NONE', #43595, #9931, #24631, .T. ) ;
#44820 = CARTESIAN_POINT ( 'NONE',  ( 69.69189222814998175, -41.76310523276723785, -47.71602681600972318 ) ) ;
#44821 = CARTESIAN_POINT ( 'NONE',  ( 114.3024890045248156, -9.868328341294098749, -11.32035403202665869 ) ) ;
#44822 = CARTESIAN_POINT ( 'NONE',  ( 120.4709786403692249, -1.196538596002817867, -17.02799684832028504 ) ) ;
#44823 = CARTESIAN_POINT ( 'NONE',  ( 120.0212673109119805, -9.289237151508434209, -11.05642687123711454 ) ) ;
#44824 = CARTESIAN_POINT ( 'NONE',  ( 112.9097148109119928, -9.565557343593411588, -10.61323700422346583 ) ) ;
#44825 = CARTESIAN_POINT ( 'NONE',  ( 106.1070202545248407, -10.62599879583958717, -15.77991374673208469 ) ) ;
#44826 = CARTESIAN_POINT ( 'NONE',  ( 117.5045748109119756, 0.5811942927096067635, -14.16772938898808576 ) ) ;
#44827 = CARTESIAN_POINT ( 'NONE',  ( 109.8574890045247940, 0.8980012041604421569, -15.77991374673208469 ) ) ;
#44828 = CARTESIAN_POINT ( 'NONE',  ( 74.47157298427187300, -3.053873105668316601, -7.147228641687434880 ) ) ;
#44829 = CARTESIAN_POINT ( 'NONE',  ( 111.8886348109120092, -6.222761293078241884, -8.102969835052219238 ) ) ;
#44830 = DIRECTION ( 'NONE',  ( 1.000000000000000000, 0.000000000000000000, 0.000000000000000000 ) ) ;
#44831 =( BOUNDED_SURFACE ( )  B_SPLINE_SURFACE ( 1, 2, ( 
 ( #23726, #19610, #44021, #19843, #40828, #2729, #15973, #26463, #41285, #20523, #16885, #27365, #12782, #30549, #34183, #16202, #13463, #13235, #16654, #30105, #2049, #10048, #9354, #30325, #40366, #33961, #33731, #33494, #6156, #5921, #44470, #9583, #23499, #23952, #20076, #9817, #37385, #43792, #6391, #9129, #20298, #2958, #27137, #16429, #44252, #26684, #2502, #36921, #30777, #2272, #40596, #23264, #13009, #26908, #44702, #37833, #6610, #29876, #5691, #17984, #41720, #24827, #17541, #41506, #20744, #34836, #6838, #17109, #24607, #38950, #7717, #38718, #38272, #7489, #10925, #34623, #24386, #7053, #42164, #10484, #38490, #41941, #3409, #10261, #21182, #20964, #21406, #35287, #3621, #34403, #7265, #201, #4060, #31434, #31884, #28034, #42387, #30999, #3184, #14117, #24168, #11151, #31657, #425, #649, #17760, #35059, #28483, #14564, #25057, #10704, #44925, #13683, #3840, #27593, #14341, #38060, #17326, #28255, #31216, #45142, #13899, #27805, #43283, #8627, #7943, #15019, #43058, #32558, #11825, #18446, #25732, #18880, #14793, #22527, #18665, #25283, #36423, #4290, #39413, #29145, #28707, #39639, #8403, #42614, #32994, #15236, #19110, #15466, #1325, #1768, #29372, #1102, #12054, #25955, #21854, #22086, #15694, #35974, #35750, #29596, #22307, #32107, #12282, #36203, #21630, #40086, #39862, #28930, #5192, #4970, #32771, #4745, #11377, #18209, #43513, #26178, #8176, #1545, #35518, #42837, #39179, #874, #32335, #4523, #11598, #25508, #44416, #19787, #29821, #9759, #8847, #40313, #16831, #22980, #36869, #16603, #16146, #30272, #5421, #37327, #5639, #37561, #43737, #6330, #30496, #26403, #19560, #26630, #2449, #9526, #22747, #19338, #2902, #27312, #23671, #34133, #33437, #6098, #41006, #2216, #20247, #20018, #23442, #30050, #36648, #30724, #43963, #37091, #33223, #40768, #40543, #9077, #12959, #12727, #33901, #16369, #44197, #44647, #26855, #2671, #13182, #9304, #13409, #27085, #1998, #12507, #15924, #23212, #5865, #33671, #10876, #38011, #31382, #17935, #14514, #17710 ),
 ( #7432, #10433, #10209, #21352, #34789, #6555, #31834, #20915, #37782, #378, #20472, #35002, #42116, #3573, #24340, #38224, #24117, #13844, #34353, #153, #13628, #34573, #6786, #41451, #20695, #3785, #38444, #27539, #14290, #31609, #3357, #9990, #14068, #23899, #28208, #7006, #17056, #24772, #41230, #17275, #4012, #31167, #45088, #38664, #27760, #17485, #3133, #24558, #41675, #35236, #30948, #603, #44872, #27986, #41891, #10652, #7214, #21127, #42338, #38894, #22474, #1717, #43232, #8573, #25231, #11771, #15414, #42559, #39806, #39586, #43002, #11320, #28426, #36368, #35695, #11549, #7663, #15187, #14963, #821, #32501, #32282, #29091, #22029, #35923, #5139, #1275, #22249, #18609, #1048, #19055, #4689, #21579, #4241, #18828, #35466, #42788, #25679, #11998, #39128, #8347, #32941, #11098, #4913, #36145, #25901, #32720, #18391, #1492, #7895, #25000, #28876, #29319, #18158, #4471, #8127, #14741, #32054, #28653, #25457, #21802, #39360, #16088, #23160, #26577, #2392, #22924, #37041, #33615, #26123, #19961, #40491, #9474, #40260, #40028, #23385, #29993, #20198, #22699, #36595, #15640, #34082, #6039, #36817, #44367, #5811, #30223, #43910, #8792, #43461, #33850, #27033, #2160, #12679, #16552, #9026, #5371, #5586, #19288, #16320, #9252, #19730, #44143, #12909, #19509, #26805, #40715, #33167, #2619, #37270, #30447, #33387, #1943, #13129, #40948, #29544, #15868, #29765, #12225, #43676, #9705, #23618, #37504, #6278, #12451, #26352, #41176, #30674, #21075, #14238, #34522, #45039, #3738, #27487, #23850, #24506, #44818, #16781, #20860, #44594, #38391, #13799, #37736, #17661, #2849, #34306, #10822, #17007, #30896, #10604, #10161, #24291, #13357, #31332, #13576, #31557, #6507, #325, #7163, #20422, #41405, #20646, #41625, #3521, #27262, #9936, #42065, #21302, #28155, #24719, #24069, #106, #34952, #37960, #38608, #14019, #17439, #6736, #3079, #7384, #3300, #31115, #17224, #34739, #27711, #10381, #6955, #38177, #27934, #41844, #28825, #11948, #8075, #29044, #25405, #39077, #25844 ) ),
 .UNSPECIFIED., .F., .F., .T. ) 
 B_SPLINE_SURFACE_WITH_KNOTS ( ( 2, 2 ),
 ( 3, 2, 2, 2, 2, 2, 2, 2, 2, 2, 2, 2, 2, 2, 2, 2, 2, 2, 2, 2, 2, 2, 2, 2, 2, 2, 2, 2, 2, 2, 2, 2, 2, 2, 2, 2, 2, 2, 2, 2, 2, 2, 2, 2, 2, 2, 2, 2, 2, 2, 2, 2, 2, 2, 2, 2, 2, 2, 2, 2, 2, 2, 2, 2, 2, 2, 2, 2, 2, 2, 2, 2, 2, 2, 2, 2, 2, 2, 2, 2, 2, 2, 2, 2, 2, 2, 2, 2, 2, 2, 2, 2, 2, 2, 2, 2, 2, 2, 2, 2, 2, 2, 2, 2, 2, 2, 2, 2, 2, 2, 2, 2, 2, 2, 2, 2, 2, 2, 2, 2, 2, 2, 2, 2, 2, 2, 2, 2, 3 ),
 ( 0.000000000000000000, 1.000000000000000000 ),
 ( 0.000000000000000000, 0.007812500000000000000, 0.01562500000000000000, 0.02343750000000000000, 0.03125000000000000000, 0.03906250000000000000, 0.04687500000000000000, 0.05468750000000000000, 0.06250000000000000000, 0.07031250000000000000, 0.07812500000000000000, 0.08593750000000000000, 0.09375000000000000000, 0.1015625000000000000, 0.1093750000000000000, 0.1171875000000000000, 0.1250000000000000000, 0.1328125000000000000, 0.1406250000000000000, 0.1484375000000000000, 0.1562500000000000000, 0.1640625000000000000, 0.1718750000000000000, 0.1796875000000000000, 0.1875000000000000000, 0.1953125000000000000, 0.2031250000000000000, 0.2109375000000000000, 0.2187500000000000000, 0.2265625000000000000, 0.2343750000000000000, 0.2421875000000000000, 0.2500000000000000000, 0.2578125000000000000, 0.2656250000000000000, 0.2734375000000000000, 0.2812500000000000000, 0.2890625000000000000, 0.2968750000000000000, 0.3046875000000000000, 0.3125000000000000000, 0.3203125000000000000, 0.3281250000000000000, 0.3359375000000000000, 0.3437500000000000000, 0.3515625000000000000, 0.3593750000000000000, 0.3671875000000000000, 0.3750000000000000000, 0.3828125000000000000, 0.3906250000000000000, 0.3984375000000000000, 0.4062500000000000000, 0.4140625000000000000, 0.4218750000000000000, 0.4296875000000000000, 0.4375000000000000000, 0.4453125000000000000, 0.4531250000000000000, 0.4609375000000000000, 0.4687500000000000000, 0.4765625000000000000, 0.4843750000000000000, 0.4921875000000000000, 0.5000000000000000000, 0.5078125000000000000, 0.5156250000000000000, 0.5234375000000000000, 0.5312500000000000000, 0.5390625000000000000, 0.5468750000000000000, 0.5546875000000000000, 0.5625000000000000000, 0.5703125000000000000, 0.5781250000000000000, 0.5859375000000000000, 0.5937500000000000000, 0.6015625000000000000, 0.6093750000000000000, 0.6171875000000000000, 0.6250000000000000000, 0.6328125000000000000, 0.6406250000000000000, 0.6484375000000000000, 0.6562500000000000000, 0.6640625000000000000, 0.6718750000000000000, 0.6796875000000000000, 0.6875000000000000000, 0.6953125000000000000, 0.7031250000000000000, 0.7109375000000000000, 0.7187500000000000000, 0.7265625000000000000, 0.7343750000000000000, 0.7421875000000000000, 0.7500000000000000000, 0.7578125000000000000, 0.7656250000000000000, 0.7734375000000000000, 0.7812500000000000000, 0.7890625000000000000, 0.7968750000000000000, 0.8046875000000000000, 0.8125000000000000000, 0.8203125000000000000, 0.8281250000000000000, 0.8359375000000000000, 0.8437500000000000000, 0.8515625000000000000, 0.8593750000000000000, 0.8671875000000000000, 0.8750000000000000000, 0.8828125000000000000, 0.8906250000000000000, 0.8984375000000000000, 0.9062500000000000000, 0.9140625000000000000, 0.9218750000000000000, 0.9296875000000000000, 0.9375000000000000000, 0.9453125000000000000, 0.9531250000000000000, 0.9609375000000000000, 0.9687500000000000000, 0.9765625000000000000, 0.9843750000000000000, 0.9921875000000000000, 1.000000000000000000 ),
 .UNSPECIFIED. ) 
 GEOMETRIC_REPRESENTATION_ITEM ( )  RATIONAL_B_SPLINE_SURFACE ( (
 ( 1.000000000000000000, 0.9238795325112869605, 1.000000000000000000, 0.9238795325112869605, 1.000000000000000000, 0.9238795325112869605, 1.000000000000000000, 0.9238795325112869605, 1.000000000000000000, 0.9238795325112869605, 1.000000000000000000, 0.9238795325112869605, 1.000000000000000000, 0.9238795325112869605, 1.000000000000000000, 0.9238795325112869605, 1.000000000000000000, 0.9238795325112869605, 1.000000000000000000, 0.9238795325112869605, 1.000000000000000000, 0.9238795325112869605, 1.000000000000000000, 0.9238795325112869605, 1.000000000000000000, 0.9238795325112869605, 1.000000000000000000, 0.9238795325112869605, 1.000000000000000000, 0.9238795325112869605, 1.000000000000000000, 0.9238795325112869605, 1.000000000000000000, 0.9238795325112869605, 1.000000000000000000, 0.9238795325112869605, 1.000000000000000000, 0.9238795325112869605, 1.000000000000000000, 0.9238795325112869605, 1.000000000000000000, 0.9238795325112869605, 1.000000000000000000, 0.9238795325112869605, 1.000000000000000000, 0.9238795325112869605, 1.000000000000000000, 0.9238795325112869605, 1.000000000000000000, 0.9238795325112869605, 1.000000000000000000, 0.9238795325112869605, 1.000000000000000000, 0.9238795325112869605, 1.000000000000000000, 0.9238795325112869605, 1.000000000000000000, 0.9238795325112869605, 1.000000000000000000, 0.9238795325112869605, 1.000000000000000000, 0.9238795325112869605, 1.000000000000000000, 0.9238795325112869605, 1.000000000000000000, 0.9238795325112869605, 1.000000000000000000, 0.9238795325112869605, 1.000000000000000000, 0.9238795325112869605, 1.000000000000000000, 0.9238795325112869605, 1.000000000000000000, 0.9238795325112869605, 1.000000000000000000, 0.9238795325112869605, 1.000000000000000000, 0.9238795325112869605, 1.000000000000000000, 0.9238795325112869605, 1.000000000000000000, 0.9238795325112869605, 1.000000000000000000, 0.9238795325112869605, 1.000000000000000000, 0.9238795325112869605, 1.000000000000000000, 0.9238795325112869605, 1.000000000000000000, 0.9238795325112869605, 1.000000000000000000, 0.9238795325112869605, 1.000000000000000000, 0.9238795325112869605, 1.000000000000000000, 0.9238795325112869605, 1.000000000000000000, 0.9238795325112869605, 1.000000000000000000, 0.9238795325112869605, 1.000000000000000000, 0.9238795325112869605, 1.000000000000000000, 0.9238795325112869605, 1.000000000000000000, 0.9238795325112869605, 1.000000000000000000, 0.9238795325112869605, 1.000000000000000000, 0.9238795325112869605, 1.000000000000000000, 0.9238795325112869605, 1.000000000000000000, 0.9238795325112869605, 1.000000000000000000, 0.9238795325112869605, 1.000000000000000000, 0.9238795325112869605, 1.000000000000000000, 0.9238795325112869605, 1.000000000000000000, 0.9238795325112869605, 1.000000000000000000, 0.9238795325112869605, 1.000000000000000000, 0.9238795325112869605, 1.000000000000000000, 0.9238795325112869605, 1.000000000000000000, 0.9238795325112869605, 1.000000000000000000, 0.9238795325112869605, 1.000000000000000000, 0.9238795325112869605, 1.000000000000000000, 0.9238795325112869605, 1.000000000000000000, 0.9238795325112869605, 1.000000000000000000, 0.9238795325112869605, 1.000000000000000000, 0.9238795325112869605, 1.000000000000000000, 0.9238795325112869605, 1.000000000000000000, 0.9238795325112869605, 1.000000000000000000, 0.9238795325112869605, 1.000000000000000000, 0.9238795325112869605, 1.000000000000000000, 0.9238795325112869605, 1.000000000000000000, 0.9238795325112869605, 1.000000000000000000, 0.9238795325112869605, 1.000000000000000000, 0.9238795325112869605, 1.000000000000000000, 0.9238795325112869605, 1.000000000000000000, 0.9238795325112869605, 1.000000000000000000, 0.9238795325112869605, 1.000000000000000000, 0.9238795325112869605, 1.000000000000000000, 0.9238795325112869605, 1.000000000000000000, 0.9238795325112869605, 1.000000000000000000, 0.9238795325112869605, 1.000000000000000000, 0.9238795325112869605, 1.000000000000000000, 0.9238795325112869605, 1.000000000000000000, 0.9238795325112869605, 1.000000000000000000, 0.9238795325112869605, 1.000000000000000000, 0.9238795325112869605, 1.000000000000000000, 0.9238795325112869605, 1.000000000000000000, 0.9238795325112869605, 1.000000000000000000, 0.9238795325112869605, 1.000000000000000000, 0.9238795325112869605, 1.000000000000000000, 0.9238795325112869605, 1.000000000000000000, 0.9238795325112869605, 1.000000000000000000, 0.9238795325112869605, 1.000000000000000000, 0.9238795325112869605, 1.000000000000000000, 0.9238795325112869605, 1.000000000000000000, 0.9238795325112869605, 1.000000000000000000, 0.9238795325112869605, 1.000000000000000000, 0.9238795325112869605, 1.000000000000000000, 0.9238795325112869605, 1.000000000000000000, 0.9238795325112869605, 1.000000000000000000, 0.9238795325112869605, 1.000000000000000000, 0.9238795325112869605, 1.000000000000000000, 0.9238795325112869605, 1.000000000000000000, 0.9238795325112869605, 1.000000000000000000, 0.9238795325112869605, 1.000000000000000000, 0.9238795325112869605, 1.000000000000000000, 0.9238795325112869605, 1.000000000000000000, 0.9238795325112869605, 1.000000000000000000, 0.9238795325112869605, 1.000000000000000000, 0.9238795325112869605, 1.000000000000000000, 0.9238795325112869605, 1.000000000000000000, 0.9238795325112869605, 1.000000000000000000, 0.9238795325112869605, 1.000000000000000000, 0.9238795325112869605, 1.000000000000000000, 0.9238795325112869605, 1.000000000000000000, 0.9238795325112869605, 1.000000000000000000, 0.9238795325112869605, 1.000000000000000000, 0.9238795325112869605, 1.000000000000000000, 0.9238795325112869605, 1.000000000000000000, 0.9238795325112869605, 1.000000000000000000, 0.9238795325112869605, 1.000000000000000000, 0.9238795325112869605, 1.000000000000000000, 0.9238795325112869605, 1.000000000000000000),
 ( 1.000000000000000000, 0.9238795325112869605, 1.000000000000000000, 0.9238795325112869605, 1.000000000000000000, 0.9238795325112869605, 1.000000000000000000, 0.9238795325112869605, 1.000000000000000000, 0.9238795325112869605, 1.000000000000000000, 0.9238795325112869605, 1.000000000000000000, 0.9238795325112869605, 1.000000000000000000, 0.9238795325112869605, 1.000000000000000000, 0.9238795325112869605, 1.000000000000000000, 0.9238795325112869605, 1.000000000000000000, 0.9238795325112869605, 1.000000000000000000, 0.9238795325112869605, 1.000000000000000000, 0.9238795325112869605, 1.000000000000000000, 0.9238795325112869605, 1.000000000000000000, 0.9238795325112869605, 1.000000000000000000, 0.9238795325112869605, 1.000000000000000000, 0.9238795325112869605, 1.000000000000000000, 0.9238795325112869605, 1.000000000000000000, 0.9238795325112869605, 1.000000000000000000, 0.9238795325112869605, 1.000000000000000000, 0.9238795325112869605, 1.000000000000000000, 0.9238795325112869605, 1.000000000000000000, 0.9238795325112869605, 1.000000000000000000, 0.9238795325112869605, 1.000000000000000000, 0.9238795325112869605, 1.000000000000000000, 0.9238795325112869605, 1.000000000000000000, 0.9238795325112869605, 1.000000000000000000, 0.9238795325112869605, 1.000000000000000000, 0.9238795325112869605, 1.000000000000000000, 0.9238795325112869605, 1.000000000000000000, 0.9238795325112869605, 1.000000000000000000, 0.9238795325112869605, 1.000000000000000000, 0.9238795325112869605, 1.000000000000000000, 0.9238795325112869605, 1.000000000000000000, 0.9238795325112869605, 1.000000000000000000, 0.9238795325112869605, 1.000000000000000000, 0.9238795325112869605, 1.000000000000000000, 0.9238795325112869605, 1.000000000000000000, 0.9238795325112869605, 1.000000000000000000, 0.9238795325112869605, 1.000000000000000000, 0.9238795325112869605, 1.000000000000000000, 0.9238795325112869605, 1.000000000000000000, 0.9238795325112869605, 1.000000000000000000, 0.9238795325112869605, 1.000000000000000000, 0.9238795325112869605, 1.000000000000000000, 0.9238795325112869605, 1.000000000000000000, 0.9238795325112869605, 1.000000000000000000, 0.9238795325112869605, 1.000000000000000000, 0.9238795325112869605, 1.000000000000000000, 0.9238795325112869605, 1.000000000000000000, 0.9238795325112869605, 1.000000000000000000, 0.9238795325112869605, 1.000000000000000000, 0.9238795325112869605, 1.000000000000000000, 0.9238795325112869605, 1.000000000000000000, 0.9238795325112869605, 1.000000000000000000, 0.9238795325112869605, 1.000000000000000000, 0.9238795325112869605, 1.000000000000000000, 0.9238795325112869605, 1.000000000000000000, 0.9238795325112869605, 1.000000000000000000, 0.9238795325112869605, 1.000000000000000000, 0.9238795325112869605, 1.000000000000000000, 0.9238795325112869605, 1.000000000000000000, 0.9238795325112869605, 1.000000000000000000, 0.9238795325112869605, 1.000000000000000000, 0.9238795325112869605, 1.000000000000000000, 0.9238795325112869605, 1.000000000000000000, 0.9238795325112869605, 1.000000000000000000, 0.9238795325112869605, 1.000000000000000000, 0.9238795325112869605, 1.000000000000000000, 0.9238795325112869605, 1.000000000000000000, 0.9238795325112869605, 1.000000000000000000, 0.9238795325112869605, 1.000000000000000000, 0.9238795325112869605, 1.000000000000000000, 0.9238795325112869605, 1.000000000000000000, 0.9238795325112869605, 1.000000000000000000, 0.9238795325112869605, 1.000000000000000000, 0.9238795325112869605, 1.000000000000000000, 0.9238795325112869605, 1.000000000000000000, 0.9238795325112869605, 1.000000000000000000, 0.9238795325112869605, 1.000000000000000000, 0.9238795325112869605, 1.000000000000000000, 0.9238795325112869605, 1.000000000000000000, 0.9238795325112869605, 1.000000000000000000, 0.9238795325112869605, 1.000000000000000000, 0.9238795325112869605, 1.000000000000000000, 0.9238795325112869605, 1.000000000000000000, 0.9238795325112869605, 1.000000000000000000, 0.9238795325112869605, 1.000000000000000000, 0.9238795325112869605, 1.000000000000000000, 0.9238795325112869605, 1.000000000000000000, 0.9238795325112869605, 1.000000000000000000, 0.9238795325112869605, 1.000000000000000000, 0.9238795325112869605, 1.000000000000000000, 0.9238795325112869605, 1.000000000000000000, 0.9238795325112869605, 1.000000000000000000, 0.9238795325112869605, 1.000000000000000000, 0.9238795325112869605, 1.000000000000000000, 0.9238795325112869605, 1.000000000000000000, 0.9238795325112869605, 1.000000000000000000, 0.9238795325112869605, 1.000000000000000000, 0.9238795325112869605, 1.000000000000000000, 0.9238795325112869605, 1.000000000000000000, 0.9238795325112869605, 1.000000000000000000, 0.9238795325112869605, 1.000000000000000000, 0.9238795325112869605, 1.000000000000000000, 0.9238795325112869605, 1.000000000000000000, 0.9238795325112869605, 1.000000000000000000, 0.9238795325112869605, 1.000000000000000000, 0.9238795325112869605, 1.000000000000000000, 0.9238795325112869605, 1.000000000000000000, 0.9238795325112869605, 1.000000000000000000, 0.9238795325112869605, 1.000000000000000000, 0.9238795325112869605, 1.000000000000000000, 0.9238795325112869605, 1.000000000000000000, 0.9238795325112869605, 1.000000000000000000, 0.9238795325112869605, 1.000000000000000000, 0.9238795325112869605, 1.000000000000000000, 0.9238795325112869605, 1.000000000000000000, 0.9238795325112869605, 1.000000000000000000, 0.9238795325112869605, 1.000000000000000000, 0.9238795325112869605, 1.000000000000000000, 0.9238795325112869605, 1.000000000000000000, 0.9238795325112869605, 1.000000000000000000, 0.9238795325112869605, 1.000000000000000000, 0.9238795325112869605, 1.000000000000000000, 0.9238795325112869605, 1.000000000000000000, 0.9238795325112869605, 1.000000000000000000, 0.9238795325112869605, 1.000000000000000000) ) ) 
 REPRESENTATION_ITEM ( '' )  SURFACE ( )  );
#44832 = CARTESIAN_POINT ( 'NONE',  ( 120.9649014775786355, -3.383040157471821630, -19.15922257007629170 ) ) ;
#44833 = CARTESIAN_POINT ( 'NONE',  ( 112.0020881442453344, 0.2603800115204892296, -16.42320221600525088 ) ) ;
#44834 = ORIENTED_EDGE ( 'NONE', *, *, #29504, .T. ) ;
#44835 = CARTESIAN_POINT ( 'NONE',  ( 112.9664414775786412, -9.859900752359374465, -12.68260735090039404 ) ) ;
#44836 = EDGE_CURVE ( 'NONE', #26941, #39210, #11178, .T. ) ;
#44837 = CIRCLE ( 'NONE', #12042, 2.999999999999999556 ) ;
#44838 = CARTESIAN_POINT ( 'NONE',  ( 125.9001214775786224, -4.089484607189486809, -7.948022111789456723 ) ) ;
#44839 = CARTESIAN_POINT ( 'NONE',  ( 124.9924948109119924, -4.089484607189486809, -7.948022111789456723 ) ) ;
#44840 = CARTESIAN_POINT ( 'NONE',  ( 114.1577014775786552, -6.344957434206662583, -7.627207830600332805 ) ) ;
#44841 = CARTESIAN_POINT ( 'NONE',  ( 116.1998614775786507, 0.4262465694468514643, -12.03445270309931736 ) ) ;
#44842 = ORIENTED_EDGE ( 'NONE', *, *, #37659, .T. ) ;
#44843 = EDGE_CURVE ( 'NONE', #36736, #4599, #40678, .T. ) ;
#44844 = CARTESIAN_POINT ( 'NONE',  ( 118.9227414775786542, 0.4262465694468514643, -12.03445270309931736 ) ) ;
#44845 = EDGE_CURVE ( 'NONE', #21905, #3495, #42859, .T. ) ;
#44846 = EDGE_CURVE ( 'NONE', #8410, #44542, #8198, .T. ) ;
#44847 = CIRCLE ( 'NONE', #1133, 6.132259260909266985 ) ;
#44848 = CARTESIAN_POINT ( 'NONE',  ( 116.9373081442452929, -8.166667518702817929, -8.995218007635861213 ) ) ;
#44849 = CARTESIAN_POINT ( 'NONE',  ( 123.0070614775786169, -10.15424416112533912, -14.75197769757731336 ) ) ;
#44850 = DIRECTION ( 'NONE',  ( -0.9063289528979890930, -0.4225728684367167087, 0.000000000000000000 ) ) ;
#44851 = CARTESIAN_POINT ( 'NONE',  ( 114.8581140045248361, -10.62599879583958717, -11.00651665394454604 ) ) ;
#44852 = ORIENTED_EDGE ( 'NONE', *, *, #11469, .T. ) ;
#44853 = CARTESIAN_POINT ( 'NONE',  ( 119.7434548109119703, 2.250047331442289966, -9.733932798157443500 ) ) ;
#44854 = DIRECTION ( 'NONE',  ( -1.000000000000000000, -1.697309329729404623E-15, 0.000000000000000000 ) ) ;
#44855 = CARTESIAN_POINT ( 'NONE',  ( 116.2471765045247594, -2.791137627527939813, -8.388885654883777576 ) ) ;
#44856 = AXIS2_PLACEMENT_3D ( 'NONE', #13361, #23853, #17665 ) ;
#44857 = CARTESIAN_POINT ( 'NONE',  ( 116.7920406659710864, 2.007758018742032302, -5.899424721369208591 ) ) ;
#44858 = CARTESIAN_POINT ( 'NONE',  ( 112.3991748109119868, -1.833838273342658809, -17.42832698103878286 ) ) ;
#44859 = CARTESIAN_POINT ( 'NONE',  ( 107.3571765045248299, -2.791137627527939813, -8.388885654883777576 ) ) ;
#44860 = CARTESIAN_POINT ( 'NONE',  ( 94.86797725101182266, -26.75172757040932936, -12.91007389524920157 ) ) ;
#44861 = CARTESIAN_POINT ( 'NONE',  ( 119.4332814775786318, -0.4660016031367893996, -10.09054647747474043 ) ) ;
#44862 = CARTESIAN_POINT ( 'NONE',  ( 136.4577890465943995, -4.246979716881710942, -19.12709517244668334 ) ) ;
#44863 = CARTESIAN_POINT ( 'NONE',  ( 115.5212212410415873, 0.7607806665037644134, -12.14321520033829493 ) ) ;
#44864 = CARTESIAN_POINT ( 'NONE',  ( 118.9794681442453026, -9.261995988541702474, -16.69588392320187964 ) ) ;
#44865 = CARTESIAN_POINT ( 'NONE',  ( 121.5888948109119809, 0.1319031606808879209, -14.10382304977623669 ) ) ;
#44866 = ORIENTED_EDGE ( 'NONE', *, *, #14431, .F. ) ;
#44867 = CARTESIAN_POINT ( 'NONE',  ( 126.1270281442452870, -10.30919188438810075, -12.61870101168855918 ) ) ;
#44868 = CARTESIAN_POINT ( 'NONE',  ( 119.2063748109119814, -1.561330072975668504, -17.79121239304076951 ) ) ;
#44869 = DIRECTION ( 'NONE',  ( -1.000000000000000000, 0.000000000000000000, 0.000000000000000000 ) ) ;
#44870 = CARTESIAN_POINT ( 'NONE',  ( 116.3133148109120043, -2.084020599724406786, -8.691656652584148546 ) ) ;
#44871 = CIRCLE ( 'NONE', #39022, 1.610000000000000986 ) ;
#44872 = CARTESIAN_POINT ( 'NONE',  ( 114.2144281442453178, -1.833838273342658809, -17.42832698103878286 ) ) ;
#44873 = CARTESIAN_POINT ( 'NONE',  ( 110.8298327545248299, -2.477300249445798297, -19.15521520033831138 ) ) ;
#44874 = CARTESIAN_POINT ( 'NONE',  ( 69.69189222815028018, -41.76310523276638520, -7.393215200338315363 ) ) ;
#44875 = CARTESIAN_POINT ( 'NONE',  ( 115.2053796295247849, -4.863998795839590272, -19.15521520033831493 ) ) ;
#44876 = CARTESIAN_POINT ( 'NONE',  ( 118.3554748109119998, -9.565557343593413364, -10.61323700422348004 ) ) ;
#44877 = CARTESIAN_POINT ( 'NONE',  ( 118.9794681442453026, -0.8288870151387760510, -10.36305467784173118 ) ) ;
#44878 = AXIS2_PLACEMENT_3D ( 'NONE', #10949, #28280, #35772 ) ;
#44879 = CARTESIAN_POINT ( 'NONE',  ( 69.69189222815028018, -41.76310523276638520, -16.39321520033831447 ) ) ;
#44880 = CARTESIAN_POINT ( 'NONE',  ( 122.1743141859119817, -0.8832429491016019485, -18.19431474523657855 ) ) ;
#44881 = CARTESIAN_POINT ( 'NONE',  ( 109.1629577545248395, -2.791137627527939813, -18.39754474579286025 ) ) ;
#44882 = LINE ( 'NONE', #44426, #30588 ) ;
#44883 = CARTESIAN_POINT ( 'NONE',  ( 113.5337081442453240, -9.261995988541697145, -16.69588392320189030 ) ) ;
#44884 = CARTESIAN_POINT ( 'NONE',  ( 115.1220548109119761, -8.166667518702817929, -8.995218007635861213 ) ) ;
#44885 = CARTESIAN_POINT ( 'NONE',  ( 122.5215798109119874, -7.200787124940443817, -17.81845355600750835 ) ) ;
#44886 = CARTESIAN_POINT ( 'NONE',  ( 120.5074391859119913, -1.406689858478933353, -17.56299727309130887 ) ) ;
#44887 = ORIENTED_EDGE ( 'NONE', *, *, #21494, .T. ) ;
#44888 = LINE ( 'NONE', #5881, #10130 ) ;
#44889 = EDGE_LOOP ( 'NONE', ( #9792, #33532, #16921, #41120, #25755, #34660 ) ) ;
#44890 = CARTESIAN_POINT ( 'NONE',  ( 121.4187148109119789, -6.344957434206665248, -7.627207830600338134 ) ) ;
#44891 = CARTESIAN_POINT ( 'NONE',  ( 113.0798948109119948, -0.4660016031367893996, -10.09054647747474043 ) ) ;
#44892 = CARTESIAN_POINT ( 'NONE',  ( 117.0507614775786465, 0.1319031606808879209, -14.10382304977623669 ) ) ;
#44893 = CIRCLE ( 'NONE', #19377, 2.000000000000000444 ) ;
#44894 = CARTESIAN_POINT ( 'NONE',  ( 90.20794100481921873, -11.57440209418094668, -8.143215200338314474 ) ) ;
#44895 = CARTESIAN_POINT ( 'NONE',  ( 122.4965214775786251, -10.30919188438810075, -12.61870101168855918 ) ) ;
#44896 = CARTESIAN_POINT ( 'NONE',  ( 116.8238548109119819, -4.089484607189486809, -7.948022111789456723 ) ) ;
#44897 = EDGE_CURVE ( 'NONE', #22762, #42783, #27730, .T. ) ;
#44898 = CARTESIAN_POINT ( 'NONE',  ( 116.0388171295248014, -10.62599879583958540, -13.39321520033831447 ) ) ;
#44899 = CARTESIAN_POINT ( 'NONE',  ( 111.9453614775786434, -7.894159318335828068, -9.358103419637847864 ) ) ;
#44900 = CARTESIAN_POINT ( 'NONE',  ( 117.8659193777725278, -1.267766418764730840, -16.93314635290706605 ) ) ;
#44901 = ORIENTED_EDGE ( 'NONE', *, *, #35895, .T. ) ;
#44902 = ADVANCED_FACE ( 'NONE', ( #42636 ), #41965, .F. ) ;
#44903 = CARTESIAN_POINT ( 'NONE',  ( 117.8449348109119938, -8.166667518702817929, -8.995218007635861213 ) ) ;
#44904 = CONICAL_SURFACE ( 'NONE', #28875, 2.000000000000000444, 0.9599310885968830309 ) ;
#44905 = DIRECTION ( 'NONE',  ( -0.9908103287288505534, 0.1352586133457950035, 0.000000000000000000 ) ) ;
#44906 = CARTESIAN_POINT ( 'NONE',  ( 115.6325948109119821, 0.2603800115204892296, -16.42320221600525088 ) ) ;
#44907 = VERTEX_POINT ( 'NONE', #35085 ) ;
#44908 = CARTESIAN_POINT ( 'NONE',  ( 107.0793640045248196, 0.1403307496149616695, -15.46607636864997204 ) ) ;
#44909 = CARTESIAN_POINT ( 'NONE',  ( 123.8012348109119642, 0.2603800115204892296, -16.42320221600525088 ) ) ;
#44910 = CARTESIAN_POINT ( 'NONE',  ( 85.75809888461174069, -18.45227461768569199, -21.89321520033831447 ) ) ;
#44911 = CARTESIAN_POINT ( 'NONE',  ( 75.95778847736481509, -3.256761025687722189, -16.89321520033831447 ) ) ;
#44912 =( BOUNDED_CURVE ( )  B_SPLINE_CURVE ( 3, ( #4447, #28184, #16298, #33365 ),
 .UNSPECIFIED., .F., .T. ) 
 B_SPLINE_CURVE_WITH_KNOTS ( ( 4, 4 ),
 ( 1.570796326794895004, 2.466461120652760020 ),
 .UNSPECIFIED. ) 
 CURVE ( )  GEOMETRIC_REPRESENTATION_ITEM ( )  RATIONAL_B_SPLINE_CURVE ( ( 1.000000000000000000, 0.9342585459106650392, 0.9342585459106650392, 1.000000000000000000 ) ) 
 REPRESENTATION_ITEM ( '' )  );
#44913 = FACE_OUTER_BOUND ( 'NONE', #34427, .T. ) ;
#44914 = CARTESIAN_POINT ( 'NONE',  ( 117.3343948109119737, -6.222761293078241884, -8.102969835052219238 ) ) ;
#44915 = DIRECTION ( 'NONE',  ( -0.000000000000000000, -0.9284778069183720062, -0.3713878862591650232 ) ) ;
#44916 = CARTESIAN_POINT ( 'NONE',  ( 117.0507614775786465, 0.1319031606808879209, -14.10382304977623669 ) ) ;
#44917 = PLANE ( 'NONE',  #12140 ) ;
#44918 = AXIS2_PLACEMENT_3D ( 'NONE', #25652, #39556, #43645 ) ;
#44919 = CARTESIAN_POINT ( 'NONE',  ( 115.5191414775786569, -6.222761293078241884, -8.102969835052219238 ) ) ;
#44920 = CARTESIAN_POINT ( 'NONE',  ( 123.9106423109119675, -9.959231468620755479, -10.70263013195267199 ) ) ;
#44921 = CARTESIAN_POINT ( 'NONE',  ( 114.4413348109119823, -9.261995988541697145, -16.69588392320189030 ) ) ;
#44922 = CARTESIAN_POINT ( 'NONE',  ( 111.3780948109119890, -5.574606645277164318, -18.38911715685844683 ) ) ;
#44923 = CARTESIAN_POINT ( 'NONE',  ( 118.2420214775786320, -6.222761293078241884, -8.102969835052219238 ) ) ;
#44924 = ORIENTED_EDGE ( 'NONE', *, *, #16387, .F. ) ;
#44925 = CARTESIAN_POINT ( 'NONE',  ( 118.0151148109119816, -10.63000616557722466, -14.87417383870573495 ) ) ;
#44926 = CARTESIAN_POINT ( 'NONE',  ( 107.5655358795247736, -0.7896495226426338832, -17.46756447353520159 ) ) ;
#44927 = AXIS2_PLACEMENT_3D ( 'NONE', #23854, #6511, #20426 ) ;
#44928 = LINE ( 'NONE', #13686, #11019 ) ;
#44929 = CARTESIAN_POINT ( 'NONE',  ( 111.2646414775786496, -8.862178061932382889, -16.39564131203247399 ) ) ;
#44930 = CARTESIAN_POINT ( 'NONE',  ( 72.54180985774836188, -53.22909301380743585, -33.76528779565084903 ) ) ;
#44931 = CARTESIAN_POINT ( 'NONE',  ( 121.3052614775786111, -1.834011780172310813, -8.268836392978581529 ) ) ;
#44932 = ORIENTED_EDGE ( 'NONE', *, *, #44836, .T. ) ;
#44933 = CARTESIAN_POINT ( 'NONE',  ( 126.2184548109105435, -7.866424907533402511, -9.395035934245175469 ) ) ;
#44934 = CARTESIAN_POINT ( 'NONE',  ( 119.7736414775786358, 0.1319031606808879209, -14.10382304977623669 ) ) ;
#44935 = CARTESIAN_POINT ( 'NONE',  ( 123.2855641859119800, -0.8832429491016133838, -18.19431474523658565 ) ) ;
#44936 = ADVANCED_FACE ( 'NONE', ( #17565 ), #227, .T. ) ;
#44937 = AXIS2_PLACEMENT_3D ( 'NONE', #37129, #20729, #30985 ) ;
#44938 = CARTESIAN_POINT ( 'NONE',  ( 122.1561614775786353, -0.4660016031367893996, -10.09054647747474043 ) ) ;
#44939 = CARTESIAN_POINT ( 'NONE',  ( 106.3848327545248651, -2.477300249445798297, -19.15521520033831138 ) ) ;
#44940 = CARTESIAN_POINT ( 'NONE',  ( 124.5147686830089810, -1.087735405160626723, -17.17288456429612964 ) ) ;
#44941 = VERTEX_POINT ( 'NONE', #40334 ) ;
#44942 = FACE_OUTER_BOUND ( 'NONE', #43196, .T. ) ;
#44943 = CARTESIAN_POINT ( 'NONE',  ( 112.0020881442453344, 0.2603800115204892296, -16.42320221600525088 ) ) ;
#44944 = CARTESIAN_POINT ( 'NONE',  ( 123.8579614775786126, 0.5811942927096110934, -14.16772938898807510 ) ) ;
#44945 = CARTESIAN_POINT ( 'NONE',  ( 117.3911214775786505, -7.894159318335828068, -9.358103419637847864 ) ) ;
#44946 = CARTESIAN_POINT ( 'NONE',  ( 70.19189222814998175, -60.76597359474132531, -37.50918677187066663 ) ) ;
#44947 = CARTESIAN_POINT ( 'NONE',  ( 117.8449348109119938, -8.166667518702817929, -8.995218007635861213 ) ) ;
#44948 = DIRECTION ( 'NONE',  ( -0.8636456077245092677, 0.5040994586965584778, 0.000000000000000000 ) ) ;
#44949 = CARTESIAN_POINT ( 'NONE',  ( 123.4041481442452834, 0.1319031606808879209, -14.10382304977623669 ) ) ;
#44950 = ORIENTED_EDGE ( 'NONE', *, *, #42977, .T. ) ;
#44951 = DIRECTION ( 'NONE',  ( 0.5735764363510499342, 0.3127926500124801890, -0.7570804645221008711 ) ) ;
#44952 = ADVANCED_FACE ( 'NONE', ( #23233 ), #19132, .T. ) ;
#44953 = VECTOR ( 'NONE', #44850, 1000.000000000000000 ) ;
#44954 = CARTESIAN_POINT ( 'NONE',  ( 118.0718414775786300, -9.261995988541697145, -16.69588392320189030 ) ) ;
#44955 = CARTESIAN_POINT ( 'NONE',  ( 135.8419766445518633, -8.523023866441993945, -18.08927214266044103 ) ) ;
#44956 = EDGE_LOOP ( 'NONE', ( #34433, #20991, #30838, #25282 ) ) ;
#44957 = CARTESIAN_POINT ( 'NONE',  ( 123.7717360609119623, -6.564341423271550902, -7.887810678476487425 ) ) ;
#44958 = CARTESIAN_POINT ( 'NONE',  ( 62.98033575700867459, -12.60074217725106394, -10.22254757083790722 ) ) ;
#44959 = CARTESIAN_POINT ( 'NONE',  ( 122.4965214775786251, -10.30919188438810075, -12.61870101168855918 ) ) ;
#44960 = CARTESIAN_POINT ( 'NONE',  ( 109.5102233795247884, -8.938348069036489818, -17.46756447353520159 ) ) ;
#44961 = CARTESIAN_POINT ( 'NONE',  ( 120.1140014775786398, -7.894159318335828068, -9.358103419637847864 ) ) ;
#44962 = AXIS2_PLACEMENT_3D ( 'NONE', #19771, #29807, #43721 ) ;
#44963 = ORIENTED_EDGE ( 'NONE', *, *, #9703, .F. ) ;
#44964 = ORIENTED_EDGE ( 'NONE', *, *, #29837, .T. ) ;
#44965 = CARTESIAN_POINT ( 'NONE',  ( 115.8595014775786609, -1.834011780172310813, -8.268836392978581529 ) ) ;
#44966 = DIRECTION ( 'NONE',  ( 0.2397535688815952137, -0.1551785207689905521, -0.9583516332226319490 ) ) ;
#44967 = VECTOR ( 'NONE', #9748, 1000.000000000000114 ) ;
#44968 = DIRECTION ( 'NONE',  ( 0.000000000000000000, -0.4669533266896290225, -0.8842819633428516957 ) ) ;
#44969 = CARTESIAN_POINT ( 'NONE',  ( 123.0070614775786169, 0.9020085738987339008, -11.91225656197089222 ) ) ;
#44970 = LINE ( 'NONE', #1143, #3663 ) ;
#44971 = DIRECTION ( 'NONE',  ( 0.000000000000000000, 0.000000000000000000, -1.000000000000000000 ) ) ;
#44972 = CARTESIAN_POINT ( 'NONE',  ( 119.6034614775786196, -6.344957434206665248, -7.627207830600338134 ) ) ;
#44974 = CARTESIAN_POINT ( 'NONE',  ( 118.5823814775786360, -7.643976991954077427, -18.09477374809248928 ) ) ;
#44973 = CARTESIAN_POINT ( 'NONE',  ( 119.2631014775786298, 0.2603800115204892296, -16.42320221600525088 ) ) ;
#44975 = CARTESIAN_POINT ( 'NONE',  ( 125.4584548109119737, -8.702576499751430106, -17.94267422983053706 ) ) ;
#44976 = CARTESIAN_POINT ( 'NONE',  ( 117.7314814775786260, -4.089484607189486809, -7.948022111789456723 ) ) ;
#44977 = ORIENTED_EDGE ( 'NONE', *, *, #22011, .T. ) ;
#44978 = CARTESIAN_POINT ( 'NONE',  ( 126.2972081442452890, -2.084020599724406786, -8.691656652584148546 ) ) ;
#44979 = CARTESIAN_POINT ( 'NONE',  ( 125.3328548109119964, -0.8288870151393684660, -10.36305467784094247 ) ) ;
#44980 = CARTESIAN_POINT ( 'NONE',  ( 110.2742077545248094, -7.250697342233347165, -7.631215200338321125 ) ) ;
#44981 = CARTESIAN_POINT ( 'NONE',  ( 110.4825671295247815, 0.1403307496149613920, -13.39321520033831447 ) ) ;
#44982 = CARTESIAN_POINT ( 'NONE',  ( 106.5237390045248418, 0.8980012041604421569, -15.77991374673208469 ) ) ;
#44983 = CARTESIAN_POINT ( 'NONE',  ( 121.7023481442452777, -9.261995988541697145, -16.69588392320189030 ) ) ;
#44984 = CARTESIAN_POINT ( 'NONE',  ( 125.9001214775786224, -5.574606645277164318, -18.38911715685844683 ) ) ;
#44985 = ORIENTED_EDGE ( 'NONE', *, *, #35361, .F. ) ;
#44986 = CARTESIAN_POINT ( 'NONE',  ( 126.0135748109119902, -8.166667518702819706, -8.995218007635861213 ) ) ;
#44987 = CARTESIAN_POINT ( 'NONE',  ( 112.0799890045248475, 0.8980012041604421569, -15.77991374673208469 ) ) ;
#44988 = CARTESIAN_POINT ( 'NONE',  ( 60.11760374155740294, -14.70486118635416695, -19.35686119223085555 ) ) ;
#44989 = CARTESIAN_POINT ( 'NONE',  ( 124.0848681442452772, -4.089484607189486809, -7.948022111789456723 ) ) ;
#44990 = CARTESIAN_POINT ( 'NONE',  ( 123.7445081442452874, -1.561330072975668948, -17.79121239304076951 ) ) ;
#44991 = DIRECTION ( 'NONE',  ( 1.000000000000000000, 1.671245155169139691E-16, 0.000000000000000000 ) ) ;
#44992 = CARTESIAN_POINT ( 'NONE',  ( 126.5241148109119393, -9.565557343593413364, -10.61323700422348004 ) ) ;
#44993 = CARTESIAN_POINT ( 'NONE',  ( 111.5125327111057345, -1.267766418764825875, -16.93314635290698789 ) ) ;
#44994 = CARTESIAN_POINT ( 'NONE',  ( 107.5655358795247736, -0.7896495226426338832, -17.46756447353520159 ) ) ;
#44995 = VERTEX_POINT ( 'NONE', #1790 ) ;
#44996 = CARTESIAN_POINT ( 'NONE',  ( 77.25325688895158294, -4.012910213732562070, -7.993215200338315007 ) ) ;
#44997 = CARTESIAN_POINT ( 'NONE',  ( 114.3846081442453197, 0.4262465694468514643, -12.03445270309931736 ) ) ;
#44998 = CARTESIAN_POINT ( 'NONE',  ( 112.4559014775786494, -9.988377603198976828, -10.36322818467138340 ) ) ;
#44999 = CARTESIAN_POINT ( 'NONE',  ( 116.4555358795247884, -0.7896495226426338832, -17.46756447353520159 ) ) ;
#45000 = CARTESIAN_POINT ( 'NONE',  ( 108.9545983795247821, -8.402594152722688392, -16.93181055722141792 ) ) ;
#45001 = CARTESIAN_POINT ( 'NONE',  ( 121.8158014775786171, -4.153390946401325223, -8.397313243818185668 ) ) ;
#45002 = CARTESIAN_POINT ( 'NONE',  ( 116.0296814775786345, -1.833838273342658809, -17.42832698103878286 ) ) ;
#45003 = CARTESIAN_POINT ( 'NONE',  ( 111.4915481442453142, -1.833838273342658365, -17.42832698103878286 ) ) ;
#45004 = ORIENTED_EDGE ( 'NONE', *, *, #30653, .F. ) ;
#45005 = FACE_OUTER_BOUND ( 'NONE', #19644, .T. ) ;
#45006 = CARTESIAN_POINT ( 'NONE',  ( 118.2420214775786320, -3.383040157471821630, -19.15922257007629170 ) ) ;
#45007 = EDGE_CURVE ( 'NONE', #2614, #30977, #33822, .T. ) ;
#45008 = FACE_OUTER_BOUND ( 'NONE', #480, .T. ) ;
#45009 = CARTESIAN_POINT ( 'NONE',  ( 114.1577014775786552, -3.505236298600246325, -18.68346056562440793 ) ) ;
#45010 = VERTEX_POINT ( 'NONE', #15943 ) ;
#45011 = CARTESIAN_POINT ( 'NONE',  ( 90.25835095068887881, -11.48803753340850164, -14.14321520033831625 ) ) ;
#45012 = ORIENTED_EDGE ( 'NONE', *, *, #39499, .T. ) ;
#45013 = CARTESIAN_POINT ( 'NONE',  ( 113.4769814775786330, 0.4262465694468514643, -12.03445270309931736 ) ) ;
#45014 = VECTOR ( 'NONE', #18823, 1000.000000000000114 ) ;
#45015 = CARTESIAN_POINT ( 'NONE',  ( 115.4624148109119943, -4.153390946401321671, -8.397313243818183892 ) ) ;
#45016 = CARTESIAN_POINT ( 'NONE',  ( 117.7515727483929311, -2.423081321603731908, -17.89265170041263175 ) ) ;
#45017 = CARTESIAN_POINT ( 'NONE',  ( 122.7299391859119737, -1.406689858478933353, -17.56299727309130887 ) ) ;
#45018 = ORIENTED_EDGE ( 'NONE', *, *, #25431, .F. ) ;
#45019 = DIRECTION ( 'NONE',  ( -0.4461977533474358326, -0.3417300876246960328, 0.8271203734159366938 ) ) ;
#45020 = CARTESIAN_POINT ( 'NONE',  ( 124.9542645564595631, 1.996632241307949140, -10.07212650071240923 ) ) ;
#45021 = CARTESIAN_POINT ( 'NONE',  ( 113.6079577545248043, -7.250697342233347165, -7.631215200338321125 ) ) ;
#45022 = CARTESIAN_POINT ( 'NONE',  ( 118.2795432127138611, -2.191907684172563986, -18.20049396185734025 ) ) ;
#45023 = CARTESIAN_POINT ( 'NONE',  ( 124.0281414775786146, -7.643976991954077427, -18.09477374809248928 ) ) ;
#45024 = CARTESIAN_POINT ( 'NONE',  ( 114.8384214775786489, -10.15424416112533912, -14.75197769757731336 ) ) ;
#45025 = CARTESIAN_POINT ( 'NONE',  ( 120.1332064091100733, -0.9924539043446216624, -17.29976612834909133 ) ) ;
#45026 = ORIENTED_EDGE ( 'NONE', *, *, #27126, .F. ) ;
#45027 = DIRECTION ( 'NONE',  ( 1.000000000000000000, 0.000000000000000000, 0.000000000000000000 ) ) ;
#45028 = CARTESIAN_POINT ( 'NONE',  ( 117.4478481442453131, -9.565557343593413364, -10.61323700422348004 ) ) ;
#45029 = CARTESIAN_POINT ( 'NONE',  ( 86.04230958663551121, -25.82262605124140364, -8.393215200338314474 ) ) ;
#45030 = DIRECTION ( 'NONE',  ( 1.000000000000000000, 0.000000000000000000, 0.000000000000000000 ) ) ;
#45031 = CARTESIAN_POINT ( 'NONE',  ( 125.4463081442452932, -4.153390946401325223, -8.397313243818185668 ) ) ;
#45032 = B_SPLINE_CURVE_WITH_KNOTS ( 'NONE', 3,
 ( #39344, #11082, #4672, #15170, #7881, #25665, #7648, #32485, #21789, #42099 ),
 .UNSPECIFIED., .F., .F.,
 ( 4, 2, 2, 2, 4 ),
 ( 0.000000000000000000, 0.0005979257515333403529, 0.001195851503066680706, 0.001793777254600021059, 0.002391703006133361412 ),
 .UNSPECIFIED. ) ;
#45033 = ORIENTED_EDGE ( 'NONE', *, *, #43789, .F. ) ;
#45034 = CARTESIAN_POINT ( 'NONE',  ( 114.4980614775786592, -7.893985811506177619, -18.51759400769804742 ) ) ;
#45035 = DIRECTION ( 'NONE',  ( 1.000000000000000000, 0.000000000000000000, -0.000000000000000000 ) ) ;
#45036 = CARTESIAN_POINT ( 'NONE',  ( 107.6349890045248401, -9.868328341294098749, -11.32035403202665869 ) ) ;
#45037 = CARTESIAN_POINT ( 'NONE',  ( 126.6375681442452930, -10.15424416112533912, -14.75197769757731336 ) ) ;
#45038 = CARTESIAN_POINT ( 'NONE',  ( 115.4624148109119943, -5.638512984488999180, -18.83840828888717311 ) ) ;
#45039 = CARTESIAN_POINT ( 'NONE',  ( 122.0994348109119443, -10.15424416112533912, -14.75197769757731336 ) ) ;
#45040 = CARTESIAN_POINT ( 'NONE',  ( 112.4967077545247633, -2.791137627527887410, -18.39754474579284249 ) ) ;
#45041 = CARTESIAN_POINT ( 'NONE',  ( 111.2465515045248168, -6.936859964151250502, -18.39754474579286025 ) ) ;
#45042 = CARTESIAN_POINT ( 'NONE',  ( 111.2465515045248168, -2.477300249445798297, -7.631215200338310467 ) ) ;
#45043 = CARTESIAN_POINT ( 'NONE',  ( 119.9518141859119851, -8.321307733199551748, -9.223433127585318303 ) ) ;
#45044 = CARTESIAN_POINT ( 'NONE',  ( 116.6536748109119941, -10.15424416112533912, -14.75197769757731336 ) ) ;
#45045 = CARTESIAN_POINT ( 'NONE',  ( 105.9681140045248355, -10.62599879583958717, -11.00651665394454604 ) ) ;
#45046 = CIRCLE ( 'NONE', #7887, 2.445500000000004448 ) ;
#45047 = CARTESIAN_POINT ( 'NONE',  ( 111.7184548109119788, -9.244942279156937559, -16.71734234406761388 ) ) ;
#45048 = CARTESIAN_POINT ( 'NONE',  ( 109.3713171295247832, -10.62599879583958540, -13.39321520033831447 ) ) ;
#45049 = CARTESIAN_POINT ( 'NONE',  ( 123.6877814775786533, -3.383040157471821630, -19.15922257007629170 ) ) ;
#45050 = CARTESIAN_POINT ( 'NONE',  ( 112.3991748109119868, -1.833838273342658809, -17.42832698103878286 ) ) ;
#45051 = CARTESIAN_POINT ( 'NONE',  ( 73.07463722459043254, -57.36051141757233296, -35.25250588052404765 ) ) ;
#45052 = CARTESIAN_POINT ( 'NONE',  ( 121.5321681442453183, -9.988377603198976828, -10.36322818467138340 ) ) ;
#45053 = CARTESIAN_POINT ( 'NONE',  ( 116.1998614775786507, -10.63000616557722466, -14.87417383870573495 ) ) ;
#45054 = VERTEX_POINT ( 'NONE', #36445 ) ;
#45055 = CARTESIAN_POINT ( 'NONE',  ( 114.3846081442453197, 0.4262465694468514643, -12.03445270309931736 ) ) ;
#45056 = CARTESIAN_POINT ( 'NONE',  ( 124.5954081442453116, -3.383040157471821630, -19.15922257007629170 ) ) ;
#45057 = CARTESIAN_POINT ( 'NONE',  ( 114.7249681442453237, 0.2603800115204892296, -16.42320221600525088 ) ) ;
#45058 = CARTESIAN_POINT ( 'NONE',  ( 115.5191414775786569, -6.222761293078241884, -8.102969835052219238 ) ) ;
#45059 = VERTEX_POINT ( 'NONE', #2240 ) ;
#45060 = CARTESIAN_POINT ( 'NONE',  ( 120.1140014775786398, -7.894159318335828068, -9.358103419637847864 ) ) ;
#45061 = CARTESIAN_POINT ( 'NONE',  ( 116.4834948109119779, -1.561330072975668504, -17.79121239304076951 ) ) ;
#45062 = CARTESIAN_POINT ( 'NONE',  ( 116.8382249924907086, -1.095796847231273130, -17.04019780263804762 ) ) ;
#45063 = CARTESIAN_POINT ( 'NONE',  ( 115.2748327545248657, -2.477300249445798297, -19.15521520033831138 ) ) ;
#45064 = ORIENTED_EDGE ( 'NONE', *, *, #35159, .F. ) ;
#45065 = CARTESIAN_POINT ( 'NONE',  ( 111.7184548109119788, -9.261995988541697145, -16.69588392320189030 ) ) ;
#45066 = CARTESIAN_POINT ( 'NONE',  ( 111.7184548109119788, -9.244942279156937559, -16.71734234406761388 ) ) ;
#45067 = DIRECTION ( 'NONE',  ( 0.000000000000000000, 0.000000000000000000, -1.000000000000000000 ) ) ;
#45068 = CARTESIAN_POINT ( 'NONE',  ( 113.4769814775786330, -10.63000616557722466, -14.87417383870573495 ) ) ;
#45069 = DIRECTION ( 'NONE',  ( 0.000000000000000000, 0.4669533266896289669, 0.8842819633428518067 ) ) ;
#45070 = CARTESIAN_POINT ( 'NONE',  ( 113.6471614775786492, -4.153390946401321671, -8.397313243818183892 ) ) ;
#45071 = CARTESIAN_POINT ( 'NONE',  ( 62.20960312368780620, -12.49232639468414163, -16.90032038405202997 ) ) ;
#45072 = CARTESIAN_POINT ( 'NONE',  ( 69.69189222814998175, -41.76310523276723785, -6.393215200338315363 ) ) ;
#45073 = CARTESIAN_POINT ( 'NONE',  ( 115.4831921295247952, -9.868328341294093420, -13.39321520033831447 ) ) ;
#45074 = CARTESIAN_POINT ( 'NONE',  ( 117.2209414775786485, -7.893985811506177619, -18.51759400769804742 ) ) ;
#45075 = CARTESIAN_POINT ( 'NONE',  ( 136.8676504264525988, -4.417203549486936609, -18.92742781940280850 ) ) ;
#45076 = CARTESIAN_POINT ( 'NONE',  ( 94.20708369096698220, -25.28273535805287864, -12.54175975618893091 ) ) ;
#45078 = B_SPLINE_CURVE_WITH_KNOTS ( 'NONE', 3,
 ( #28932, #11600, #25510, #22088, #4747, #18667, #43966, #13412, #20021, #24120, #26633, #40546, #19563, #38014, #9993, #26858, #3136, #41009, #34136, #33904, #12730, #2219, #9763, #33440, #16149, #30053, #23674, #10212, #27088, #37094, #9529, #23445, #27316, #9307 ),
 .UNSPECIFIED., .F., .F.,
 ( 4, 2, 2, 2, 2, 2, 1, 1, 2, 2, 2, 2, 1, 1, 2, 2, 2, 2, 4 ),
 ( 0.000000000000000000, 0.06249999999997646327, 0.09374999999996487532, 0.1249999999999532874, 0.1874999999999158173, 0.2187499999998893940, 0.2343749999998761824, 0.2421874999998695766, 0.2460937499998662736, 0.2499999999998629707, 0.3749999999998242517, 0.4374999999998063216, 0.4687499999997993272, 0.4843749999998045452, 0.4921874999997982725, 0.4999999999997919997, 0.6249999999998440137, 0.7499999999998959721, 1.000000000000000000 ),
 .UNSPECIFIED. ) ;
#45077 = CARTESIAN_POINT ( 'NONE',  ( 118.8660148109119774, -10.30919188438809719, -12.61870101168856273 ) ) ;
#45079 = CARTESIAN_POINT ( 'NONE',  ( 121.8725281442453223, -6.222761293078241884, -8.102969835052219238 ) ) ;
#45080 = EDGE_LOOP ( 'NONE', ( #4795, #36590, #36902, #21460, #36898, #8991 ) ) ;
#45081 = CARTESIAN_POINT ( 'NONE',  ( 135.8419766445417736, -9.560055738161365113, -9.734190129735562635 ) ) ;
#45082 = CARTESIAN_POINT ( 'NONE',  ( 119.7169148109119874, -9.988377603198976828, -10.36322818467138340 ) ) ;
#45083 = DIRECTION ( 'NONE',  ( -0.8636456077245092677, 0.5040994586965584778, 0.000000000000000000 ) ) ;
#45084 = CARTESIAN_POINT ( 'NONE',  ( 116.7104014775786425, -8.899110576539710493, -16.42337572283490132 ) ) ;
#45085 =( BOUNDED_SURFACE ( )  B_SPLINE_SURFACE ( 1, 2, ( 
 ( #11280, #27941, #41851, #21082, #21535, #35653, #38616, #24728, #31565, #32009, #28610, #10611, #18116, #35422, #14696, #34747, #42519, #4427, #7393, #11509, #21311, #1007, #31340, #38399, #28379, #25188, #39086, #114, #42292, #17892, #14027, #7855, #14923, #28834, #11054, #42744, #25413, #34959, #3747, #334, #14247, #1891, #1233, #12638, #36102, #19459, #25852, #39758, #15593, #42959, #22877, #43190, #5542, #33122, #1449, #36771, #1670, #18566, #15819, #11954, #15145, #8528, #4644, #32680, #2115, #32458, #43631, #33342, #16045, #18791, #26306, #19008, #22430, #35873, #8082, #29951, #26534, #29052, #15370, #19239, #21984, #26078, #29274, #11726, #39543, #43866, #36323, #25640, #8304, #22653, #29718, #8979, #22206, #29496, #4873, #12405, #32894, #36549, #5092, #43410, #12177, #39982, #40214, #8747, #5323, #23578, #3038, #24025, #10122, #40904, #13086, #16278, #12863, #37694, #33571, #13759, #9658, #30180, #16734, #34038, #30630, #41366, #19919, #44098, #16960, #6467, #37222, #44546, #30854, #23337, #37914, #6691, #26763, #37460, #6233, #20155, #2576, #16506, #13310, #20603, #40672, #2807, #9424, #34478, #23806, #3257, #17182, #2347, #5996, #27217, #33805, #30405, #31072, #44327, #26984, #41135, #20377, #9894, #34263, #44777, #13536 ),
 ( #27444, #40444, #44999, #9206, #23115, #36992, #5762, #19683, #17839, #3484, #27668, #31736, #62, #41581, #24677, #38565, #42016, #20818, #24244, #10340, #17400, #6908, #3699, #506, #10781, #28112, #3920, #31289, #13975, #27888, #7341, #14417, #21036, #7125, #41802, #21260, #35140, #10560, #28327, #38137, #34697, #24457, #38349, #34909, #17619, #31512, #284, #14194, #28439, #14526, #20927, #18170, #14080, #39374, #35248, #41903, #42352, #11111, #25013, #21815, #390, #10668, #42571, #32067, #17723, #38906, #11334, #3797, #4484, #35708, #24571, #4025, #31846, #615, #28221, #42128, #7677, #32297, #7227, #21592, #35017, #1062, #4253, #18405, #28890, #27998, #38456, #35479, #21141, #31621, #14977, #14303, #10888, #835, #14754, #24787, #17947, #28667, #25245, #39143, #42802, #38679, #11563, #7908, #25470, #34801, #7445, #3585, #21365, #17496, #31395, #164, #25914, #39819, #15651, #43016, #22935, #43246, #5597, #33177, #1507, #36828, #1729, #18624, #15880, #12012, #15201, #8586, #4704, #32733, #29555, #43472, #9038, #15427, #29105, #29777, #19299, #4927, #12238, #43688, #36158, #19521, #33398, #11785, #22486, #19068, #32952, #29332, #36380, #26135, #2172, #39599, #40039, #22264, #16102, #36607, #30005, #43921, #1289, #25692, #8805 ) ),
 .UNSPECIFIED., .F., .F., .T. ) 
 B_SPLINE_SURFACE_WITH_KNOTS ( ( 2, 2 ),
 ( 3, 2, 2, 2, 2, 2, 2, 2, 2, 2, 2, 2, 2, 2, 2, 2, 2, 2, 2, 2, 2, 2, 2, 2, 2, 2, 2, 2, 2, 2, 2, 2, 2, 2, 2, 2, 2, 2, 2, 2, 2, 2, 2, 2, 2, 2, 2, 2, 2, 2, 2, 2, 2, 2, 2, 2, 2, 2, 2, 2, 2, 2, 2, 2, 2, 2, 2, 2, 2, 2, 2, 2, 2, 2, 2, 2, 2, 2, 2, 2, 3 ),
 ( 0.000000000000000000, 1.000000000000000000 ),
 ( 0.000000000000000000, 0.01250000000000000069, 0.02500000000000000139, 0.03749999999999999861, 0.05000000000000000278, 0.06250000000000000000, 0.07499999999999999722, 0.08749999999999999445, 0.1000000000000000056, 0.1125000000000000028, 0.1250000000000000000, 0.1375000000000000111, 0.1499999999999999944, 0.1625000000000000056, 0.1749999999999999889, 0.1875000000000000000, 0.2000000000000000111, 0.2124999999999999944, 0.2250000000000000056, 0.2374999999999999889, 0.2500000000000000000, 0.2625000000000000111, 0.2750000000000000222, 0.2874999999999999778, 0.2999999999999999889, 0.3125000000000000000, 0.3250000000000000111, 0.3375000000000000222, 0.3499999999999999778, 0.3624999999999999889, 0.3750000000000000000, 0.3875000000000000111, 0.4000000000000000222, 0.4124999999999999778, 0.4249999999999999889, 0.4375000000000000000, 0.4500000000000000111, 0.4625000000000000222, 0.4749999999999999778, 0.4874999999999999889, 0.5000000000000000000, 0.5124999999999999556, 0.5250000000000000222, 0.5374999999999999778, 0.5500000000000000444, 0.5625000000000000000, 0.5749999999999999556, 0.5875000000000000222, 0.5999999999999999778, 0.6125000000000000444, 0.6250000000000000000, 0.6374999999999999556, 0.6500000000000000222, 0.6624999999999999778, 0.6750000000000000444, 0.6875000000000000000, 0.6999999999999999556, 0.7125000000000000222, 0.7249999999999999778, 0.7375000000000000444, 0.7500000000000000000, 0.7624999999999999556, 0.7750000000000000222, 0.7874999999999999778, 0.8000000000000000444, 0.8125000000000000000, 0.8249999999999999556, 0.8375000000000000222, 0.8499999999999999778, 0.8625000000000000444, 0.8750000000000000000, 0.8874999999999999556, 0.9000000000000000222, 0.9124999999999999778, 0.9250000000000000444, 0.9375000000000000000, 0.9499999999999999556, 0.9625000000000000222, 0.9749999999999999778, 0.9875000000000000444, 1.000000000000000000 ),
 .UNSPECIFIED. ) 
 GEOMETRIC_REPRESENTATION_ITEM ( )  RATIONAL_B_SPLINE_SURFACE ( (
 ( 1.000000000000000000, 0.9238795325112869605, 1.000000000000000000, 0.9238795325112869605, 1.000000000000000000, 0.9238795325112869605, 1.000000000000000000, 0.9238795325112869605, 1.000000000000000000, 0.9238795325112869605, 1.000000000000000000, 0.9238795325112869605, 1.000000000000000000, 0.9238795325112869605, 1.000000000000000000, 0.9238795325112869605, 1.000000000000000000, 0.9238795325112869605, 1.000000000000000000, 0.9238795325112869605, 1.000000000000000000, 0.9238795325112869605, 1.000000000000000000, 0.9238795325112869605, 1.000000000000000000, 0.9238795325112869605, 1.000000000000000000, 0.9238795325112869605, 1.000000000000000000, 0.9238795325112869605, 1.000000000000000000, 0.9238795325112869605, 1.000000000000000000, 0.9238795325112869605, 1.000000000000000000, 0.9238795325112869605, 1.000000000000000000, 0.9238795325112869605, 1.000000000000000000, 0.9238795325112869605, 1.000000000000000000, 0.9238795325112869605, 1.000000000000000000, 0.9238795325112869605, 1.000000000000000000, 0.9238795325112869605, 1.000000000000000000, 0.9238795325112869605, 1.000000000000000000, 0.9238795325112869605, 1.000000000000000000, 0.9238795325112869605, 1.000000000000000000, 0.9238795325112869605, 1.000000000000000000, 0.9238795325112869605, 1.000000000000000000, 0.9238795325112869605, 1.000000000000000000, 0.9238795325112869605, 1.000000000000000000, 0.9238795325112869605, 1.000000000000000000, 0.9238795325112869605, 1.000000000000000000, 0.9238795325112869605, 1.000000000000000000, 0.9238795325112869605, 1.000000000000000000, 0.9238795325112869605, 1.000000000000000000, 0.9238795325112869605, 1.000000000000000000, 0.9238795325112869605, 1.000000000000000000, 0.9238795325112869605, 1.000000000000000000, 0.9238795325112869605, 1.000000000000000000, 0.9238795325112869605, 1.000000000000000000, 0.9238795325112869605, 1.000000000000000000, 0.9238795325112869605, 1.000000000000000000, 0.9238795325112869605, 1.000000000000000000, 0.9238795325112869605, 1.000000000000000000, 0.9238795325112869605, 1.000000000000000000, 0.9238795325112869605, 1.000000000000000000, 0.9238795325112869605, 1.000000000000000000, 0.9238795325112869605, 1.000000000000000000, 0.9238795325112869605, 1.000000000000000000, 0.9238795325112869605, 1.000000000000000000, 0.9238795325112869605, 1.000000000000000000, 0.9238795325112869605, 1.000000000000000000, 0.9238795325112869605, 1.000000000000000000, 0.9238795325112869605, 1.000000000000000000, 0.9238795325112869605, 1.000000000000000000, 0.9238795325112869605, 1.000000000000000000, 0.9238795325112869605, 1.000000000000000000, 0.9238795325112869605, 1.000000000000000000, 0.9238795325112869605, 1.000000000000000000, 0.9238795325112869605, 1.000000000000000000, 0.9238795325112869605, 1.000000000000000000, 0.9238795325112869605, 1.000000000000000000, 0.9238795325112869605, 1.000000000000000000, 0.9238795325112869605, 1.000000000000000000, 0.9238795325112869605, 1.000000000000000000, 0.9238795325112869605, 1.000000000000000000, 0.9238795325112869605, 1.000000000000000000, 0.9238795325112869605, 1.000000000000000000, 0.9238795325112869605, 1.000000000000000000, 0.9238795325112869605, 1.000000000000000000, 0.9238795325112869605, 1.000000000000000000, 0.9238795325112869605, 1.000000000000000000, 0.9238795325112869605, 1.000000000000000000, 0.9238795325112869605, 1.000000000000000000, 0.9238795325112869605, 1.000000000000000000, 0.9238795325112869605, 1.000000000000000000, 0.9238795325112869605, 1.000000000000000000, 0.9238795325112869605, 1.000000000000000000, 0.9238795325112869605, 1.000000000000000000, 0.9238795325112869605, 1.000000000000000000),
 ( 1.000000000000000000, 0.9238795325112869605, 1.000000000000000000, 0.9238795325112869605, 1.000000000000000000, 0.9238795325112869605, 1.000000000000000000, 0.9238795325112869605, 1.000000000000000000, 0.9238795325112869605, 1.000000000000000000, 0.9238795325112869605, 1.000000000000000000, 0.9238795325112869605, 1.000000000000000000, 0.9238795325112869605, 1.000000000000000000, 0.9238795325112869605, 1.000000000000000000, 0.9238795325112869605, 1.000000000000000000, 0.9238795325112869605, 1.000000000000000000, 0.9238795325112869605, 1.000000000000000000, 0.9238795325112869605, 1.000000000000000000, 0.9238795325112869605, 1.000000000000000000, 0.9238795325112869605, 1.000000000000000000, 0.9238795325112869605, 1.000000000000000000, 0.9238795325112869605, 1.000000000000000000, 0.9238795325112869605, 1.000000000000000000, 0.9238795325112869605, 1.000000000000000000, 0.9238795325112869605, 1.000000000000000000, 0.9238795325112869605, 1.000000000000000000, 0.9238795325112869605, 1.000000000000000000, 0.9238795325112869605, 1.000000000000000000, 0.9238795325112869605, 1.000000000000000000, 0.9238795325112869605, 1.000000000000000000, 0.9238795325112869605, 1.000000000000000000, 0.9238795325112869605, 1.000000000000000000, 0.9238795325112869605, 1.000000000000000000, 0.9238795325112869605, 1.000000000000000000, 0.9238795325112869605, 1.000000000000000000, 0.9238795325112869605, 1.000000000000000000, 0.9238795325112869605, 1.000000000000000000, 0.9238795325112869605, 1.000000000000000000, 0.9238795325112869605, 1.000000000000000000, 0.9238795325112869605, 1.000000000000000000, 0.9238795325112869605, 1.000000000000000000, 0.9238795325112869605, 1.000000000000000000, 0.9238795325112869605, 1.000000000000000000, 0.9238795325112869605, 1.000000000000000000, 0.9238795325112869605, 1.000000000000000000, 0.9238795325112869605, 1.000000000000000000, 0.9238795325112869605, 1.000000000000000000, 0.9238795325112869605, 1.000000000000000000, 0.9238795325112869605, 1.000000000000000000, 0.9238795325112869605, 1.000000000000000000, 0.9238795325112869605, 1.000000000000000000, 0.9238795325112869605, 1.000000000000000000, 0.9238795325112869605, 1.000000000000000000, 0.9238795325112869605, 1.000000000000000000, 0.9238795325112869605, 1.000000000000000000, 0.9238795325112869605, 1.000000000000000000, 0.9238795325112869605, 1.000000000000000000, 0.9238795325112869605, 1.000000000000000000, 0.9238795325112869605, 1.000000000000000000, 0.9238795325112869605, 1.000000000000000000, 0.9238795325112869605, 1.000000000000000000, 0.9238795325112869605, 1.000000000000000000, 0.9238795325112869605, 1.000000000000000000, 0.9238795325112869605, 1.000000000000000000, 0.9238795325112869605, 1.000000000000000000, 0.9238795325112869605, 1.000000000000000000, 0.9238795325112869605, 1.000000000000000000, 0.9238795325112869605, 1.000000000000000000, 0.9238795325112869605, 1.000000000000000000, 0.9238795325112869605, 1.000000000000000000, 0.9238795325112869605, 1.000000000000000000, 0.9238795325112869605, 1.000000000000000000, 0.9238795325112869605, 1.000000000000000000, 0.9238795325112869605, 1.000000000000000000, 0.9238795325112869605, 1.000000000000000000, 0.9238795325112869605, 1.000000000000000000, 0.9238795325112869605, 1.000000000000000000, 0.9238795325112869605, 1.000000000000000000, 0.9238795325112869605, 1.000000000000000000, 0.9238795325112869605, 1.000000000000000000, 0.9238795325112869605, 1.000000000000000000, 0.9238795325112869605, 1.000000000000000000, 0.9238795325112869605, 1.000000000000000000, 0.9238795325112869605, 1.000000000000000000, 0.9238795325112869605, 1.000000000000000000) ) ) 
 REPRESENTATION_ITEM ( '' )  SURFACE ( )  );
#45086 = EDGE_CURVE ( 'NONE', #24250, #9155, #36668, .T. ) ;
#45087 = EDGE_CURVE ( 'NONE', #6720, #19850, #22547, .T. ) ;
#45088 = CARTESIAN_POINT ( 'NONE',  ( 113.6471614775786492, -4.153390946401321671, -8.397313243818183892 ) ) ;
#45089 = CARTESIAN_POINT ( 'NONE',  ( 110.2742077545248094, -7.250697342233347165, -7.631215200338321125 ) ) ;
#45090 = CARTESIAN_POINT ( 'NONE',  ( 106.1070202545248407, 0.1403307496149616695, -11.32035403202665336 ) ) ;
#45091 = CARTESIAN_POINT ( 'NONE',  ( 113.3995983795247895, -0.7896495226426338832, -9.318865927141430916 ) ) ;
#45092 = CARTESIAN_POINT ( 'NONE',  ( 120.5110881442453206, -3.505236298600246325, -18.68346056562440793 ) ) ;
#45093 = CARTESIAN_POINT ( 'NONE',  ( 121.6456214775786293, 0.4262465694468514643, -12.03445270309931736 ) ) ;
#45094 = CARTESIAN_POINT ( 'NONE',  ( 124.3968141859119783, -8.321307733199551748, -9.223433127585318303 ) ) ;
#45095 = CARTESIAN_POINT ( 'NONE',  ( 88.46631044337289040, -25.99489077589524300, -13.39321520033831625 ) ) ;
#45096 = CARTESIAN_POINT ( 'NONE',  ( 110.4131140045248287, 0.1403307496149616695, -15.46607636864997204 ) ) ;
#45097 = LINE ( 'NONE', #33910, #24792 ) ;
#45098 = CARTESIAN_POINT ( 'NONE',  ( 112.9664414775786412, 0.5811942927096154232, -14.16772938898807155 ) ) ;
#45099 = CARTESIAN_POINT ( 'NONE',  ( 114.2711548109119803, -9.988377603198976828, -10.36322818467138340 ) ) ;
#45100 = LINE ( 'NONE', #13857, #11898 ) ;
#45101 = ORIENTED_EDGE ( 'NONE', *, *, #3140, .T. ) ;
#45102 = FACE_OUTER_BOUND ( 'NONE', #404, .T. ) ;
#45103 = ORIENTED_EDGE ( 'NONE', *, *, #36564, .T. ) ;
#45104 = CARTESIAN_POINT ( 'NONE',  ( 120.9081748109119872, -5.638512984488999180, -18.83840828888717311 ) ) ;
#45105 = CARTESIAN_POINT ( 'NONE',  ( 126.2972081442452890, -2.084020599724406786, -8.691656652584148546 ) ) ;
#45106 = CARTESIAN_POINT ( 'NONE',  ( 118.5256548109119876, -8.899110576539710493, -16.42337572283490132 ) ) ;
#45107 =( NAMED_UNIT ( * ) PLANE_ANGLE_UNIT ( ) SI_UNIT ( $, .RADIAN. ) );
#45108 = CARTESIAN_POINT ( 'NONE',  ( 120.2532105243962235, -8.246645307473400521, -17.07926517626395224 ) ) ;
#45109 = VECTOR ( 'NONE', #42060, 1000.000000000000000 ) ;
#45110 = CARTESIAN_POINT ( 'NONE',  ( 122.2696148109119889, -4.089484607189486809, -7.948022111789456723 ) ) ;
#45111 = CARTESIAN_POINT ( 'NONE',  ( 118.2420214775786320, -3.383040157471821630, -19.15922257007629170 ) ) ;
#45112 = EDGE_CURVE ( 'NONE', #36034, #16480, #2019, .T. ) ;
#45113 = CARTESIAN_POINT ( 'NONE',  ( 107.1488171295247867, 0.1403307496149613920, -13.39321520033831447 ) ) ;
#45114 = CARTESIAN_POINT ( 'NONE',  ( 114.2711548109119803, -0.1624402480850797581, -16.17319339645315424 ) ) ;
#45115 = CARTESIAN_POINT ( 'NONE',  ( 91.11246428952674137, -27.84333996136784961, -14.15691383771150136 ) ) ;
#45116 = ORIENTED_EDGE ( 'NONE', *, *, #20330, .T. ) ;
#45117 = CARTESIAN_POINT ( 'NONE',  ( 118.8092881442453290, -9.988377603198976828, -10.36322818467138340 ) ) ;
#45118 = EDGE_CURVE ( 'NONE', #8883, #40452, #36285, .T. ) ;
#45119 = DIRECTION ( 'NONE',  ( -0.000000000000000000, -0.9284778069183718952, -0.3713878862591649677 ) ) ;
#45120 = EDGE_CURVE ( 'NONE', #2844, #35171, #27393, .T. ) ;
#45121 = CARTESIAN_POINT ( 'NONE',  ( 114.6682414775786469, -1.561330072975668060, -17.79121239304076596 ) ) ;
#45122 = ORIENTED_EDGE ( 'NONE', *, *, #39925, .F. ) ;
#45123 = CARTESIAN_POINT ( 'NONE',  ( 114.1635827545248389, -2.477300249445798297, -19.15521520033831138 ) ) ;
#45124 = CARTESIAN_POINT ( 'NONE',  ( 123.5743281442453139, -7.893985811506177619, -18.51759400769804742 ) ) ;
#45125 = LINE ( 'NONE', #17314, #481 ) ;
#45126 = CARTESIAN_POINT ( 'NONE',  ( 135.3184548109119874, -4.863998795839242995, -13.39321520033831447 ) ) ;
#45127 = DIRECTION ( 'NONE',  ( 0.000000000000000000, 0.000000000000000000, 1.000000000000000000 ) ) ;
#45128 = CARTESIAN_POINT ( 'NONE',  ( 117.6180281442453150, -8.899110576539710493, -16.42337572283490132 ) ) ;
#45129 = DIRECTION ( 'NONE',  ( 3.317300593186674996E-33, -1.668003342285379964E-16, 1.000000000000000000 ) ) ;
#45130 = ADVANCED_FACE ( 'NONE', ( #23000 ), #24860, .T. ) ;
#45131 = CARTESIAN_POINT ( 'NONE',  ( 118.1285681442453068, -2.084020599724406786, -8.691656652584148546 ) ) ;
#45132 = CIRCLE ( 'NONE', #16733, 4.500000000000000888 ) ;
#45133 = DIRECTION ( 'NONE',  ( 1.000000000000000000, 0.000000000000000000, -0.000000000000000000 ) ) ;
#45134 = CARTESIAN_POINT ( 'NONE',  ( 118.0718414775786442, -0.8288870151387760510, -10.36305467784173118 ) ) ;
#45135 = EDGE_CURVE ( 'NONE', #31317, #35799, #7510, .T. ) ;
#45136 = CARTESIAN_POINT ( 'NONE',  ( 123.2855641859119942, -0.8832429491016019485, -18.19431474523657855 ) ) ;
#45137 = CARTESIAN_POINT ( 'NONE',  ( 114.6682414775786469, -1.561330072975668060, -17.79121239304076596 ) ) ;
#45138 = EDGE_CURVE ( 'NONE', #23460, #32855, #31735, .T. ) ;
#45139 = EDGE_CURVE ( 'NONE', #6063, #38699, #23809, .T. ) ;
#45140 = CARTESIAN_POINT ( 'NONE',  ( 116.4834948109119779, -7.894159318335828068, -9.358103419637847864 ) ) ;
#45141 = ORIENTED_EDGE ( 'NONE', *, *, #21941, .F. ) ;
#45142 = CARTESIAN_POINT ( 'NONE',  ( 118.5256548109119876, -0.4660016031367893996, -10.09054647747474043 ) ) ;
#45143 = CARTESIAN_POINT ( 'NONE',  ( 105.6208483795248299, -0.7896495226426338832, -9.318865927141430916 ) ) ;
#45144 = CARTESIAN_POINT ( 'NONE',  ( 115.1430393777725385, -1.267766418764730840, -16.93314635290706605 ) ) ;
#45145 = DIRECTION ( 'NONE',  ( 0.000000000000000000, 0.9284778069183720062, 0.3713878862591650232 ) ) ;
#45146 = AXIS2_PLACEMENT_3D ( 'NONE', #1804, #2257, #40810 ) ;
#45147 = CARTESIAN_POINT ( 'NONE',  ( 113.3954021944299768, 0.6269505268395592079, -12.14321520033829849 ) ) ;
#45148 = CARTESIAN_POINT ( 'NONE',  ( 123.5743281442453139, -7.893985811506177619, -18.51759400769804742 ) ) ;
#45149 = NEXT_ASSEMBLY_USAGE_OCCURRENCE ( 'NAUO1', ' ', ' ', #24145, #16477, $ ) ;
#45150 = NEXT_ASSEMBLY_USAGE_OCCURRENCE ( 'NAUO2', ' ', ' ', #24145, #15653, $ ) ;
#45151 = NEXT_ASSEMBLY_USAGE_OCCURRENCE ( 'NAUO3', ' ', ' ', #24145, #10357, $ ) ;
#45152 = NEXT_ASSEMBLY_USAGE_OCCURRENCE ( 'NAUO4', ' ', ' ', #24145, #9359, $ ) ;
#45153 = NEXT_ASSEMBLY_USAGE_OCCURRENCE ( 'NAUO5', ' ', ' ', #24145, #33583, $ ) ;
#45154 = NEXT_ASSEMBLY_USAGE_OCCURRENCE ( 'NAUO6', ' ', ' ', #24145, #12711, $ ) ;
#45155 = NEXT_ASSEMBLY_USAGE_OCCURRENCE ( 'NAUO7', ' ', ' ', #24145, #7964, $ ) ;
#45156=COLOUR_RGB('Dark Blue',0.08,0.2,0.34);
#45157=FILL_AREA_STYLE_COLOUR('',#45156);
#45158=FILL_AREA_STYLE('',(#45157));
#45159=SURFACE_STYLE_FILL_AREA(#45158);
#45160=SURFACE_SIDE_STYLE('',(#45159));
#45161=SURFACE_STYLE_USAGE(.BOTH.,#45160);
#45162=PRESENTATION_STYLE_ASSIGNMENT((#45161));
#45163=COLOUR_RGB('Light Blue',0.38,0.62,0.78);
#45164=FILL_AREA_STYLE_COLOUR('',#45163);
#45165=FILL_AREA_STYLE('',(#45164));
#45166=SURFACE_STYLE_FILL_AREA(#45165);
#45167=SURFACE_SIDE_STYLE('',(#45166));
#45168=SURFACE_STYLE_USAGE(.BOTH.,#45167);
#45169=PRESENTATION_STYLE_ASSIGNMENT((#45168));
#45170=COLOUR_RGB('Sky Blue',0.24,0.69,0.87);
#45171=FILL_AREA_STYLE_COLOUR('',#45170);
#45172=FILL_AREA_STYLE('',(#45171));
#45173=SURFACE_STYLE_FILL_AREA(#45172);
#45174=SURFACE_SIDE_STYLE('',(#45173));
#45175=SURFACE_STYLE_USAGE(.BOTH.,#45174);
#45176=PRESENTATION_STYLE_ASSIGNMENT((#45175));
#45177=COLOUR_RGB('Grey',0.48,0.52,0.57);
#45178=FILL_AREA_STYLE_COLOUR('',#45177);
#45179=FILL_AREA_STYLE('',(#45178));
#45180=SURFACE_STYLE_FILL_AREA(#45179);
#45181=SURFACE_SIDE_STYLE('',(#45180));
#45182=SURFACE_STYLE_USAGE(.BOTH.,#45181);
#45183=PRESENTATION_STYLE_ASSIGNMENT((#45182));
#45184=COLOUR_RGB('Black',0.12,0.14,0.17);
#45185=FILL_AREA_STYLE_COLOUR('',#45184);
#45186=FILL_AREA_STYLE('',(#45185));
#45187=SURFACE_STYLE_FILL_AREA(#45186);
#45188=SURFACE_SIDE_STYLE('',(#45187));
#45189=SURFACE_STYLE_USAGE(.BOTH.,#45188);
#45190=PRESENTATION_STYLE_ASSIGNMENT((#45189));
#45191=COLOUR_RGB('Off White',0.89,0.88,0.83);
#45192=FILL_AREA_STYLE_COLOUR('',#45191);
#45193=FILL_AREA_STYLE('',(#45192));
#45194=SURFACE_STYLE_FILL_AREA(#45193);
#45195=SURFACE_SIDE_STYLE('',(#45194));
#45196=SURFACE_STYLE_USAGE(.BOTH.,#45195);
#45197=PRESENTATION_STYLE_ASSIGNMENT((#45196));
ENDSEC;
END-ISO-10303-21;
